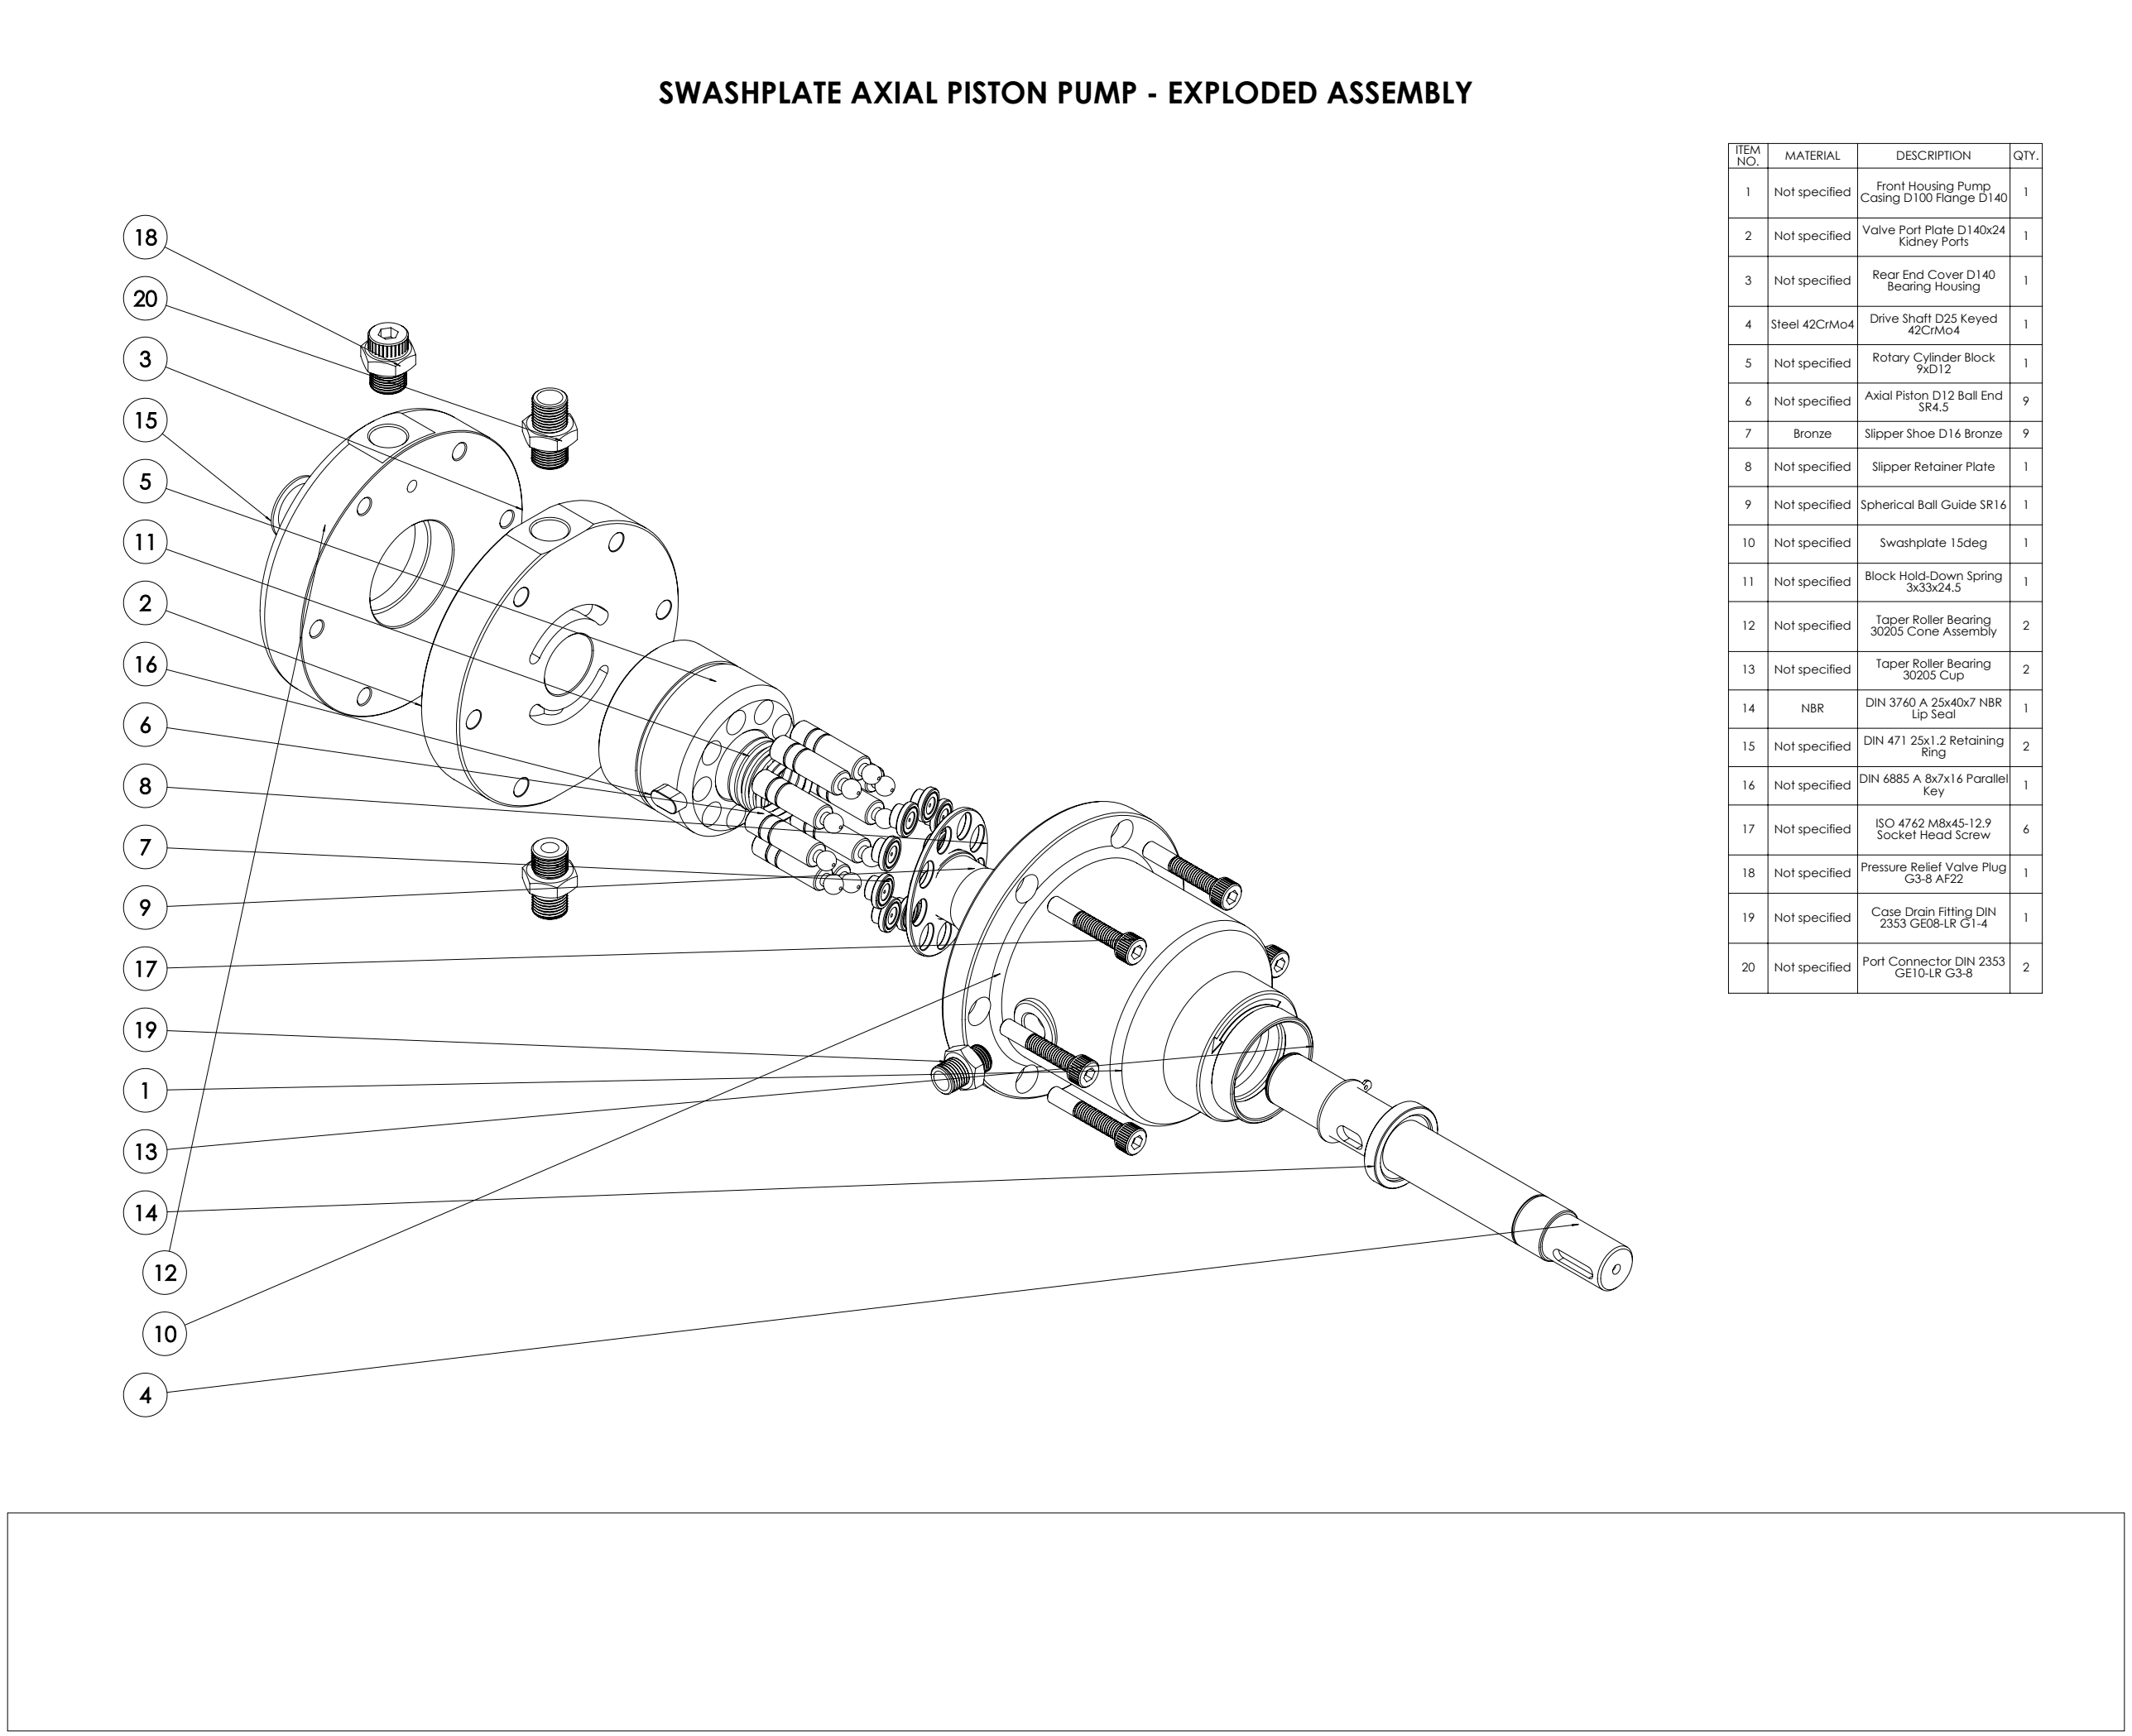
ISO-10303-21;
HEADER;
/* Generated by software containing ST-Developer
 * from STEP Tools, Inc. (www.steptools.com) 
 */

FILE_DESCRIPTION(
/* description */ (''),
/* implementation_level */ '2;1');

FILE_NAME(
/* name */ 'MAS-332',
/* time_stamp */ '2026-10-23T00:52:27+05:00',
/* author */ (''),
/* organization */ (''),
/* preprocessor_version */ 'ST-DEVELOPER v20.2',
/* originating_system */ 'Autodesk Translation Framework v15.15.0.0',
/* authorisation */ '');

FILE_SCHEMA (('AUTOMOTIVE_DESIGN { 1 0 10303 214 3 1 1 }'));
ENDSEC;

DATA;
#10=MECHANICAL_DESIGN_GEOMETRIC_PRESENTATION_REPRESENTATION('',(#1548,#1549,
#1550,#1551,#1552,#1553,#1554,#1555,#1556,#1557,#1558,#1559,#1560,#1561,
#1562,#1563,#1564,#1565,#1566,#1567,#1568,#1569,#1570,#1571,#1572,#1573,
#1574),#59204);
#11=ITEM_DEFINED_TRANSFORMATION($,$,#24159,#25071);
#12=ITEM_DEFINED_TRANSFORMATION($,$,#24197,#25072);
#13=ITEM_DEFINED_TRANSFORMATION($,$,#23046,#25073);
#14=ITEM_DEFINED_TRANSFORMATION($,$,#23123,#25074);
#15=ITEM_DEFINED_TRANSFORMATION($,$,#23145,#25075);
#16=ITEM_DEFINED_TRANSFORMATION($,$,#23166,#25076);
#17=ITEM_DEFINED_TRANSFORMATION($,$,#23174,#25077);
#18=ITEM_DEFINED_TRANSFORMATION($,$,#24636,#25078);
#19=ITEM_DEFINED_TRANSFORMATION($,$,#23191,#25079);
#20=ITEM_DEFINED_TRANSFORMATION($,$,#24231,#25080);
#21=ITEM_DEFINED_TRANSFORMATION($,$,#24619,#25081);
#22=ITEM_DEFINED_TRANSFORMATION($,$,#24661,#25082);
#23=ITEM_DEFINED_TRANSFORMATION($,$,#23228,#25083);
#24=ITEM_DEFINED_TRANSFORMATION($,$,#23491,#25084);
#25=ITEM_DEFINED_TRANSFORMATION($,$,#24996,#25085);
#26=ITEM_DEFINED_TRANSFORMATION($,$,#23559,#25086);
#27=ITEM_DEFINED_TRANSFORMATION($,$,#23609,#25087);
#28=ITEM_DEFINED_TRANSFORMATION($,$,#23720,#25088);
#29=ITEM_DEFINED_TRANSFORMATION($,$,#23866,#25089);
#30=ITEM_DEFINED_TRANSFORMATION($,$,#23996,#25090);
#31=ITEM_DEFINED_TRANSFORMATION($,$,#24159,#25091);
#32=ITEM_DEFINED_TRANSFORMATION($,$,#24159,#25092);
#33=ITEM_DEFINED_TRANSFORMATION($,$,#24159,#25093);
#34=ITEM_DEFINED_TRANSFORMATION($,$,#24159,#25094);
#35=ITEM_DEFINED_TRANSFORMATION($,$,#24159,#25095);
#36=ITEM_DEFINED_TRANSFORMATION($,$,#24159,#25096);
#37=ITEM_DEFINED_TRANSFORMATION($,$,#24159,#25097);
#38=ITEM_DEFINED_TRANSFORMATION($,$,#24159,#25098);
#39=ITEM_DEFINED_TRANSFORMATION($,$,#24197,#25099);
#40=ITEM_DEFINED_TRANSFORMATION($,$,#24197,#25100);
#41=ITEM_DEFINED_TRANSFORMATION($,$,#24197,#25101);
#42=ITEM_DEFINED_TRANSFORMATION($,$,#24197,#25102);
#43=ITEM_DEFINED_TRANSFORMATION($,$,#24197,#25103);
#44=ITEM_DEFINED_TRANSFORMATION($,$,#24197,#25104);
#45=ITEM_DEFINED_TRANSFORMATION($,$,#24197,#25105);
#46=ITEM_DEFINED_TRANSFORMATION($,$,#24197,#25106);
#47=ITEM_DEFINED_TRANSFORMATION($,$,#24231,#25107);
#48=ITEM_DEFINED_TRANSFORMATION($,$,#24619,#25108);
#49=ITEM_DEFINED_TRANSFORMATION($,$,#24636,#25109);
#50=ITEM_DEFINED_TRANSFORMATION($,$,#24661,#25110);
#51=ITEM_DEFINED_TRANSFORMATION($,$,#24661,#25111);
#52=ITEM_DEFINED_TRANSFORMATION($,$,#24661,#25112);
#53=ITEM_DEFINED_TRANSFORMATION($,$,#24661,#25113);
#54=ITEM_DEFINED_TRANSFORMATION($,$,#24661,#25114);
#55=ITEM_DEFINED_TRANSFORMATION($,$,#24996,#25115);
#56=(
REPRESENTATION_RELATIONSHIP($,$,#59310,#59296)
REPRESENTATION_RELATIONSHIP_WITH_TRANSFORMATION(#11)
SHAPE_REPRESENTATION_RELATIONSHIP()
);
#57=(
REPRESENTATION_RELATIONSHIP($,$,#59311,#59296)
REPRESENTATION_RELATIONSHIP_WITH_TRANSFORMATION(#12)
SHAPE_REPRESENTATION_RELATIONSHIP()
);
#58=(
REPRESENTATION_RELATIONSHIP($,$,#59297,#59296)
REPRESENTATION_RELATIONSHIP_WITH_TRANSFORMATION(#13)
SHAPE_REPRESENTATION_RELATIONSHIP()
);
#59=(
REPRESENTATION_RELATIONSHIP($,$,#59298,#59296)
REPRESENTATION_RELATIONSHIP_WITH_TRANSFORMATION(#14)
SHAPE_REPRESENTATION_RELATIONSHIP()
);
#60=(
REPRESENTATION_RELATIONSHIP($,$,#59299,#59296)
REPRESENTATION_RELATIONSHIP_WITH_TRANSFORMATION(#15)
SHAPE_REPRESENTATION_RELATIONSHIP()
);
#61=(
REPRESENTATION_RELATIONSHIP($,$,#59300,#59296)
REPRESENTATION_RELATIONSHIP_WITH_TRANSFORMATION(#16)
SHAPE_REPRESENTATION_RELATIONSHIP()
);
#62=(
REPRESENTATION_RELATIONSHIP($,$,#59301,#59296)
REPRESENTATION_RELATIONSHIP_WITH_TRANSFORMATION(#17)
SHAPE_REPRESENTATION_RELATIONSHIP()
);
#63=(
REPRESENTATION_RELATIONSHIP($,$,#59314,#59296)
REPRESENTATION_RELATIONSHIP_WITH_TRANSFORMATION(#18)
SHAPE_REPRESENTATION_RELATIONSHIP()
);
#64=(
REPRESENTATION_RELATIONSHIP($,$,#59302,#59296)
REPRESENTATION_RELATIONSHIP_WITH_TRANSFORMATION(#19)
SHAPE_REPRESENTATION_RELATIONSHIP()
);
#65=(
REPRESENTATION_RELATIONSHIP($,$,#59312,#59296)
REPRESENTATION_RELATIONSHIP_WITH_TRANSFORMATION(#20)
SHAPE_REPRESENTATION_RELATIONSHIP()
);
#66=(
REPRESENTATION_RELATIONSHIP($,$,#59313,#59296)
REPRESENTATION_RELATIONSHIP_WITH_TRANSFORMATION(#21)
SHAPE_REPRESENTATION_RELATIONSHIP()
);
#67=(
REPRESENTATION_RELATIONSHIP($,$,#59315,#59296)
REPRESENTATION_RELATIONSHIP_WITH_TRANSFORMATION(#22)
SHAPE_REPRESENTATION_RELATIONSHIP()
);
#68=(
REPRESENTATION_RELATIONSHIP($,$,#59303,#59296)
REPRESENTATION_RELATIONSHIP_WITH_TRANSFORMATION(#23)
SHAPE_REPRESENTATION_RELATIONSHIP()
);
#69=(
REPRESENTATION_RELATIONSHIP($,$,#59304,#59296)
REPRESENTATION_RELATIONSHIP_WITH_TRANSFORMATION(#24)
SHAPE_REPRESENTATION_RELATIONSHIP()
);
#70=(
REPRESENTATION_RELATIONSHIP($,$,#59316,#59296)
REPRESENTATION_RELATIONSHIP_WITH_TRANSFORMATION(#25)
SHAPE_REPRESENTATION_RELATIONSHIP()
);
#71=(
REPRESENTATION_RELATIONSHIP($,$,#59305,#59296)
REPRESENTATION_RELATIONSHIP_WITH_TRANSFORMATION(#26)
SHAPE_REPRESENTATION_RELATIONSHIP()
);
#72=(
REPRESENTATION_RELATIONSHIP($,$,#59306,#59296)
REPRESENTATION_RELATIONSHIP_WITH_TRANSFORMATION(#27)
SHAPE_REPRESENTATION_RELATIONSHIP()
);
#73=(
REPRESENTATION_RELATIONSHIP($,$,#59307,#59296)
REPRESENTATION_RELATIONSHIP_WITH_TRANSFORMATION(#28)
SHAPE_REPRESENTATION_RELATIONSHIP()
);
#74=(
REPRESENTATION_RELATIONSHIP($,$,#59308,#59296)
REPRESENTATION_RELATIONSHIP_WITH_TRANSFORMATION(#29)
SHAPE_REPRESENTATION_RELATIONSHIP()
);
#75=(
REPRESENTATION_RELATIONSHIP($,$,#59309,#59296)
REPRESENTATION_RELATIONSHIP_WITH_TRANSFORMATION(#30)
SHAPE_REPRESENTATION_RELATIONSHIP()
);
#76=(
REPRESENTATION_RELATIONSHIP($,$,#59310,#59296)
REPRESENTATION_RELATIONSHIP_WITH_TRANSFORMATION(#31)
SHAPE_REPRESENTATION_RELATIONSHIP()
);
#77=(
REPRESENTATION_RELATIONSHIP($,$,#59310,#59296)
REPRESENTATION_RELATIONSHIP_WITH_TRANSFORMATION(#32)
SHAPE_REPRESENTATION_RELATIONSHIP()
);
#78=(
REPRESENTATION_RELATIONSHIP($,$,#59310,#59296)
REPRESENTATION_RELATIONSHIP_WITH_TRANSFORMATION(#33)
SHAPE_REPRESENTATION_RELATIONSHIP()
);
#79=(
REPRESENTATION_RELATIONSHIP($,$,#59310,#59296)
REPRESENTATION_RELATIONSHIP_WITH_TRANSFORMATION(#34)
SHAPE_REPRESENTATION_RELATIONSHIP()
);
#80=(
REPRESENTATION_RELATIONSHIP($,$,#59310,#59296)
REPRESENTATION_RELATIONSHIP_WITH_TRANSFORMATION(#35)
SHAPE_REPRESENTATION_RELATIONSHIP()
);
#81=(
REPRESENTATION_RELATIONSHIP($,$,#59310,#59296)
REPRESENTATION_RELATIONSHIP_WITH_TRANSFORMATION(#36)
SHAPE_REPRESENTATION_RELATIONSHIP()
);
#82=(
REPRESENTATION_RELATIONSHIP($,$,#59310,#59296)
REPRESENTATION_RELATIONSHIP_WITH_TRANSFORMATION(#37)
SHAPE_REPRESENTATION_RELATIONSHIP()
);
#83=(
REPRESENTATION_RELATIONSHIP($,$,#59310,#59296)
REPRESENTATION_RELATIONSHIP_WITH_TRANSFORMATION(#38)
SHAPE_REPRESENTATION_RELATIONSHIP()
);
#84=(
REPRESENTATION_RELATIONSHIP($,$,#59311,#59296)
REPRESENTATION_RELATIONSHIP_WITH_TRANSFORMATION(#39)
SHAPE_REPRESENTATION_RELATIONSHIP()
);
#85=(
REPRESENTATION_RELATIONSHIP($,$,#59311,#59296)
REPRESENTATION_RELATIONSHIP_WITH_TRANSFORMATION(#40)
SHAPE_REPRESENTATION_RELATIONSHIP()
);
#86=(
REPRESENTATION_RELATIONSHIP($,$,#59311,#59296)
REPRESENTATION_RELATIONSHIP_WITH_TRANSFORMATION(#41)
SHAPE_REPRESENTATION_RELATIONSHIP()
);
#87=(
REPRESENTATION_RELATIONSHIP($,$,#59311,#59296)
REPRESENTATION_RELATIONSHIP_WITH_TRANSFORMATION(#42)
SHAPE_REPRESENTATION_RELATIONSHIP()
);
#88=(
REPRESENTATION_RELATIONSHIP($,$,#59311,#59296)
REPRESENTATION_RELATIONSHIP_WITH_TRANSFORMATION(#43)
SHAPE_REPRESENTATION_RELATIONSHIP()
);
#89=(
REPRESENTATION_RELATIONSHIP($,$,#59311,#59296)
REPRESENTATION_RELATIONSHIP_WITH_TRANSFORMATION(#44)
SHAPE_REPRESENTATION_RELATIONSHIP()
);
#90=(
REPRESENTATION_RELATIONSHIP($,$,#59311,#59296)
REPRESENTATION_RELATIONSHIP_WITH_TRANSFORMATION(#45)
SHAPE_REPRESENTATION_RELATIONSHIP()
);
#91=(
REPRESENTATION_RELATIONSHIP($,$,#59311,#59296)
REPRESENTATION_RELATIONSHIP_WITH_TRANSFORMATION(#46)
SHAPE_REPRESENTATION_RELATIONSHIP()
);
#92=(
REPRESENTATION_RELATIONSHIP($,$,#59312,#59296)
REPRESENTATION_RELATIONSHIP_WITH_TRANSFORMATION(#47)
SHAPE_REPRESENTATION_RELATIONSHIP()
);
#93=(
REPRESENTATION_RELATIONSHIP($,$,#59313,#59296)
REPRESENTATION_RELATIONSHIP_WITH_TRANSFORMATION(#48)
SHAPE_REPRESENTATION_RELATIONSHIP()
);
#94=(
REPRESENTATION_RELATIONSHIP($,$,#59314,#59296)
REPRESENTATION_RELATIONSHIP_WITH_TRANSFORMATION(#49)
SHAPE_REPRESENTATION_RELATIONSHIP()
);
#95=(
REPRESENTATION_RELATIONSHIP($,$,#59315,#59296)
REPRESENTATION_RELATIONSHIP_WITH_TRANSFORMATION(#50)
SHAPE_REPRESENTATION_RELATIONSHIP()
);
#96=(
REPRESENTATION_RELATIONSHIP($,$,#59315,#59296)
REPRESENTATION_RELATIONSHIP_WITH_TRANSFORMATION(#51)
SHAPE_REPRESENTATION_RELATIONSHIP()
);
#97=(
REPRESENTATION_RELATIONSHIP($,$,#59315,#59296)
REPRESENTATION_RELATIONSHIP_WITH_TRANSFORMATION(#52)
SHAPE_REPRESENTATION_RELATIONSHIP()
);
#98=(
REPRESENTATION_RELATIONSHIP($,$,#59315,#59296)
REPRESENTATION_RELATIONSHIP_WITH_TRANSFORMATION(#53)
SHAPE_REPRESENTATION_RELATIONSHIP()
);
#99=(
REPRESENTATION_RELATIONSHIP($,$,#59315,#59296)
REPRESENTATION_RELATIONSHIP_WITH_TRANSFORMATION(#54)
SHAPE_REPRESENTATION_RELATIONSHIP()
);
#100=(
REPRESENTATION_RELATIONSHIP($,$,#59316,#59296)
REPRESENTATION_RELATIONSHIP_WITH_TRANSFORMATION(#55)
SHAPE_REPRESENTATION_RELATIONSHIP()
);
#101=CONTEXT_DEPENDENT_SHAPE_REPRESENTATION(#56,#59251);
#102=CONTEXT_DEPENDENT_SHAPE_REPRESENTATION(#57,#59252);
#103=CONTEXT_DEPENDENT_SHAPE_REPRESENTATION(#58,#59253);
#104=CONTEXT_DEPENDENT_SHAPE_REPRESENTATION(#59,#59254);
#105=CONTEXT_DEPENDENT_SHAPE_REPRESENTATION(#60,#59255);
#106=CONTEXT_DEPENDENT_SHAPE_REPRESENTATION(#61,#59256);
#107=CONTEXT_DEPENDENT_SHAPE_REPRESENTATION(#62,#59257);
#108=CONTEXT_DEPENDENT_SHAPE_REPRESENTATION(#63,#59258);
#109=CONTEXT_DEPENDENT_SHAPE_REPRESENTATION(#64,#59259);
#110=CONTEXT_DEPENDENT_SHAPE_REPRESENTATION(#65,#59260);
#111=CONTEXT_DEPENDENT_SHAPE_REPRESENTATION(#66,#59261);
#112=CONTEXT_DEPENDENT_SHAPE_REPRESENTATION(#67,#59262);
#113=CONTEXT_DEPENDENT_SHAPE_REPRESENTATION(#68,#59263);
#114=CONTEXT_DEPENDENT_SHAPE_REPRESENTATION(#69,#59264);
#115=CONTEXT_DEPENDENT_SHAPE_REPRESENTATION(#70,#59265);
#116=CONTEXT_DEPENDENT_SHAPE_REPRESENTATION(#71,#59266);
#117=CONTEXT_DEPENDENT_SHAPE_REPRESENTATION(#72,#59267);
#118=CONTEXT_DEPENDENT_SHAPE_REPRESENTATION(#73,#59268);
#119=CONTEXT_DEPENDENT_SHAPE_REPRESENTATION(#74,#59269);
#120=CONTEXT_DEPENDENT_SHAPE_REPRESENTATION(#75,#59270);
#121=CONTEXT_DEPENDENT_SHAPE_REPRESENTATION(#76,#59271);
#122=CONTEXT_DEPENDENT_SHAPE_REPRESENTATION(#77,#59272);
#123=CONTEXT_DEPENDENT_SHAPE_REPRESENTATION(#78,#59273);
#124=CONTEXT_DEPENDENT_SHAPE_REPRESENTATION(#79,#59274);
#125=CONTEXT_DEPENDENT_SHAPE_REPRESENTATION(#80,#59275);
#126=CONTEXT_DEPENDENT_SHAPE_REPRESENTATION(#81,#59276);
#127=CONTEXT_DEPENDENT_SHAPE_REPRESENTATION(#82,#59277);
#128=CONTEXT_DEPENDENT_SHAPE_REPRESENTATION(#83,#59278);
#129=CONTEXT_DEPENDENT_SHAPE_REPRESENTATION(#84,#59279);
#130=CONTEXT_DEPENDENT_SHAPE_REPRESENTATION(#85,#59280);
#131=CONTEXT_DEPENDENT_SHAPE_REPRESENTATION(#86,#59281);
#132=CONTEXT_DEPENDENT_SHAPE_REPRESENTATION(#87,#59282);
#133=CONTEXT_DEPENDENT_SHAPE_REPRESENTATION(#88,#59283);
#134=CONTEXT_DEPENDENT_SHAPE_REPRESENTATION(#89,#59284);
#135=CONTEXT_DEPENDENT_SHAPE_REPRESENTATION(#90,#59285);
#136=CONTEXT_DEPENDENT_SHAPE_REPRESENTATION(#91,#59286);
#137=CONTEXT_DEPENDENT_SHAPE_REPRESENTATION(#92,#59287);
#138=CONTEXT_DEPENDENT_SHAPE_REPRESENTATION(#93,#59288);
#139=CONTEXT_DEPENDENT_SHAPE_REPRESENTATION(#94,#59289);
#140=CONTEXT_DEPENDENT_SHAPE_REPRESENTATION(#95,#59290);
#141=CONTEXT_DEPENDENT_SHAPE_REPRESENTATION(#96,#59291);
#142=CONTEXT_DEPENDENT_SHAPE_REPRESENTATION(#97,#59292);
#143=CONTEXT_DEPENDENT_SHAPE_REPRESENTATION(#98,#59293);
#144=CONTEXT_DEPENDENT_SHAPE_REPRESENTATION(#99,#59294);
#145=CONTEXT_DEPENDENT_SHAPE_REPRESENTATION(#100,#59295);
#146=NEXT_ASSEMBLY_USAGE_OCCURRENCE(
'06_Axial_Piston_D12_Ball_End_SR4.5:1',
'06_Axial_Piston_D12_Ball_End_SR4.5:1',
'06_Axial_Piston_D12_Ball_End_SR4.5:1',#59318,#59332,
'06_Axial_Piston_D12_Ball_End_SR4.5:1');
#147=NEXT_ASSEMBLY_USAGE_OCCURRENCE('07_Slipper_Shoe_D16_Bronze:1',
'07_Slipper_Shoe_D16_Bronze:1','07_Slipper_Shoe_D16_Bronze:1',#59318,#59333,
'07_Slipper_Shoe_D16_Bronze:1');
#148=NEXT_ASSEMBLY_USAGE_OCCURRENCE('08_Slipper_Retainer_Plate:1',
'08_Slipper_Retainer_Plate:1','08_Slipper_Retainer_Plate:1',#59318,#59319,
'08_Slipper_Retainer_Plate:1');
#149=NEXT_ASSEMBLY_USAGE_OCCURRENCE('09_Spherical_Ball_Guide_SR16:1',
'09_Spherical_Ball_Guide_SR16:1','09_Spherical_Ball_Guide_SR16:1',#59318,
#59320,'09_Spherical_Ball_Guide_SR16:1');
#150=NEXT_ASSEMBLY_USAGE_OCCURRENCE('10_Swashplate_15deg:1',
'10_Swashplate_15deg:1','10_Swashplate_15deg:1',#59318,#59321,
'10_Swashplate_15deg:1');
#151=NEXT_ASSEMBLY_USAGE_OCCURRENCE(
'11_Block_Hold-Down_Spring_3x33x24.5:1',
'11_Block_Hold-Down_Spring_3x33x24.5:1',
'11_Block_Hold-Down_Spring_3x33x24.5:1',#59318,#59322,
'11_Block_Hold-Down_Spring_3x33x24.5:1');
#152=NEXT_ASSEMBLY_USAGE_OCCURRENCE(
'16_DIN_6885_A_8x7x16_Parallel_Key:1',
'16_DIN_6885_A_8x7x16_Parallel_Key:1',
'16_DIN_6885_A_8x7x16_Parallel_Key:1',#59318,#59323,
'16_DIN_6885_A_8x7x16_Parallel_Key:1');
#153=NEXT_ASSEMBLY_USAGE_OCCURRENCE(
'15_DIN_471_25x1.2_Retaining_Ring:1',
'15_DIN_471_25x1.2_Retaining_Ring:1',
'15_DIN_471_25x1.2_Retaining_Ring:1',#59318,#59336,
'15_DIN_471_25x1.2_Retaining_Ring:1');
#154=NEXT_ASSEMBLY_USAGE_OCCURRENCE(
'14_DIN_3760_A_25x40x7_NBR_Lip_Seal:1',
'14_DIN_3760_A_25x40x7_NBR_Lip_Seal:1',
'14_DIN_3760_A_25x40x7_NBR_Lip_Seal:1',#59318,#59324,
'14_DIN_3760_A_25x40x7_NBR_Lip_Seal:1');
#155=NEXT_ASSEMBLY_USAGE_OCCURRENCE(
'12_Taper_Roller_Bearing_30205_Cone_Assembly:1',
'12_Taper_Roller_Bearing_30205_Cone_Assembly:1',
'12_Taper_Roller_Bearing_30205_Cone_Assembly:1',#59318,#59334,
'12_Taper_Roller_Bearing_30205_Cone_Assembly:1');
#156=NEXT_ASSEMBLY_USAGE_OCCURRENCE(
'13_Taper_Roller_Bearing_30205_Cup:1',
'13_Taper_Roller_Bearing_30205_Cup:1',
'13_Taper_Roller_Bearing_30205_Cup:1',#59318,#59335,
'13_Taper_Roller_Bearing_30205_Cup:1');
#157=NEXT_ASSEMBLY_USAGE_OCCURRENCE(
'17_ISO_4762_M8x45-12.9_Socket_Head_Screw:1',
'17_ISO_4762_M8x45-12.9_Socket_Head_Screw:1',
'17_ISO_4762_M8x45-12.9_Socket_Head_Screw:1',#59318,#59337,
'17_ISO_4762_M8x45-12.9_Socket_Head_Screw:1');
#158=NEXT_ASSEMBLY_USAGE_OCCURRENCE(
'18_Pressure_Relief_Valve_Plug_G3-8_AF22:1',
'18_Pressure_Relief_Valve_Plug_G3-8_AF22:1',
'18_Pressure_Relief_Valve_Plug_G3-8_AF22:1',#59318,#59325,
'18_Pressure_Relief_Valve_Plug_G3-8_AF22:1');
#159=NEXT_ASSEMBLY_USAGE_OCCURRENCE(
'19_Case_Drain_Fitting_DIN_2353_GE08-LR_G1-4:1',
'19_Case_Drain_Fitting_DIN_2353_GE08-LR_G1-4:1',
'19_Case_Drain_Fitting_DIN_2353_GE08-LR_G1-4:1',#59318,#59326,
'19_Case_Drain_Fitting_DIN_2353_GE08-LR_G1-4:1');
#160=NEXT_ASSEMBLY_USAGE_OCCURRENCE(
'20_Port_Connector_DIN_2353_GE10-LR_G3-8:1',
'20_Port_Connector_DIN_2353_GE10-LR_G3-8:1',
'20_Port_Connector_DIN_2353_GE10-LR_G3-8:1',#59318,#59338,
'20_Port_Connector_DIN_2353_GE10-LR_G3-8:1');
#161=NEXT_ASSEMBLY_USAGE_OCCURRENCE(
'04_Drive_Shaft_D25_Keyed_42CrMo4:1',
'04_Drive_Shaft_D25_Keyed_42CrMo4:1',
'04_Drive_Shaft_D25_Keyed_42CrMo4:1',#59318,#59327,
'04_Drive_Shaft_D25_Keyed_42CrMo4:1');
#162=NEXT_ASSEMBLY_USAGE_OCCURRENCE('05_Rotary_Cylinder_Block_9xD12:1',
'05_Rotary_Cylinder_Block_9xD12:1','05_Rotary_Cylinder_Block_9xD12:1',#59318,
#59328,'05_Rotary_Cylinder_Block_9xD12:1');
#163=NEXT_ASSEMBLY_USAGE_OCCURRENCE(
'01_Front_Housing_Pump_Casing_D100_Flange_D140:1',
'01_Front_Housing_Pump_Casing_D100_Flange_D140:1',
'01_Front_Housing_Pump_Casing_D100_Flange_D140:1',#59318,#59329,
'01_Front_Housing_Pump_Casing_D100_Flange_D140:1');
#164=NEXT_ASSEMBLY_USAGE_OCCURRENCE(
'02_Valve_Port_Plate_D140x24_Kidney_Ports:1',
'02_Valve_Port_Plate_D140x24_Kidney_Ports:1',
'02_Valve_Port_Plate_D140x24_Kidney_Ports:1',#59318,#59330,
'02_Valve_Port_Plate_D140x24_Kidney_Ports:1');
#165=NEXT_ASSEMBLY_USAGE_OCCURRENCE(
'03_Rear_End_Cover_D140_Bearing_Housing:1',
'03_Rear_End_Cover_D140_Bearing_Housing:1',
'03_Rear_End_Cover_D140_Bearing_Housing:1',#59318,#59331,
'03_Rear_End_Cover_D140_Bearing_Housing:1');
#166=NEXT_ASSEMBLY_USAGE_OCCURRENCE(
'06_Axial_Piston_D12_Ball_End_SR4.5:2',
'06_Axial_Piston_D12_Ball_End_SR4.5:2',
'06_Axial_Piston_D12_Ball_End_SR4.5:2',#59318,#59332,
'06_Axial_Piston_D12_Ball_End_SR4.5:2');
#167=NEXT_ASSEMBLY_USAGE_OCCURRENCE(
'06_Axial_Piston_D12_Ball_End_SR4.5:3',
'06_Axial_Piston_D12_Ball_End_SR4.5:3',
'06_Axial_Piston_D12_Ball_End_SR4.5:3',#59318,#59332,
'06_Axial_Piston_D12_Ball_End_SR4.5:3');
#168=NEXT_ASSEMBLY_USAGE_OCCURRENCE(
'06_Axial_Piston_D12_Ball_End_SR4.5:4',
'06_Axial_Piston_D12_Ball_End_SR4.5:4',
'06_Axial_Piston_D12_Ball_End_SR4.5:4',#59318,#59332,
'06_Axial_Piston_D12_Ball_End_SR4.5:4');
#169=NEXT_ASSEMBLY_USAGE_OCCURRENCE(
'06_Axial_Piston_D12_Ball_End_SR4.5:5',
'06_Axial_Piston_D12_Ball_End_SR4.5:5',
'06_Axial_Piston_D12_Ball_End_SR4.5:5',#59318,#59332,
'06_Axial_Piston_D12_Ball_End_SR4.5:5');
#170=NEXT_ASSEMBLY_USAGE_OCCURRENCE(
'06_Axial_Piston_D12_Ball_End_SR4.5:6',
'06_Axial_Piston_D12_Ball_End_SR4.5:6',
'06_Axial_Piston_D12_Ball_End_SR4.5:6',#59318,#59332,
'06_Axial_Piston_D12_Ball_End_SR4.5:6');
#171=NEXT_ASSEMBLY_USAGE_OCCURRENCE(
'06_Axial_Piston_D12_Ball_End_SR4.5:7',
'06_Axial_Piston_D12_Ball_End_SR4.5:7',
'06_Axial_Piston_D12_Ball_End_SR4.5:7',#59318,#59332,
'06_Axial_Piston_D12_Ball_End_SR4.5:7');
#172=NEXT_ASSEMBLY_USAGE_OCCURRENCE(
'06_Axial_Piston_D12_Ball_End_SR4.5:8',
'06_Axial_Piston_D12_Ball_End_SR4.5:8',
'06_Axial_Piston_D12_Ball_End_SR4.5:8',#59318,#59332,
'06_Axial_Piston_D12_Ball_End_SR4.5:8');
#173=NEXT_ASSEMBLY_USAGE_OCCURRENCE(
'06_Axial_Piston_D12_Ball_End_SR4.5:9',
'06_Axial_Piston_D12_Ball_End_SR4.5:9',
'06_Axial_Piston_D12_Ball_End_SR4.5:9',#59318,#59332,
'06_Axial_Piston_D12_Ball_End_SR4.5:9');
#174=NEXT_ASSEMBLY_USAGE_OCCURRENCE('07_Slipper_Shoe_D16_Bronze:2',
'07_Slipper_Shoe_D16_Bronze:2','07_Slipper_Shoe_D16_Bronze:2',#59318,#59333,
'07_Slipper_Shoe_D16_Bronze:2');
#175=NEXT_ASSEMBLY_USAGE_OCCURRENCE('07_Slipper_Shoe_D16_Bronze:3',
'07_Slipper_Shoe_D16_Bronze:3','07_Slipper_Shoe_D16_Bronze:3',#59318,#59333,
'07_Slipper_Shoe_D16_Bronze:3');
#176=NEXT_ASSEMBLY_USAGE_OCCURRENCE('07_Slipper_Shoe_D16_Bronze:4',
'07_Slipper_Shoe_D16_Bronze:4','07_Slipper_Shoe_D16_Bronze:4',#59318,#59333,
'07_Slipper_Shoe_D16_Bronze:4');
#177=NEXT_ASSEMBLY_USAGE_OCCURRENCE('07_Slipper_Shoe_D16_Bronze:5',
'07_Slipper_Shoe_D16_Bronze:5','07_Slipper_Shoe_D16_Bronze:5',#59318,#59333,
'07_Slipper_Shoe_D16_Bronze:5');
#178=NEXT_ASSEMBLY_USAGE_OCCURRENCE('07_Slipper_Shoe_D16_Bronze:6',
'07_Slipper_Shoe_D16_Bronze:6','07_Slipper_Shoe_D16_Bronze:6',#59318,#59333,
'07_Slipper_Shoe_D16_Bronze:6');
#179=NEXT_ASSEMBLY_USAGE_OCCURRENCE('07_Slipper_Shoe_D16_Bronze:7',
'07_Slipper_Shoe_D16_Bronze:7','07_Slipper_Shoe_D16_Bronze:7',#59318,#59333,
'07_Slipper_Shoe_D16_Bronze:7');
#180=NEXT_ASSEMBLY_USAGE_OCCURRENCE('07_Slipper_Shoe_D16_Bronze:8',
'07_Slipper_Shoe_D16_Bronze:8','07_Slipper_Shoe_D16_Bronze:8',#59318,#59333,
'07_Slipper_Shoe_D16_Bronze:8');
#181=NEXT_ASSEMBLY_USAGE_OCCURRENCE('07_Slipper_Shoe_D16_Bronze:9',
'07_Slipper_Shoe_D16_Bronze:9','07_Slipper_Shoe_D16_Bronze:9',#59318,#59333,
'07_Slipper_Shoe_D16_Bronze:9');
#182=NEXT_ASSEMBLY_USAGE_OCCURRENCE(
'12_Taper_Roller_Bearing_30205_Cone_Assembly:2',
'12_Taper_Roller_Bearing_30205_Cone_Assembly:2',
'12_Taper_Roller_Bearing_30205_Cone_Assembly:2',#59318,#59334,
'12_Taper_Roller_Bearing_30205_Cone_Assembly:2');
#183=NEXT_ASSEMBLY_USAGE_OCCURRENCE(
'13_Taper_Roller_Bearing_30205_Cup:2',
'13_Taper_Roller_Bearing_30205_Cup:2',
'13_Taper_Roller_Bearing_30205_Cup:2',#59318,#59335,
'13_Taper_Roller_Bearing_30205_Cup:2');
#184=NEXT_ASSEMBLY_USAGE_OCCURRENCE(
'15_DIN_471_25x1.2_Retaining_Ring:2',
'15_DIN_471_25x1.2_Retaining_Ring:2',
'15_DIN_471_25x1.2_Retaining_Ring:2',#59318,#59336,
'15_DIN_471_25x1.2_Retaining_Ring:2');
#185=NEXT_ASSEMBLY_USAGE_OCCURRENCE(
'17_ISO_4762_M8x45-12.9_Socket_Head_Screw:2',
'17_ISO_4762_M8x45-12.9_Socket_Head_Screw:2',
'17_ISO_4762_M8x45-12.9_Socket_Head_Screw:2',#59318,#59337,
'17_ISO_4762_M8x45-12.9_Socket_Head_Screw:2');
#186=NEXT_ASSEMBLY_USAGE_OCCURRENCE(
'17_ISO_4762_M8x45-12.9_Socket_Head_Screw:3',
'17_ISO_4762_M8x45-12.9_Socket_Head_Screw:3',
'17_ISO_4762_M8x45-12.9_Socket_Head_Screw:3',#59318,#59337,
'17_ISO_4762_M8x45-12.9_Socket_Head_Screw:3');
#187=NEXT_ASSEMBLY_USAGE_OCCURRENCE(
'17_ISO_4762_M8x45-12.9_Socket_Head_Screw:4',
'17_ISO_4762_M8x45-12.9_Socket_Head_Screw:4',
'17_ISO_4762_M8x45-12.9_Socket_Head_Screw:4',#59318,#59337,
'17_ISO_4762_M8x45-12.9_Socket_Head_Screw:4');
#188=NEXT_ASSEMBLY_USAGE_OCCURRENCE(
'17_ISO_4762_M8x45-12.9_Socket_Head_Screw:5',
'17_ISO_4762_M8x45-12.9_Socket_Head_Screw:5',
'17_ISO_4762_M8x45-12.9_Socket_Head_Screw:5',#59318,#59337,
'17_ISO_4762_M8x45-12.9_Socket_Head_Screw:5');
#189=NEXT_ASSEMBLY_USAGE_OCCURRENCE(
'17_ISO_4762_M8x45-12.9_Socket_Head_Screw:6',
'17_ISO_4762_M8x45-12.9_Socket_Head_Screw:6',
'17_ISO_4762_M8x45-12.9_Socket_Head_Screw:6',#59318,#59337,
'17_ISO_4762_M8x45-12.9_Socket_Head_Screw:6');
#190=NEXT_ASSEMBLY_USAGE_OCCURRENCE(
'20_Port_Connector_DIN_2353_GE10-LR_G3-8:2',
'20_Port_Connector_DIN_2353_GE10-LR_G3-8:2',
'20_Port_Connector_DIN_2353_GE10-LR_G3-8:2',#59318,#59338,
'20_Port_Connector_DIN_2353_GE10-LR_G3-8:2');
#191=ELLIPSE('',#24235,2.14723853173756,2.09817147851385);
#192=ELLIPSE('',#24236,1.89123203768515,1.8480150491299);
#193=ELLIPSE('',#24237,2.14723853173756,2.09817147851385);
#194=ELLIPSE('',#24238,1.89123203768515,1.8480150491299);
#195=ELLIPSE('',#24239,2.14723853173756,2.09817147851385);
#196=ELLIPSE('',#24240,1.89123203768515,1.8480150491299);
#197=ELLIPSE('',#24241,2.14723853173756,2.09817147851385);
#198=ELLIPSE('',#24242,1.89123203768515,1.8480150491299);
#199=ELLIPSE('',#24243,2.14723853173756,2.09817147851385);
#200=ELLIPSE('',#24244,1.89123203768515,1.8480150491299);
#201=ELLIPSE('',#24245,2.14723853173756,2.09817147851385);
#202=ELLIPSE('',#24246,1.89123203768515,1.8480150491299);
#203=ELLIPSE('',#24247,2.14723853173756,2.09817147851385);
#204=ELLIPSE('',#24248,1.89123203768515,1.8480150491299);
#205=ELLIPSE('',#24249,2.14723853173756,2.09817147851384);
#206=ELLIPSE('',#24250,1.89123203768515,1.8480150491299);
#207=ELLIPSE('',#24251,2.14723853173756,2.09817147851385);
#208=ELLIPSE('',#24252,1.89123203768515,1.8480150491299);
#209=ELLIPSE('',#24253,2.14723853173756,2.09817147851385);
#210=ELLIPSE('',#24254,1.89123203768515,1.8480150491299);
#211=ELLIPSE('',#24255,2.14723853173756,2.09817147851385);
#212=ELLIPSE('',#24256,1.89123203768515,1.8480150491299);
#213=ELLIPSE('',#24257,2.14723853173756,2.09817147851385);
#214=ELLIPSE('',#24258,1.89123203768515,1.8480150491299);
#215=ELLIPSE('',#24259,2.14723853173756,2.09817147851384);
#216=ELLIPSE('',#24260,1.89123203768515,1.8480150491299);
#217=ELLIPSE('',#24261,2.14723853173756,2.09817147851384);
#218=ELLIPSE('',#24262,1.89123203768515,1.8480150491299);
#219=ELLIPSE('',#24263,2.14723853173756,2.09817147851385);
#220=ELLIPSE('',#24264,1.89123203768515,1.8480150491299);
#221=ELLIPSE('',#24265,2.14723853173756,2.09817147851385);
#222=ELLIPSE('',#24266,1.89123203768515,1.8480150491299);
#223=ELLIPSE('',#24267,1.89123203768515,1.8480150491299);
#224=ELLIPSE('',#24268,2.14723853173756,2.09817147851385);
#225=ELLIPSE('',#24272,2.2310239828778,2.18004232858406);
#226=ELLIPSE('',#24273,1.97501748882539,1.92988589920012);
#227=ELLIPSE('',#24274,2.2310239828778,2.18004232858406);
#228=ELLIPSE('',#24275,1.97501748882539,1.92988589920012);
#229=ELLIPSE('',#24276,2.2310239828778,2.18004232858406);
#230=ELLIPSE('',#24277,1.97501748882539,1.92988589920012);
#231=ELLIPSE('',#24278,2.2310239828778,2.18004232858406);
#232=ELLIPSE('',#24279,1.97501748882539,1.92988589920012);
#233=ELLIPSE('',#24280,2.2310239828778,2.18004232858406);
#234=ELLIPSE('',#24281,1.97501748882539,1.92988589920012);
#235=ELLIPSE('',#24282,2.2310239828778,2.18004232858406);
#236=ELLIPSE('',#24283,1.9750174888254,1.92988589920012);
#237=ELLIPSE('',#24284,2.2310239828778,2.18004232858406);
#238=ELLIPSE('',#24285,1.97501748882539,1.92988589920012);
#239=ELLIPSE('',#24286,2.2310239828778,2.18004232858406);
#240=ELLIPSE('',#24287,1.97501748882539,1.92988589920012);
#241=ELLIPSE('',#24288,2.2310239828778,2.18004232858406);
#242=ELLIPSE('',#24289,1.97501748882539,1.92988589920012);
#243=ELLIPSE('',#24290,2.2310239828778,2.18004232858406);
#244=ELLIPSE('',#24291,1.97501748882539,1.92988589920012);
#245=ELLIPSE('',#24292,2.2310239828778,2.18004232858406);
#246=ELLIPSE('',#24293,1.97501748882539,1.92988589920012);
#247=ELLIPSE('',#24294,2.2310239828778,2.18004232858406);
#248=ELLIPSE('',#24295,1.97501748882539,1.92988589920012);
#249=ELLIPSE('',#24296,2.2310239828778,2.18004232858406);
#250=ELLIPSE('',#24297,1.97501748882539,1.92988589920012);
#251=ELLIPSE('',#24298,2.2310239828778,2.18004232858406);
#252=ELLIPSE('',#24299,1.97501748882539,1.92988589920012);
#253=ELLIPSE('',#24300,2.2310239828778,2.18004232858406);
#254=ELLIPSE('',#24301,1.97501748882539,1.92988589920012);
#255=ELLIPSE('',#24302,2.2310239828778,2.18004232858406);
#256=ELLIPSE('',#24303,1.97501748882539,1.92988589920012);
#257=ELLIPSE('',#24304,2.2310239828778,2.18004232858406);
#258=ELLIPSE('',#24305,1.97501748882539,1.92988589920012);
#259=ELLIPSE('',#24312,1.60810685188985,1.57186069047033);
#260=ELLIPSE('',#24318,0.349707645748017,0.3420563457837);
#261=ELLIPSE('',#24324,1.60810685188985,1.57186069047032);
#262=ELLIPSE('',#24330,0.349707645748017,0.3420563457837);
#263=ELLIPSE('',#24336,1.60810685188985,1.57186069047033);
#264=ELLIPSE('',#24342,0.349707645748017,0.3420563457837);
#265=ELLIPSE('',#24348,1.60810685188985,1.57186069047033);
#266=ELLIPSE('',#24354,0.349707645748017,0.3420563457837);
#267=ELLIPSE('',#24360,1.60810685188985,1.57186069047032);
#268=ELLIPSE('',#24366,0.349707645748018,0.3420563457837);
#269=ELLIPSE('',#24372,1.60810685188985,1.57186069047033);
#270=ELLIPSE('',#24378,0.349707645748017,0.3420563457837);
#271=ELLIPSE('',#24384,1.60810685188985,1.57186069047033);
#272=ELLIPSE('',#24390,0.349707645748017,0.3420563457837);
#273=ELLIPSE('',#24396,1.60810685188985,1.57186069047033);
#274=ELLIPSE('',#24402,0.349707645748017,0.3420563457837);
#275=ELLIPSE('',#24408,1.60810685188985,1.57186069047032);
#276=ELLIPSE('',#24414,0.349707645748017,0.3420563457837);
#277=ELLIPSE('',#24420,1.60810685188985,1.57186069047033);
#278=ELLIPSE('',#24426,0.349707645748018,0.3420563457837);
#279=ELLIPSE('',#24432,1.60810685188985,1.57186069047033);
#280=ELLIPSE('',#24438,0.349707645748017,0.3420563457837);
#281=ELLIPSE('',#24444,1.60810685188985,1.57186069047033);
#282=ELLIPSE('',#24450,0.349707645748017,0.3420563457837);
#283=ELLIPSE('',#24456,1.60810685188985,1.57186069047032);
#284=ELLIPSE('',#24462,0.349707645748017,0.3420563457837);
#285=ELLIPSE('',#24468,1.60810685188985,1.57186069047032);
#286=ELLIPSE('',#24474,0.349707645748017,0.3420563457837);
#287=ELLIPSE('',#24480,1.60810685188985,1.57186069047032);
#288=ELLIPSE('',#24486,0.349707645748017,0.3420563457837);
#289=ELLIPSE('',#24492,1.60810685188985,1.57186069047033);
#290=ELLIPSE('',#24498,0.349707645748017,0.3420563457837);
#291=ELLIPSE('',#24506,1.60810685188985,1.57186069047033);
#292=ELLIPSE('',#24511,0.349707645748017,0.3420563457837);
#293=ELLIPSE('',#24515,0.349707645748017,0.3420563457837);
#294=ELLIPSE('',#24539,0.349707645748017,0.3420563457837);
#295=ELLIPSE('',#24543,0.349707645748017,0.3420563457837);
#296=ELLIPSE('',#24547,0.349707645748017,0.3420563457837);
#297=ELLIPSE('',#24551,0.349707645748018,0.3420563457837);
#298=ELLIPSE('',#24555,0.349707645748017,0.3420563457837);
#299=ELLIPSE('',#24559,0.349707645748017,0.3420563457837);
#300=ELLIPSE('',#24563,0.349707645748017,0.3420563457837);
#301=ELLIPSE('',#24567,0.349707645748017,0.3420563457837);
#302=ELLIPSE('',#24571,0.349707645748018,0.3420563457837);
#303=ELLIPSE('',#24575,0.349707645748017,0.3420563457837);
#304=ELLIPSE('',#24579,0.349707645748017,0.3420563457837);
#305=ELLIPSE('',#24583,0.349707645748017,0.3420563457837);
#306=ELLIPSE('',#24587,0.349707645748017,0.3420563457837);
#307=ELLIPSE('',#24591,0.349707645748017,0.3420563457837);
#308=ELLIPSE('',#24595,0.349707645748017,0.3420563457837);
#309=ELLIPSE('',#24597,0.349707645748017,0.3420563457837);
#310=TOROIDAL_SURFACE('',#23784,5.4,0.4);
#311=TOROIDAL_SURFACE('',#23834,4.4,0.6);
#312=TOROIDAL_SURFACE('',#24105,6.3,0.7);
#313=TOROIDAL_SURFACE('',#24719,0.4333,0.04);
#314=B_SPLINE_SURFACE_WITH_KNOTS('',3,3,((#30941,#30942,#30943,#30944,#30945,
#30946,#30947,#30948,#30949,#30950),(#30951,#30952,#30953,#30954,#30955,
#30956,#30957,#30958,#30959,#30960),(#30961,#30962,#30963,#30964,#30965,
#30966,#30967,#30968,#30969,#30970),(#30971,#30972,#30973,#30974,#30975,
#30976,#30977,#30978,#30979,#30980)),.UNSPECIFIED.,.F.,.F.,.F.,(4,4),(4,
1,1,1,1,1,1,4),(0.,1.),(0.0830596749235681,0.519992957590172,0.956926240256775,
1.39385952292338,1.83079280558998,2.26772608825659,2.70465937092319,3.14159265358979),
 .UNSPECIFIED.);
#315=B_SPLINE_SURFACE_WITH_KNOTS('',3,3,((#31030,#31031,#31032,#31033,#31034,
#31035,#31036,#31037,#31038,#31039),(#31040,#31041,#31042,#31043,#31044,
#31045,#31046,#31047,#31048,#31049),(#31050,#31051,#31052,#31053,#31054,
#31055,#31056,#31057,#31058,#31059),(#31060,#31061,#31062,#31063,#31064,
#31065,#31066,#31067,#31068,#31069)),.UNSPECIFIED.,.F.,.F.,.F.,(4,4),(4,
1,1,1,1,1,1,4),(0.,1.),(-3.14159265358979,-2.70465937092292,-2.26772608825605,
-1.83079280558918,-1.39385952292231,-0.95692624025544,-0.519992957588569,
-0.083059674921698),.UNSPECIFIED.);
#316=B_SPLINE_SURFACE_WITH_KNOTS('',3,3,((#31111,#31112,#31113,#31114,#31115,
#31116,#31117,#31118,#31119,#31120,#31121,#31122,#31123,#31124,#31125,#31126,
#31127),(#31128,#31129,#31130,#31131,#31132,#31133,#31134,#31135,#31136,
#31137,#31138,#31139,#31140,#31141,#31142,#31143,#31144),(#31145,#31146,
#31147,#31148,#31149,#31150,#31151,#31152,#31153,#31154,#31155,#31156,#31157,
#31158,#31159,#31160,#31161),(#31162,#31163,#31164,#31165,#31166,#31167,
#31168,#31169,#31170,#31171,#31172,#31173,#31174,#31175,#31176,#31177,#31178)),
 .UNSPECIFIED.,.F.,.T.,.F.,(4,4),(4,1,1,1,1,1,1,1,1,1,1,1,1,1,4),(0.,1.),
(-3.14159265358979,-2.69279370307697,-2.24399475256414,-1.79519580205131,
-1.34639685153848,-1.0471975511966,-0.448798950512828,-0.149599650170943,
0.448798950512828,0.747998250854713,1.34639685153848,1.64559615188037,2.24399475256414,
2.69279370307697,3.14159265358979),.UNSPECIFIED.);
#317=B_SPLINE_SURFACE_WITH_KNOTS('',3,3,((#31275,#31276,#31277,#31278,#31279,
#31280,#31281,#31282,#31283,#31284,#31285,#31286,#31287,#31288,#31289,#31290,
#31291,#31292,#31293,#31294,#31295,#31296,#31297,#31298,#31299,#31300,#31301,
#31302,#31303,#31304,#31305,#31306,#31307,#31308,#31309,#31310,#31311,#31312,
#31313,#31314,#31315,#31316,#31317,#31318,#31319,#31320,#31321,#31322,#31323,
#31324,#31325,#31326,#31327,#31328,#31329,#31330,#31331,#31332,#31333,#31334,
#31335,#31336,#31337,#31338,#31339,#31340,#31341,#31342,#31343,#31344,#31345,
#31346,#31347,#31348,#31349,#31350,#31351,#31352,#31353,#31354,#31355,#31356,
#31357),(#31358,#31359,#31360,#31361,#31362,#31363,#31364,#31365,#31366,
#31367,#31368,#31369,#31370,#31371,#31372,#31373,#31374,#31375,#31376,#31377,
#31378,#31379,#31380,#31381,#31382,#31383,#31384,#31385,#31386,#31387,#31388,
#31389,#31390,#31391,#31392,#31393,#31394,#31395,#31396,#31397,#31398,#31399,
#31400,#31401,#31402,#31403,#31404,#31405,#31406,#31407,#31408,#31409,#31410,
#31411,#31412,#31413,#31414,#31415,#31416,#31417,#31418,#31419,#31420,#31421,
#31422,#31423,#31424,#31425,#31426,#31427,#31428,#31429,#31430,#31431,#31432,
#31433,#31434,#31435,#31436,#31437,#31438,#31439,#31440),(#31441,#31442,
#31443,#31444,#31445,#31446,#31447,#31448,#31449,#31450,#31451,#31452,#31453,
#31454,#31455,#31456,#31457,#31458,#31459,#31460,#31461,#31462,#31463,#31464,
#31465,#31466,#31467,#31468,#31469,#31470,#31471,#31472,#31473,#31474,#31475,
#31476,#31477,#31478,#31479,#31480,#31481,#31482,#31483,#31484,#31485,#31486,
#31487,#31488,#31489,#31490,#31491,#31492,#31493,#31494,#31495,#31496,#31497,
#31498,#31499,#31500,#31501,#31502,#31503,#31504,#31505,#31506,#31507,#31508,
#31509,#31510,#31511,#31512,#31513,#31514,#31515,#31516,#31517,#31518,#31519,
#31520,#31521,#31522,#31523),(#31524,#31525,#31526,#31527,#31528,#31529,
#31530,#31531,#31532,#31533,#31534,#31535,#31536,#31537,#31538,#31539,#31540,
#31541,#31542,#31543,#31544,#31545,#31546,#31547,#31548,#31549,#31550,#31551,
#31552,#31553,#31554,#31555,#31556,#31557,#31558,#31559,#31560,#31561,#31562,
#31563,#31564,#31565,#31566,#31567,#31568,#31569,#31570,#31571,#31572,#31573,
#31574,#31575,#31576,#31577,#31578,#31579,#31580,#31581,#31582,#31583,#31584,
#31585,#31586,#31587,#31588,#31589,#31590,#31591,#31592,#31593,#31594,#31595,
#31596,#31597,#31598,#31599,#31600,#31601,#31602,#31603,#31604,#31605,#31606),
(#31607,#31608,#31609,#31610,#31611,#31612,#31613,#31614,#31615,#31616,
#31617,#31618,#31619,#31620,#31621,#31622,#31623,#31624,#31625,#31626,#31627,
#31628,#31629,#31630,#31631,#31632,#31633,#31634,#31635,#31636,#31637,#31638,
#31639,#31640,#31641,#31642,#31643,#31644,#31645,#31646,#31647,#31648,#31649,
#31650,#31651,#31652,#31653,#31654,#31655,#31656,#31657,#31658,#31659,#31660,
#31661,#31662,#31663,#31664,#31665,#31666,#31667,#31668,#31669,#31670,#31671,
#31672,#31673,#31674,#31675,#31676,#31677,#31678,#31679,#31680,#31681,#31682,
#31683,#31684,#31685,#31686,#31687,#31688,#31689),(#31690,#31691,#31692,
#31693,#31694,#31695,#31696,#31697,#31698,#31699,#31700,#31701,#31702,#31703,
#31704,#31705,#31706,#31707,#31708,#31709,#31710,#31711,#31712,#31713,#31714,
#31715,#31716,#31717,#31718,#31719,#31720,#31721,#31722,#31723,#31724,#31725,
#31726,#31727,#31728,#31729,#31730,#31731,#31732,#31733,#31734,#31735,#31736,
#31737,#31738,#31739,#31740,#31741,#31742,#31743,#31744,#31745,#31746,#31747,
#31748,#31749,#31750,#31751,#31752,#31753,#31754,#31755,#31756,#31757,#31758,
#31759,#31760,#31761,#31762,#31763,#31764,#31765,#31766,#31767,#31768,#31769,
#31770,#31771,#31772),(#31773,#31774,#31775,#31776,#31777,#31778,#31779,
#31780,#31781,#31782,#31783,#31784,#31785,#31786,#31787,#31788,#31789,#31790,
#31791,#31792,#31793,#31794,#31795,#31796,#31797,#31798,#31799,#31800,#31801,
#31802,#31803,#31804,#31805,#31806,#31807,#31808,#31809,#31810,#31811,#31812,
#31813,#31814,#31815,#31816,#31817,#31818,#31819,#31820,#31821,#31822,#31823,
#31824,#31825,#31826,#31827,#31828,#31829,#31830,#31831,#31832,#31833,#31834,
#31835,#31836,#31837,#31838,#31839,#31840,#31841,#31842,#31843,#31844,#31845,
#31846,#31847,#31848,#31849,#31850,#31851,#31852,#31853,#31854,#31855),
(#31856,#31857,#31858,#31859,#31860,#31861,#31862,#31863,#31864,#31865,
#31866,#31867,#31868,#31869,#31870,#31871,#31872,#31873,#31874,#31875,#31876,
#31877,#31878,#31879,#31880,#31881,#31882,#31883,#31884,#31885,#31886,#31887,
#31888,#31889,#31890,#31891,#31892,#31893,#31894,#31895,#31896,#31897,#31898,
#31899,#31900,#31901,#31902,#31903,#31904,#31905,#31906,#31907,#31908,#31909,
#31910,#31911,#31912,#31913,#31914,#31915,#31916,#31917,#31918,#31919,#31920,
#31921,#31922,#31923,#31924,#31925,#31926,#31927,#31928,#31929,#31930,#31931,
#31932,#31933,#31934,#31935,#31936,#31937,#31938),(#31939,#31940,#31941,
#31942,#31943,#31944,#31945,#31946,#31947,#31948,#31949,#31950,#31951,#31952,
#31953,#31954,#31955,#31956,#31957,#31958,#31959,#31960,#31961,#31962,#31963,
#31964,#31965,#31966,#31967,#31968,#31969,#31970,#31971,#31972,#31973,#31974,
#31975,#31976,#31977,#31978,#31979,#31980,#31981,#31982,#31983,#31984,#31985,
#31986,#31987,#31988,#31989,#31990,#31991,#31992,#31993,#31994,#31995,#31996,
#31997,#31998,#31999,#32000,#32001,#32002,#32003,#32004,#32005,#32006,#32007,
#32008,#32009,#32010,#32011,#32012,#32013,#32014,#32015,#32016,#32017,#32018,
#32019,#32020,#32021),(#32022,#32023,#32024,#32025,#32026,#32027,#32028,
#32029,#32030,#32031,#32032,#32033,#32034,#32035,#32036,#32037,#32038,#32039,
#32040,#32041,#32042,#32043,#32044,#32045,#32046,#32047,#32048,#32049,#32050,
#32051,#32052,#32053,#32054,#32055,#32056,#32057,#32058,#32059,#32060,#32061,
#32062,#32063,#32064,#32065,#32066,#32067,#32068,#32069,#32070,#32071,#32072,
#32073,#32074,#32075,#32076,#32077,#32078,#32079,#32080,#32081,#32082,#32083,
#32084,#32085,#32086,#32087,#32088,#32089,#32090,#32091,#32092,#32093,#32094,
#32095,#32096,#32097,#32098,#32099,#32100,#32101,#32102,#32103,#32104)),
 .UNSPECIFIED.,.T.,.F.,.F.,(4,1,1,1,1,1,1,4),(4,1,1,1,1,1,1,1,1,1,1,1,1,
1,1,1,1,1,1,1,1,1,1,1,1,1,1,1,1,1,1,1,1,1,1,1,1,1,1,1,1,1,1,1,1,1,1,1,1,
1,1,1,1,1,1,1,1,1,1,1,1,1,1,1,1,1,1,1,1,1,1,1,1,1,1,1,1,1,1,1,4),(-3.14159265358979,
-2.24399475256414,-1.34639685153848,-0.448798950512828,0.448798950512828,
1.34639685153848,2.24399475256414,3.14159265358979),(0.,0.00892857142857143,
0.0178571428571429,0.0267857142857143,0.0357142857142857,0.0535714285714286,
0.0714285714285714,0.0892857142857143,0.107142857142857,0.125,0.133928571428571,
0.142857142857143,0.158730158730159,0.174603174603175,0.19047619047619,
0.202380952380952,0.214285714285714,0.226190476190476,0.238095238095238,
0.25,0.261904761904762,0.273809523809524,0.279761904761905,0.285714285714286,
0.297619047619048,0.30952380952381,0.321428571428571,0.333333333333333,
0.349206349206349,0.365079365079365,0.373015873015873,0.380952380952381,
0.396825396825397,0.412698412698413,0.428571428571429,0.444444444444444,
0.46031746031746,0.476190476190476,0.492063492063492,0.507936507936508,
0.523809523809524,0.535714285714286,0.547619047619048,0.55952380952381,
0.571428571428571,0.583333333333333,0.595238095238095,0.607142857142857,
0.619047619047619,0.630952380952381,0.642857142857143,0.654761904761905,
0.666666666666667,0.682539682539682,0.698412698412698,0.706349206349206,
0.714285714285714,0.722222222222222,0.73015873015873,0.746031746031746,
0.761904761904762,0.773809523809524,0.785714285714286,0.797619047619047,
0.809523809523809,0.821428571428571,0.833333333333333,0.845238095238095,
0.857142857142857,0.861607142857143,0.866071428571429,0.875,0.892857142857143,
0.910714285714286,0.928571428571429,0.946428571428571,0.964285714285714,
0.973214285714286,0.982142857142857,0.991071428571429,1.),.UNSPECIFIED.);
#318=B_SPLINE_SURFACE_WITH_KNOTS('',3,3,((#32590,#32591,#32592,#32593,#32594,
#32595,#32596,#32597,#32598,#32599,#32600,#32601,#32602,#32603,#32604,#32605,
#32606,#32607,#32608,#32609,#32610,#32611,#32612,#32613,#32614,#32615,#32616,
#32617,#32618,#32619,#32620,#32621,#32622,#32623,#32624,#32625,#32626,#32627,
#32628,#32629,#32630,#32631,#32632,#32633,#32634,#32635,#32636,#32637,#32638,
#32639,#32640,#32641,#32642,#32643,#32644,#32645,#32646,#32647,#32648,#32649,
#32650,#32651,#32652,#32653,#32654,#32655,#32656,#32657,#32658,#32659,#32660,
#32661,#32662,#32663,#32664,#32665,#32666,#32667,#32668,#32669,#32670,#32671,
#32672,#32673,#32674,#32675,#32676,#32677,#32678,#32679,#32680,#32681,#32682,
#32683,#32684,#32685,#32686,#32687,#32688,#32689,#32690),(#32691,#32692,
#32693,#32694,#32695,#32696,#32697,#32698,#32699,#32700,#32701,#32702,#32703,
#32704,#32705,#32706,#32707,#32708,#32709,#32710,#32711,#32712,#32713,#32714,
#32715,#32716,#32717,#32718,#32719,#32720,#32721,#32722,#32723,#32724,#32725,
#32726,#32727,#32728,#32729,#32730,#32731,#32732,#32733,#32734,#32735,#32736,
#32737,#32738,#32739,#32740,#32741,#32742,#32743,#32744,#32745,#32746,#32747,
#32748,#32749,#32750,#32751,#32752,#32753,#32754,#32755,#32756,#32757,#32758,
#32759,#32760,#32761,#32762,#32763,#32764,#32765,#32766,#32767,#32768,#32769,
#32770,#32771,#32772,#32773,#32774,#32775,#32776,#32777,#32778,#32779,#32780,
#32781,#32782,#32783,#32784,#32785,#32786,#32787,#32788,#32789,#32790,#32791),
(#32792,#32793,#32794,#32795,#32796,#32797,#32798,#32799,#32800,#32801,
#32802,#32803,#32804,#32805,#32806,#32807,#32808,#32809,#32810,#32811,#32812,
#32813,#32814,#32815,#32816,#32817,#32818,#32819,#32820,#32821,#32822,#32823,
#32824,#32825,#32826,#32827,#32828,#32829,#32830,#32831,#32832,#32833,#32834,
#32835,#32836,#32837,#32838,#32839,#32840,#32841,#32842,#32843,#32844,#32845,
#32846,#32847,#32848,#32849,#32850,#32851,#32852,#32853,#32854,#32855,#32856,
#32857,#32858,#32859,#32860,#32861,#32862,#32863,#32864,#32865,#32866,#32867,
#32868,#32869,#32870,#32871,#32872,#32873,#32874,#32875,#32876,#32877,#32878,
#32879,#32880,#32881,#32882,#32883,#32884,#32885,#32886,#32887,#32888,#32889,
#32890,#32891,#32892),(#32893,#32894,#32895,#32896,#32897,#32898,#32899,
#32900,#32901,#32902,#32903,#32904,#32905,#32906,#32907,#32908,#32909,#32910,
#32911,#32912,#32913,#32914,#32915,#32916,#32917,#32918,#32919,#32920,#32921,
#32922,#32923,#32924,#32925,#32926,#32927,#32928,#32929,#32930,#32931,#32932,
#32933,#32934,#32935,#32936,#32937,#32938,#32939,#32940,#32941,#32942,#32943,
#32944,#32945,#32946,#32947,#32948,#32949,#32950,#32951,#32952,#32953,#32954,
#32955,#32956,#32957,#32958,#32959,#32960,#32961,#32962,#32963,#32964,#32965,
#32966,#32967,#32968,#32969,#32970,#32971,#32972,#32973,#32974,#32975,#32976,
#32977,#32978,#32979,#32980,#32981,#32982,#32983,#32984,#32985,#32986,#32987,
#32988,#32989,#32990,#32991,#32992,#32993),(#32994,#32995,#32996,#32997,
#32998,#32999,#33000,#33001,#33002,#33003,#33004,#33005,#33006,#33007,#33008,
#33009,#33010,#33011,#33012,#33013,#33014,#33015,#33016,#33017,#33018,#33019,
#33020,#33021,#33022,#33023,#33024,#33025,#33026,#33027,#33028,#33029,#33030,
#33031,#33032,#33033,#33034,#33035,#33036,#33037,#33038,#33039,#33040,#33041,
#33042,#33043,#33044,#33045,#33046,#33047,#33048,#33049,#33050,#33051,#33052,
#33053,#33054,#33055,#33056,#33057,#33058,#33059,#33060,#33061,#33062,#33063,
#33064,#33065,#33066,#33067,#33068,#33069,#33070,#33071,#33072,#33073,#33074,
#33075,#33076,#33077,#33078,#33079,#33080,#33081,#33082,#33083,#33084,#33085,
#33086,#33087,#33088,#33089,#33090,#33091,#33092,#33093,#33094)),
 .UNSPECIFIED.,.F.,.F.,.F.,(4,1,4),(4,1,1,1,1,1,1,1,1,1,1,1,1,1,1,1,1,1,
1,1,1,1,1,1,1,1,1,1,1,1,1,1,1,1,1,1,1,1,1,1,1,1,1,1,1,1,1,1,1,1,1,1,1,1,
1,1,1,1,1,1,1,1,1,1,1,1,1,1,1,1,1,1,1,1,1,1,1,1,1,1,1,1,1,1,1,1,1,1,1,1,
1,1,1,1,1,1,1,1,4),(0.,0.467498906784196,1.09083078249646),(6.28318530717956,
6.77358368901884,7.26398207085813,7.75438045269741,8.24477883453669,8.73517721637598,
9.22557559821526,9.71597398005454,10.2063723618938,10.6967707437331,11.1871691255724,
11.6775675074117,12.167965889251,12.6583642710902,13.1487626529295,13.6391610347688,
14.1295594166081,14.6199577984474,15.1103561802867,15.6007545621259,16.0911529439652,
16.5815513258045,17.0719497076438,17.5623480894831,18.0527464713224,18.5431448531616,
19.0335432350009,19.5239416168402,20.0143399986795,20.5047383805188,20.9951367623581,
21.4855351441973,21.9759335260366,22.4663319078759,22.9567302897152,23.4471286715545,
23.9375270533938,24.427925435233,24.9183238170723,25.4087221989116,25.8991205807509,
26.3895189625902,26.8799173444295,27.3703157262687,27.860714108108,28.3511124899473,
28.8415108717866,29.3319092536259,29.8223076354652,30.3127060173044,30.8031043991437,
31.293502780983,31.7839011628223,32.2742995446616,32.7646979265009,33.2550963083402,
33.7454946901794,34.2358930720187,34.726291453858,35.2166898356973,35.7070882175366,
36.1974865993759,36.6878849812151,37.1782833630544,37.6686817448937,38.159080126733,
38.6494785085723,39.1398768904116,39.6302752722508,40.1206736540901,40.6110720359294,
41.1014704177687,41.591868799608,42.0822671814473,42.5726655632865,43.0630639451258,
43.5534623269651,44.0438607088044,44.5342590906437,45.024657472483,45.5150558543222,
46.0054542361615,46.4958526180008,46.9862509998401,47.4766493816794,47.9670477635187,
48.4574461453579,48.9478445271972,49.4382429090365,49.9286412908758,50.4190396727151,
50.9094380545544,51.3998364363936,51.8902348182329,52.3806332000722,52.8710315819115,
53.3614299637508,53.8518283455901,54.3422267274293),.UNSPECIFIED.);
#319=B_SPLINE_SURFACE_WITH_KNOTS('',3,3,((#33507,#33508,#33509,#33510,#33511,
#33512,#33513,#33514,#33515,#33516,#33517,#33518,#33519,#33520,#33521,#33522,
#33523,#33524,#33525,#33526,#33527,#33528,#33529,#33530,#33531,#33532,#33533,
#33534,#33535,#33536,#33537,#33538,#33539,#33540,#33541,#33542,#33543,#33544,
#33545,#33546,#33547,#33548,#33549,#33550,#33551,#33552,#33553,#33554,#33555,
#33556,#33557,#33558,#33559,#33560,#33561,#33562,#33563,#33564,#33565,#33566,
#33567,#33568,#33569,#33570,#33571,#33572,#33573,#33574,#33575,#33576,#33577,
#33578,#33579,#33580,#33581,#33582,#33583,#33584,#33585,#33586,#33587,#33588,
#33589,#33590,#33591,#33592,#33593,#33594,#33595,#33596,#33597,#33598,#33599,
#33600,#33601,#33602,#33603,#33604,#33605,#33606,#33607),(#33608,#33609,
#33610,#33611,#33612,#33613,#33614,#33615,#33616,#33617,#33618,#33619,#33620,
#33621,#33622,#33623,#33624,#33625,#33626,#33627,#33628,#33629,#33630,#33631,
#33632,#33633,#33634,#33635,#33636,#33637,#33638,#33639,#33640,#33641,#33642,
#33643,#33644,#33645,#33646,#33647,#33648,#33649,#33650,#33651,#33652,#33653,
#33654,#33655,#33656,#33657,#33658,#33659,#33660,#33661,#33662,#33663,#33664,
#33665,#33666,#33667,#33668,#33669,#33670,#33671,#33672,#33673,#33674,#33675,
#33676,#33677,#33678,#33679,#33680,#33681,#33682,#33683,#33684,#33685,#33686,
#33687,#33688,#33689,#33690,#33691,#33692,#33693,#33694,#33695,#33696,#33697,
#33698,#33699,#33700,#33701,#33702,#33703,#33704,#33705,#33706,#33707,#33708),
(#33709,#33710,#33711,#33712,#33713,#33714,#33715,#33716,#33717,#33718,
#33719,#33720,#33721,#33722,#33723,#33724,#33725,#33726,#33727,#33728,#33729,
#33730,#33731,#33732,#33733,#33734,#33735,#33736,#33737,#33738,#33739,#33740,
#33741,#33742,#33743,#33744,#33745,#33746,#33747,#33748,#33749,#33750,#33751,
#33752,#33753,#33754,#33755,#33756,#33757,#33758,#33759,#33760,#33761,#33762,
#33763,#33764,#33765,#33766,#33767,#33768,#33769,#33770,#33771,#33772,#33773,
#33774,#33775,#33776,#33777,#33778,#33779,#33780,#33781,#33782,#33783,#33784,
#33785,#33786,#33787,#33788,#33789,#33790,#33791,#33792,#33793,#33794,#33795,
#33796,#33797,#33798,#33799,#33800,#33801,#33802,#33803,#33804,#33805,#33806,
#33807,#33808,#33809),(#33810,#33811,#33812,#33813,#33814,#33815,#33816,
#33817,#33818,#33819,#33820,#33821,#33822,#33823,#33824,#33825,#33826,#33827,
#33828,#33829,#33830,#33831,#33832,#33833,#33834,#33835,#33836,#33837,#33838,
#33839,#33840,#33841,#33842,#33843,#33844,#33845,#33846,#33847,#33848,#33849,
#33850,#33851,#33852,#33853,#33854,#33855,#33856,#33857,#33858,#33859,#33860,
#33861,#33862,#33863,#33864,#33865,#33866,#33867,#33868,#33869,#33870,#33871,
#33872,#33873,#33874,#33875,#33876,#33877,#33878,#33879,#33880,#33881,#33882,
#33883,#33884,#33885,#33886,#33887,#33888,#33889,#33890,#33891,#33892,#33893,
#33894,#33895,#33896,#33897,#33898,#33899,#33900,#33901,#33902,#33903,#33904,
#33905,#33906,#33907,#33908,#33909,#33910)),.UNSPECIFIED.,.F.,.F.,.F.,(4,
4),(4,1,1,1,1,1,1,1,1,1,1,1,1,1,1,1,1,1,1,1,1,1,1,1,1,1,1,1,1,1,1,1,1,1,
1,1,1,1,1,1,1,1,1,1,1,1,1,1,1,1,1,1,1,1,1,1,1,1,1,1,1,1,1,1,1,1,1,1,1,1,
1,1,1,1,1,1,1,1,1,1,1,1,1,1,1,1,1,1,1,1,1,1,1,1,1,1,1,1,4),(0.,0.0671853436149873),
(7.04827039213813,7.54574010072062,8.04320980930311,8.5406795178856,9.03814922646809,
9.53561893505058,10.0330886436331,10.5305583522156,11.0280280607981,11.5254977693805,
12.022967477963,12.5204371865455,13.017906895128,13.5153766037105,14.012846312293,
14.5103160208755,15.007785729458,15.5052554380405,16.002725146623,16.5001948552054,
16.9976645637879,17.4951342723704,17.9926039809529,18.4900736895354,18.9875433981179,
19.4850131067004,19.9824828152829,20.4799525238654,20.9774222324479,21.4748919410303,
21.9723616496128,22.4698313581953,22.9673010667778,23.4647707753603,23.9622404839428,
24.4597101925253,24.9571799011078,25.4546496096903,25.9521193182728,26.4495890268552,
26.9470587354377,27.4445284440202,27.9419981526027,28.4394678611852,28.9369375697677,
29.4344072783502,29.9318769869327,30.4293466955152,30.9268164040977,31.4242861126801,
31.9217558212626,32.4192255298451,32.9166952384276,33.4141649470101,33.9116346555926,
34.4091043641751,34.9065740727576,35.4040437813401,35.9015134899225,36.398983198505,
36.8964529070875,37.39392261567,37.8913923242525,38.388862032835,38.8863317414175,
39.38380145,39.8812711585825,40.378740867165,40.8762105757474,41.3736802843299,
41.8711499929124,42.3686197014949,42.8660894100774,43.3635591186599,43.8610288272424,
44.3584985358249,44.8559682444074,45.3534379529899,45.8509076615723,46.3483773701548,
46.8458470787373,47.3433167873198,47.8407864959023,48.3382562044848,48.8357259130673,
49.3331956216498,49.8306653302323,50.3281350388148,50.8256047473972,51.3230744559797,
51.8205441645622,52.3180138731447,52.8154835817272,53.3129532903097,53.8104229988922,
54.3078927074747,54.8053624160572,55.3028321246397,55.8003018332221),
 .UNSPECIFIED.);
#320=B_SPLINE_SURFACE_WITH_KNOTS('',3,3,((#34113,#34114,#34115,#34116,#34117,
#34118,#34119,#34120,#34121,#34122,#34123,#34124,#34125,#34126,#34127,#34128,
#34129,#34130,#34131,#34132,#34133,#34134,#34135,#34136,#34137,#34138,#34139,
#34140,#34141,#34142,#34143,#34144,#34145,#34146,#34147,#34148,#34149,#34150,
#34151,#34152,#34153,#34154,#34155,#34156,#34157,#34158,#34159,#34160,#34161,
#34162,#34163,#34164,#34165,#34166,#34167,#34168,#34169,#34170,#34171,#34172,
#34173,#34174,#34175,#34176,#34177,#34178,#34179,#34180,#34181,#34182,#34183,
#34184,#34185,#34186,#34187,#34188,#34189,#34190,#34191,#34192,#34193,#34194,
#34195,#34196,#34197,#34198,#34199,#34200,#34201,#34202,#34203,#34204,#34205,
#34206,#34207,#34208,#34209,#34210,#34211,#34212,#34213),(#34214,#34215,
#34216,#34217,#34218,#34219,#34220,#34221,#34222,#34223,#34224,#34225,#34226,
#34227,#34228,#34229,#34230,#34231,#34232,#34233,#34234,#34235,#34236,#34237,
#34238,#34239,#34240,#34241,#34242,#34243,#34244,#34245,#34246,#34247,#34248,
#34249,#34250,#34251,#34252,#34253,#34254,#34255,#34256,#34257,#34258,#34259,
#34260,#34261,#34262,#34263,#34264,#34265,#34266,#34267,#34268,#34269,#34270,
#34271,#34272,#34273,#34274,#34275,#34276,#34277,#34278,#34279,#34280,#34281,
#34282,#34283,#34284,#34285,#34286,#34287,#34288,#34289,#34290,#34291,#34292,
#34293,#34294,#34295,#34296,#34297,#34298,#34299,#34300,#34301,#34302,#34303,
#34304,#34305,#34306,#34307,#34308,#34309,#34310,#34311,#34312,#34313,#34314),
(#34315,#34316,#34317,#34318,#34319,#34320,#34321,#34322,#34323,#34324,
#34325,#34326,#34327,#34328,#34329,#34330,#34331,#34332,#34333,#34334,#34335,
#34336,#34337,#34338,#34339,#34340,#34341,#34342,#34343,#34344,#34345,#34346,
#34347,#34348,#34349,#34350,#34351,#34352,#34353,#34354,#34355,#34356,#34357,
#34358,#34359,#34360,#34361,#34362,#34363,#34364,#34365,#34366,#34367,#34368,
#34369,#34370,#34371,#34372,#34373,#34374,#34375,#34376,#34377,#34378,#34379,
#34380,#34381,#34382,#34383,#34384,#34385,#34386,#34387,#34388,#34389,#34390,
#34391,#34392,#34393,#34394,#34395,#34396,#34397,#34398,#34399,#34400,#34401,
#34402,#34403,#34404,#34405,#34406,#34407,#34408,#34409,#34410,#34411,#34412,
#34413,#34414,#34415),(#34416,#34417,#34418,#34419,#34420,#34421,#34422,
#34423,#34424,#34425,#34426,#34427,#34428,#34429,#34430,#34431,#34432,#34433,
#34434,#34435,#34436,#34437,#34438,#34439,#34440,#34441,#34442,#34443,#34444,
#34445,#34446,#34447,#34448,#34449,#34450,#34451,#34452,#34453,#34454,#34455,
#34456,#34457,#34458,#34459,#34460,#34461,#34462,#34463,#34464,#34465,#34466,
#34467,#34468,#34469,#34470,#34471,#34472,#34473,#34474,#34475,#34476,#34477,
#34478,#34479,#34480,#34481,#34482,#34483,#34484,#34485,#34486,#34487,#34488,
#34489,#34490,#34491,#34492,#34493,#34494,#34495,#34496,#34497,#34498,#34499,
#34500,#34501,#34502,#34503,#34504,#34505,#34506,#34507,#34508,#34509,#34510,
#34511,#34512,#34513,#34514,#34515,#34516),(#34517,#34518,#34519,#34520,
#34521,#34522,#34523,#34524,#34525,#34526,#34527,#34528,#34529,#34530,#34531,
#34532,#34533,#34534,#34535,#34536,#34537,#34538,#34539,#34540,#34541,#34542,
#34543,#34544,#34545,#34546,#34547,#34548,#34549,#34550,#34551,#34552,#34553,
#34554,#34555,#34556,#34557,#34558,#34559,#34560,#34561,#34562,#34563,#34564,
#34565,#34566,#34567,#34568,#34569,#34570,#34571,#34572,#34573,#34574,#34575,
#34576,#34577,#34578,#34579,#34580,#34581,#34582,#34583,#34584,#34585,#34586,
#34587,#34588,#34589,#34590,#34591,#34592,#34593,#34594,#34595,#34596,#34597,
#34598,#34599,#34600,#34601,#34602,#34603,#34604,#34605,#34606,#34607,#34608,
#34609,#34610,#34611,#34612,#34613,#34614,#34615,#34616,#34617)),
 .UNSPECIFIED.,.F.,.F.,.F.,(4,1,4),(4,1,1,1,1,1,1,1,1,1,1,1,1,1,1,1,1,1,
1,1,1,1,1,1,1,1,1,1,1,1,1,1,1,1,1,1,1,1,1,1,1,1,1,1,1,1,1,1,1,1,1,1,1,1,
1,1,1,1,1,1,1,1,1,1,1,1,1,1,1,1,1,1,1,1,1,1,1,1,1,1,1,1,1,1,1,1,1,1,1,1,
1,1,1,1,1,1,1,1,4),(0.,0.467498906784196,1.09083078249646),(8.50634549793094,
8.99674387977022,9.48714226160951,9.97754064344879,10.4679390252881,10.9583374071274,
11.4487357889666,11.9391341708059,12.4295325526452,12.9199309344845,13.4103293163238,
13.9007276981631,14.3911260800023,14.8815244618416,15.3719228436809,15.8623212255202,
16.3527196073595,16.8431179891988,17.333516371038,17.8239147528773,18.3143131347166,
18.8047115165559,19.2951098983952,19.7855082802345,20.2759066620737,20.766305043913,
21.2567034257523,21.7471018075916,22.2375001894309,22.7278985712702,23.2182969531094,
23.7086953349487,24.199093716788,24.6894920986273,25.1798904804666,25.6702888623059,
26.1606872441451,26.6510856259844,27.1414840078237,27.631882389663,28.1222807715023,
28.6126791533416,29.1030775351808,29.5934759170201,30.0838742988594,30.5742726806987,
31.064671062538,31.5550694443773,32.0454678262165,32.5358662080558,33.0262645898951,
33.5166629717344,34.0070613535737,34.497459735413,34.9878581172523,35.4782564990915,
35.9686548809308,36.4590532627701,36.9494516446094,37.4398500264487,37.930248408288,
38.4206467901272,38.9110451719665,39.4014435538058,39.8918419356451,40.3822403174844,
40.8726386993237,41.3630370811629,41.8534354630022,42.3438338448415,42.8342322266808,
43.3246306085201,43.8150289903594,44.3054273721986,44.7958257540379,45.2862241358772,
45.7766225177165,46.2670208995558,46.7574192813951,47.2478176632343,47.7382160450736,
48.2286144269129,48.7190128087522,49.2094111905915,49.6998095724308,50.19020795427,
50.6806063361093,51.1710047179486,51.6614030997879,52.1518014816272,52.6421998634665,
53.1325982453057,53.622996627145,54.1133950089843,54.6037933908236,55.0941917726629,
55.5845901545022,56.0749885363414,56.5653869181807),.UNSPECIFIED.);
#321=B_SPLINE_SURFACE_WITH_KNOTS('',3,3,((#34710,#34711,#34712,#34713,#34714,
#34715,#34716,#34717,#34718,#34719,#34720,#34721,#34722,#34723,#34724,#34725,
#34726,#34727,#34728,#34729,#34730,#34731,#34732,#34733,#34734,#34735,#34736,
#34737,#34738,#34739,#34740,#34741,#34742,#34743,#34744,#34745,#34746,#34747,
#34748,#34749,#34750,#34751,#34752,#34753,#34754,#34755,#34756,#34757,#34758,
#34759,#34760,#34761,#34762,#34763,#34764,#34765,#34766,#34767,#34768,#34769,
#34770,#34771,#34772,#34773,#34774,#34775,#34776,#34777,#34778,#34779,#34780,
#34781,#34782,#34783,#34784,#34785,#34786,#34787,#34788,#34789,#34790,#34791,
#34792,#34793,#34794,#34795,#34796,#34797,#34798,#34799,#34800,#34801,#34802,
#34803,#34804,#34805,#34806,#34807,#34808,#34809,#34810),(#34811,#34812,
#34813,#34814,#34815,#34816,#34817,#34818,#34819,#34820,#34821,#34822,#34823,
#34824,#34825,#34826,#34827,#34828,#34829,#34830,#34831,#34832,#34833,#34834,
#34835,#34836,#34837,#34838,#34839,#34840,#34841,#34842,#34843,#34844,#34845,
#34846,#34847,#34848,#34849,#34850,#34851,#34852,#34853,#34854,#34855,#34856,
#34857,#34858,#34859,#34860,#34861,#34862,#34863,#34864,#34865,#34866,#34867,
#34868,#34869,#34870,#34871,#34872,#34873,#34874,#34875,#34876,#34877,#34878,
#34879,#34880,#34881,#34882,#34883,#34884,#34885,#34886,#34887,#34888,#34889,
#34890,#34891,#34892,#34893,#34894,#34895,#34896,#34897,#34898,#34899,#34900,
#34901,#34902,#34903,#34904,#34905,#34906,#34907,#34908,#34909,#34910,#34911),
(#34912,#34913,#34914,#34915,#34916,#34917,#34918,#34919,#34920,#34921,
#34922,#34923,#34924,#34925,#34926,#34927,#34928,#34929,#34930,#34931,#34932,
#34933,#34934,#34935,#34936,#34937,#34938,#34939,#34940,#34941,#34942,#34943,
#34944,#34945,#34946,#34947,#34948,#34949,#34950,#34951,#34952,#34953,#34954,
#34955,#34956,#34957,#34958,#34959,#34960,#34961,#34962,#34963,#34964,#34965,
#34966,#34967,#34968,#34969,#34970,#34971,#34972,#34973,#34974,#34975,#34976,
#34977,#34978,#34979,#34980,#34981,#34982,#34983,#34984,#34985,#34986,#34987,
#34988,#34989,#34990,#34991,#34992,#34993,#34994,#34995,#34996,#34997,#34998,
#34999,#35000,#35001,#35002,#35003,#35004,#35005,#35006,#35007,#35008,#35009,
#35010,#35011,#35012),(#35013,#35014,#35015,#35016,#35017,#35018,#35019,
#35020,#35021,#35022,#35023,#35024,#35025,#35026,#35027,#35028,#35029,#35030,
#35031,#35032,#35033,#35034,#35035,#35036,#35037,#35038,#35039,#35040,#35041,
#35042,#35043,#35044,#35045,#35046,#35047,#35048,#35049,#35050,#35051,#35052,
#35053,#35054,#35055,#35056,#35057,#35058,#35059,#35060,#35061,#35062,#35063,
#35064,#35065,#35066,#35067,#35068,#35069,#35070,#35071,#35072,#35073,#35074,
#35075,#35076,#35077,#35078,#35079,#35080,#35081,#35082,#35083,#35084,#35085,
#35086,#35087,#35088,#35089,#35090,#35091,#35092,#35093,#35094,#35095,#35096,
#35097,#35098,#35099,#35100,#35101,#35102,#35103,#35104,#35105,#35106,#35107,
#35108,#35109,#35110,#35111,#35112,#35113),(#35114,#35115,#35116,#35117,
#35118,#35119,#35120,#35121,#35122,#35123,#35124,#35125,#35126,#35127,#35128,
#35129,#35130,#35131,#35132,#35133,#35134,#35135,#35136,#35137,#35138,#35139,
#35140,#35141,#35142,#35143,#35144,#35145,#35146,#35147,#35148,#35149,#35150,
#35151,#35152,#35153,#35154,#35155,#35156,#35157,#35158,#35159,#35160,#35161,
#35162,#35163,#35164,#35165,#35166,#35167,#35168,#35169,#35170,#35171,#35172,
#35173,#35174,#35175,#35176,#35177,#35178,#35179,#35180,#35181,#35182,#35183,
#35184,#35185,#35186,#35187,#35188,#35189,#35190,#35191,#35192,#35193,#35194,
#35195,#35196,#35197,#35198,#35199,#35200,#35201,#35202,#35203,#35204,#35205,
#35206,#35207,#35208,#35209,#35210,#35211,#35212,#35213,#35214)),
 .UNSPECIFIED.,.F.,.F.,.F.,(4,1,4),(4,1,1,1,1,1,1,1,1,1,1,1,1,1,1,1,1,1,
1,1,1,1,1,1,1,1,1,1,1,1,1,1,1,1,1,1,1,1,1,1,1,1,1,1,1,1,1,1,1,1,1,1,1,1,
1,1,1,1,1,1,1,1,1,1,1,1,1,1,1,1,1,1,1,1,1,1,1,1,1,1,1,1,1,1,1,1,1,1,1,1,
1,1,1,1,1,1,1,1,4),(-1.09083078249646,-0.623331875712262,0.),(9.57812533864918,
10.0685237204885,10.5589221023278,11.049320484167,11.5397188660063,12.0301172478456,
12.5205156296849,13.0109140115242,13.5013123933635,13.9917107752027,14.482109157042,
14.9725075388813,15.4629059207206,15.9533043025599,16.4437026843992,16.9341010662384,
17.4244994480777,17.914897829917,18.4052962117563,18.8956945935956,19.3860929754349,
19.8764913572741,20.3668897391134,20.8572881209527,21.347686502792,21.8380848846313,
22.3284832664706,22.8188816483098,23.3092800301491,23.7996784119884,24.2900767938277,
24.780475175667,25.2708735575063,25.7612719393455,26.2516703211848,26.7420687030241,
27.2324670848634,27.7228654667027,28.213263848542,28.7036622303812,29.1940606122205,
29.6844589940598,30.1748573758991,30.6652557577384,31.1556541395777,31.6460525214169,
32.1364509032562,32.6268492850955,33.1172476669348,33.6076460487741,34.0980444306134,
34.5884428124526,35.0788411942919,35.5692395761312,36.0596379579705,36.5500363398098,
37.0404347216491,37.5308331034883,38.0212314853276,38.5116298671669,39.0020282490062,
39.4924266308455,39.9828250126848,40.473223394524,40.9636217763633,41.4540201582026,
41.9444185400419,42.4348169218812,42.9252153037205,43.4156136855597,43.906012067399,
44.3964104492383,44.8868088310776,45.3772072129169,45.8676055947562,46.3580039765954,
46.8484023584347,47.338800740274,47.8291991221133,48.3195975039526,48.8099958857919,
49.3003942676311,49.7907926494704,50.2811910313097,50.771589413149,51.2619877949883,
51.7523861768276,52.2427845586669,52.7331829405061,53.2235813223454,53.7139797041847,
54.204378086024,54.6947764678633,55.1851748497025,55.6755732315418,56.1659716133811,
56.6563699952204,57.1467683770597,57.637166758899),.UNSPECIFIED.);
#322=B_SPLINE_SURFACE_WITH_KNOTS('',3,3,((#35322,#35323,#35324,#35325,#35326,
#35327,#35328,#35329,#35330,#35331,#35332,#35333,#35334,#35335,#35336,#35337,
#35338,#35339,#35340,#35341,#35342,#35343,#35344,#35345,#35346,#35347,#35348,
#35349,#35350,#35351,#35352,#35353,#35354,#35355,#35356,#35357,#35358,#35359,
#35360,#35361,#35362,#35363,#35364,#35365,#35366,#35367,#35368,#35369,#35370,
#35371,#35372,#35373,#35374,#35375,#35376,#35377,#35378,#35379,#35380,#35381,
#35382,#35383,#35384,#35385,#35386,#35387,#35388,#35389,#35390,#35391,#35392,
#35393,#35394,#35395,#35396,#35397,#35398,#35399,#35400,#35401,#35402,#35403,
#35404,#35405,#35406,#35407,#35408,#35409,#35410,#35411,#35412,#35413,#35414,
#35415,#35416,#35417,#35418,#35419,#35420,#35421,#35422),(#35423,#35424,
#35425,#35426,#35427,#35428,#35429,#35430,#35431,#35432,#35433,#35434,#35435,
#35436,#35437,#35438,#35439,#35440,#35441,#35442,#35443,#35444,#35445,#35446,
#35447,#35448,#35449,#35450,#35451,#35452,#35453,#35454,#35455,#35456,#35457,
#35458,#35459,#35460,#35461,#35462,#35463,#35464,#35465,#35466,#35467,#35468,
#35469,#35470,#35471,#35472,#35473,#35474,#35475,#35476,#35477,#35478,#35479,
#35480,#35481,#35482,#35483,#35484,#35485,#35486,#35487,#35488,#35489,#35490,
#35491,#35492,#35493,#35494,#35495,#35496,#35497,#35498,#35499,#35500,#35501,
#35502,#35503,#35504,#35505,#35506,#35507,#35508,#35509,#35510,#35511,#35512,
#35513,#35514,#35515,#35516,#35517,#35518,#35519,#35520,#35521,#35522,#35523),
(#35524,#35525,#35526,#35527,#35528,#35529,#35530,#35531,#35532,#35533,
#35534,#35535,#35536,#35537,#35538,#35539,#35540,#35541,#35542,#35543,#35544,
#35545,#35546,#35547,#35548,#35549,#35550,#35551,#35552,#35553,#35554,#35555,
#35556,#35557,#35558,#35559,#35560,#35561,#35562,#35563,#35564,#35565,#35566,
#35567,#35568,#35569,#35570,#35571,#35572,#35573,#35574,#35575,#35576,#35577,
#35578,#35579,#35580,#35581,#35582,#35583,#35584,#35585,#35586,#35587,#35588,
#35589,#35590,#35591,#35592,#35593,#35594,#35595,#35596,#35597,#35598,#35599,
#35600,#35601,#35602,#35603,#35604,#35605,#35606,#35607,#35608,#35609,#35610,
#35611,#35612,#35613,#35614,#35615,#35616,#35617,#35618,#35619,#35620,#35621,
#35622,#35623,#35624),(#35625,#35626,#35627,#35628,#35629,#35630,#35631,
#35632,#35633,#35634,#35635,#35636,#35637,#35638,#35639,#35640,#35641,#35642,
#35643,#35644,#35645,#35646,#35647,#35648,#35649,#35650,#35651,#35652,#35653,
#35654,#35655,#35656,#35657,#35658,#35659,#35660,#35661,#35662,#35663,#35664,
#35665,#35666,#35667,#35668,#35669,#35670,#35671,#35672,#35673,#35674,#35675,
#35676,#35677,#35678,#35679,#35680,#35681,#35682,#35683,#35684,#35685,#35686,
#35687,#35688,#35689,#35690,#35691,#35692,#35693,#35694,#35695,#35696,#35697,
#35698,#35699,#35700,#35701,#35702,#35703,#35704,#35705,#35706,#35707,#35708,
#35709,#35710,#35711,#35712,#35713,#35714,#35715,#35716,#35717,#35718,#35719,
#35720,#35721,#35722,#35723,#35724,#35725)),.UNSPECIFIED.,.F.,.F.,.F.,(4,
4),(4,1,1,1,1,1,1,1,1,1,1,1,1,1,1,1,1,1,1,1,1,1,1,1,1,1,1,1,1,1,1,1,1,1,
1,1,1,1,1,1,1,1,1,1,1,1,1,1,1,1,1,1,1,1,1,1,1,1,1,1,1,1,1,1,1,1,1,1,1,1,
1,1,1,1,1,1,1,1,1,1,1,1,1,1,1,1,1,1,1,1,1,1,1,1,1,1,1,1,4),(0.,0.0671853436149873),
(10.3432104236078,10.8406801321902,11.3381498407727,11.8356195493552,12.3330892579377,
12.8305589665202,13.3280286751027,13.8254983836852,14.3229680922677,14.8204378008502,
15.3179075094327,15.8153772180151,16.3128469265976,16.8103166351801,17.3077863437626,
17.8052560523451,18.3027257609276,18.8001954695101,19.2976651780926,19.7951348866751,
20.2926045952576,20.79007430384,21.2875440124225,21.785013721005,22.2824834295875,
22.77995313817,23.2774228467525,23.774892555335,24.2723622639175,24.7698319725,
25.2673016810825,25.7647713896649,26.2622410982474,26.7597108068299,27.2571805154124,
27.7546502239949,28.2521199325774,28.7495896411599,29.2470593497424,29.7445290583249,
30.2419987669074,30.7394684754899,31.2369381840723,31.7344078926548,32.2318776012373,
32.7293473098198,33.2268170184023,33.7242867269848,34.2217564355673,34.7192261441498,
35.2166958527323,35.7141655613148,36.2116352698972,36.7091049784797,37.2065746870622,
37.7040443956447,38.2015141042272,38.6989838128097,39.1964535213922,39.6939232299747,
40.1913929385572,40.6888626471397,41.1863323557221,41.6838020643046,42.1812717728871,
42.6787414814696,43.1762111900521,43.6736808986346,44.1711506072171,44.6686203157996,
45.1660900243821,45.6635597329645,46.161029441547,46.6584991501295,47.155968858712,
47.6534385672945,48.150908275877,48.6483779844595,49.145847693042,49.6433174016245,
50.140787110207,50.6382568187894,51.1357265273719,51.6331962359544,52.1306659445369,
52.6281356531194,53.1256053617019,53.6230750702844,54.1205447788669,54.6180144874494,
55.1154841960319,55.6129539046143,56.1104236131968,56.6078933217793,57.1053630303618,
57.6028327389443,58.1003024475268,58.5977721561093,59.0952418646918),
 .UNSPECIFIED.);
#323=B_SPLINE_SURFACE_WITH_KNOTS('',3,3,((#35878,#35879,#35880,#35881,#35882,
#35883,#35884,#35885,#35886,#35887,#35888,#35889,#35890,#35891,#35892,#35893,
#35894,#35895,#35896,#35897,#35898,#35899,#35900,#35901,#35902,#35903,#35904,
#35905,#35906,#35907,#35908,#35909,#35910,#35911,#35912,#35913,#35914,#35915,
#35916,#35917,#35918,#35919,#35920,#35921,#35922,#35923,#35924,#35925,#35926,
#35927,#35928,#35929,#35930,#35931,#35932,#35933,#35934,#35935,#35936,#35937,
#35938,#35939,#35940,#35941,#35942,#35943,#35944,#35945,#35946,#35947,#35948,
#35949,#35950,#35951,#35952,#35953,#35954,#35955,#35956,#35957,#35958,#35959,
#35960,#35961,#35962,#35963,#35964,#35965,#35966,#35967,#35968,#35969,#35970,
#35971,#35972,#35973,#35974,#35975,#35976,#35977,#35978),(#35979,#35980,
#35981,#35982,#35983,#35984,#35985,#35986,#35987,#35988,#35989,#35990,#35991,
#35992,#35993,#35994,#35995,#35996,#35997,#35998,#35999,#36000,#36001,#36002,
#36003,#36004,#36005,#36006,#36007,#36008,#36009,#36010,#36011,#36012,#36013,
#36014,#36015,#36016,#36017,#36018,#36019,#36020,#36021,#36022,#36023,#36024,
#36025,#36026,#36027,#36028,#36029,#36030,#36031,#36032,#36033,#36034,#36035,
#36036,#36037,#36038,#36039,#36040,#36041,#36042,#36043,#36044,#36045,#36046,
#36047,#36048,#36049,#36050,#36051,#36052,#36053,#36054,#36055,#36056,#36057,
#36058,#36059,#36060,#36061,#36062,#36063,#36064,#36065,#36066,#36067,#36068,
#36069,#36070,#36071,#36072,#36073,#36074,#36075,#36076,#36077,#36078,#36079),
(#36080,#36081,#36082,#36083,#36084,#36085,#36086,#36087,#36088,#36089,
#36090,#36091,#36092,#36093,#36094,#36095,#36096,#36097,#36098,#36099,#36100,
#36101,#36102,#36103,#36104,#36105,#36106,#36107,#36108,#36109,#36110,#36111,
#36112,#36113,#36114,#36115,#36116,#36117,#36118,#36119,#36120,#36121,#36122,
#36123,#36124,#36125,#36126,#36127,#36128,#36129,#36130,#36131,#36132,#36133,
#36134,#36135,#36136,#36137,#36138,#36139,#36140,#36141,#36142,#36143,#36144,
#36145,#36146,#36147,#36148,#36149,#36150,#36151,#36152,#36153,#36154,#36155,
#36156,#36157,#36158,#36159,#36160,#36161,#36162,#36163,#36164,#36165,#36166,
#36167,#36168,#36169,#36170,#36171,#36172,#36173,#36174,#36175,#36176,#36177,
#36178,#36179,#36180),(#36181,#36182,#36183,#36184,#36185,#36186,#36187,
#36188,#36189,#36190,#36191,#36192,#36193,#36194,#36195,#36196,#36197,#36198,
#36199,#36200,#36201,#36202,#36203,#36204,#36205,#36206,#36207,#36208,#36209,
#36210,#36211,#36212,#36213,#36214,#36215,#36216,#36217,#36218,#36219,#36220,
#36221,#36222,#36223,#36224,#36225,#36226,#36227,#36228,#36229,#36230,#36231,
#36232,#36233,#36234,#36235,#36236,#36237,#36238,#36239,#36240,#36241,#36242,
#36243,#36244,#36245,#36246,#36247,#36248,#36249,#36250,#36251,#36252,#36253,
#36254,#36255,#36256,#36257,#36258,#36259,#36260,#36261,#36262,#36263,#36264,
#36265,#36266,#36267,#36268,#36269,#36270,#36271,#36272,#36273,#36274,#36275,
#36276,#36277,#36278,#36279,#36280,#36281),(#36282,#36283,#36284,#36285,
#36286,#36287,#36288,#36289,#36290,#36291,#36292,#36293,#36294,#36295,#36296,
#36297,#36298,#36299,#36300,#36301,#36302,#36303,#36304,#36305,#36306,#36307,
#36308,#36309,#36310,#36311,#36312,#36313,#36314,#36315,#36316,#36317,#36318,
#36319,#36320,#36321,#36322,#36323,#36324,#36325,#36326,#36327,#36328,#36329,
#36330,#36331,#36332,#36333,#36334,#36335,#36336,#36337,#36338,#36339,#36340,
#36341,#36342,#36343,#36344,#36345,#36346,#36347,#36348,#36349,#36350,#36351,
#36352,#36353,#36354,#36355,#36356,#36357,#36358,#36359,#36360,#36361,#36362,
#36363,#36364,#36365,#36366,#36367,#36368,#36369,#36370,#36371,#36372,#36373,
#36374,#36375,#36376,#36377,#36378,#36379,#36380,#36381,#36382)),
 .UNSPECIFIED.,.F.,.F.,.F.,(4,1,4),(4,1,1,1,1,1,1,1,1,1,1,1,1,1,1,1,1,1,
1,1,1,1,1,1,1,1,1,1,1,1,1,1,1,1,1,1,1,1,1,1,1,1,1,1,1,1,1,1,1,1,1,1,1,1,
1,1,1,1,1,1,1,1,1,1,1,1,1,1,1,1,1,1,1,1,1,1,1,1,1,1,1,1,1,1,1,1,1,1,1,1,
1,1,1,1,1,1,1,1,4),(-1.09083078249646,-0.623331875712262,0.),(11.8012855294006,
12.2916839112399,12.7820822930791,13.2724806749184,13.7628790567577,14.253277438597,
14.7436758204363,15.2340742022756,15.7244725841148,16.2148709659541,16.7052693477934,
17.1956677296327,17.686066111472,18.1764644933113,18.6668628751505,19.1572612569898,
19.6476596388291,20.1380580206684,20.6284564025077,21.118854784347,21.6092531661862,
22.0996515480255,22.5900499298648,23.0804483117041,23.5708466935434,24.0612450753827,
24.5516434572219,25.0420418390612,25.5324402209005,26.0228386027398,26.5132369845791,
27.0036353664184,27.4940337482576,27.9844321300969,28.4748305119362,28.9652288937755,
29.4556272756148,29.9460256574541,30.4364240392933,30.9268224211326,31.4172208029719,
31.9076191848112,32.3980175666505,32.8884159484898,33.378814330329,33.8692127121683,
34.3596110940076,34.8500094758469,35.3404078576862,35.8308062395255,36.3212046213647,
36.811603003204,37.3020013850433,37.7923997668826,38.2827981487219,38.7731965305612,
39.2635949124004,39.7539932942397,40.244391676079,40.7347900579183,41.2251884397576,
41.7155868215969,42.2059852034361,42.6963835852754,43.1867819671147,43.677180348954,
44.1675787307933,44.6579771126326,45.1483754944718,45.6387738763111,46.1291722581504,
46.6195706399897,47.109969021829,47.6003674036683,48.0907657855076,48.5811641673468,
49.0715625491861,49.5619609310254,50.0523593128647,50.542757694704,51.0331560765432,
51.5235544583825,52.0139528402218,52.5043512220611,52.9947496039004,53.4851479857397,
53.975546367579,54.4659447494182,54.9563431312575,55.4467415130968,55.9371398949361,
56.4275382767754,56.9179366586147,57.4083350404539,57.8987334222932,58.3891318041325,
58.8795301859718,59.3699285678111,59.8603269496504),.UNSPECIFIED.);
#324=B_SPLINE_SURFACE_WITH_KNOTS('',3,3,((#38272,#38273,#38274,#38275,#38276,
#38277,#38278,#38279,#38280,#38281,#38282,#38283,#38284,#38285,#38286,#38287,
#38288,#38289,#38290,#38291,#38292,#38293,#38294,#38295,#38296,#38297,#38298,
#38299,#38300,#38301,#38302,#38303,#38304,#38305,#38306,#38307,#38308,#38309,
#38310,#38311,#38312,#38313,#38314,#38315,#38316,#38317,#38318,#38319,#38320,
#38321,#38322,#38323,#38324,#38325,#38326,#38327,#38328,#38329,#38330,#38331,
#38332,#38333,#38334,#38335,#38336,#38337,#38338,#38339,#38340,#38341,#38342,
#38343,#38344,#38345,#38346,#38347,#38348,#38349,#38350,#38351,#38352,#38353,
#38354,#38355,#38356,#38357,#38358,#38359,#38360,#38361,#38362,#38363,#38364,
#38365,#38366),(#38367,#38368,#38369,#38370,#38371,#38372,#38373,#38374,
#38375,#38376,#38377,#38378,#38379,#38380,#38381,#38382,#38383,#38384,#38385,
#38386,#38387,#38388,#38389,#38390,#38391,#38392,#38393,#38394,#38395,#38396,
#38397,#38398,#38399,#38400,#38401,#38402,#38403,#38404,#38405,#38406,#38407,
#38408,#38409,#38410,#38411,#38412,#38413,#38414,#38415,#38416,#38417,#38418,
#38419,#38420,#38421,#38422,#38423,#38424,#38425,#38426,#38427,#38428,#38429,
#38430,#38431,#38432,#38433,#38434,#38435,#38436,#38437,#38438,#38439,#38440,
#38441,#38442,#38443,#38444,#38445,#38446,#38447,#38448,#38449,#38450,#38451,
#38452,#38453,#38454,#38455,#38456,#38457,#38458,#38459,#38460,#38461),
(#38462,#38463,#38464,#38465,#38466,#38467,#38468,#38469,#38470,#38471,
#38472,#38473,#38474,#38475,#38476,#38477,#38478,#38479,#38480,#38481,#38482,
#38483,#38484,#38485,#38486,#38487,#38488,#38489,#38490,#38491,#38492,#38493,
#38494,#38495,#38496,#38497,#38498,#38499,#38500,#38501,#38502,#38503,#38504,
#38505,#38506,#38507,#38508,#38509,#38510,#38511,#38512,#38513,#38514,#38515,
#38516,#38517,#38518,#38519,#38520,#38521,#38522,#38523,#38524,#38525,#38526,
#38527,#38528,#38529,#38530,#38531,#38532,#38533,#38534,#38535,#38536,#38537,
#38538,#38539,#38540,#38541,#38542,#38543,#38544,#38545,#38546,#38547,#38548,
#38549,#38550,#38551,#38552,#38553,#38554,#38555,#38556),(#38557,#38558,
#38559,#38560,#38561,#38562,#38563,#38564,#38565,#38566,#38567,#38568,#38569,
#38570,#38571,#38572,#38573,#38574,#38575,#38576,#38577,#38578,#38579,#38580,
#38581,#38582,#38583,#38584,#38585,#38586,#38587,#38588,#38589,#38590,#38591,
#38592,#38593,#38594,#38595,#38596,#38597,#38598,#38599,#38600,#38601,#38602,
#38603,#38604,#38605,#38606,#38607,#38608,#38609,#38610,#38611,#38612,#38613,
#38614,#38615,#38616,#38617,#38618,#38619,#38620,#38621,#38622,#38623,#38624,
#38625,#38626,#38627,#38628,#38629,#38630,#38631,#38632,#38633,#38634,#38635,
#38636,#38637,#38638,#38639,#38640,#38641,#38642,#38643,#38644,#38645,#38646,
#38647,#38648,#38649,#38650,#38651)),.UNSPECIFIED.,.F.,.F.,.F.,(4,4),(4,
1,1,1,1,1,1,1,1,1,1,1,1,1,1,1,1,1,1,1,1,1,1,1,1,1,1,1,1,1,1,1,1,1,1,1,1,
1,1,1,1,1,1,1,1,1,1,1,1,1,1,1,1,1,1,1,1,1,1,1,1,1,1,1,1,1,1,1,1,1,1,1,1,
1,1,1,1,1,1,1,1,1,1,1,1,1,1,1,1,1,1,1,4),(0.,0.0989001011121828),(8.30505915324877,
8.80450411269543,9.30394907214209,9.80339403158876,10.3028389910354,10.8022839504821,
11.3017289099287,11.8011738693754,12.3006188288221,12.8000637882687,13.2995087477154,
13.7989537071621,14.2983986666087,14.7978436260554,15.297288585502,15.7967335449487,
16.2961785043954,16.795623463842,17.2950684232887,17.7945133827353,18.293958342182,
18.7934033016287,19.2928482610753,19.792293220522,20.2917381799687,20.7911831394153,
21.290628098862,21.7900730583086,22.2895180177553,22.788962977202,23.2884079366486,
23.7878528960953,24.287297855542,24.7867428149886,25.2861877744353,25.7856327338819,
26.2850776933286,26.7845226527753,27.2839676122219,27.7834125716686,28.2828575311152,
28.7823024905619,29.2817474500086,29.7811924094552,30.2806373689019,30.7800823283486,
31.2795272877952,31.7789722472419,32.2784172066885,32.7778621661352,33.2773071255819,
33.7767520850285,34.2761970444752,34.7756420039219,35.2750869633685,35.7745319228152,
36.2739768822618,36.7734218417085,37.2728668011552,37.7723117606018,38.2717567200485,
38.7712016794951,39.2706466389418,39.7700915983885,40.2695365578351,40.7689815172818,
41.2684264767285,41.7678714361751,42.2673163956218,42.7667613550684,43.2662063145151,
43.7656512739618,44.2650962334084,44.7645411928551,45.2639861523018,45.7634311117484,
46.2628760711951,46.7623210306417,47.2617659900884,47.7612109495351,48.2606559089817,
48.7601008684284,49.2595458278751,49.7589907873217,50.2584357467684,50.757880706215,
51.2573256656617,51.7567706251084,52.256215584555,52.7556605440017,53.2551055034483,
53.754550462895,54.2539954223417),.UNSPECIFIED.);
#325=B_SPLINE_SURFACE_WITH_KNOTS('',3,3,((#38789,#38790,#38791,#38792,#38793,
#38794,#38795,#38796,#38797,#38798,#38799,#38800,#38801,#38802,#38803,#38804,
#38805,#38806,#38807,#38808,#38809,#38810,#38811,#38812,#38813,#38814,#38815,
#38816,#38817,#38818,#38819,#38820,#38821,#38822,#38823,#38824,#38825,#38826,
#38827,#38828,#38829,#38830,#38831,#38832,#38833,#38834,#38835,#38836,#38837,
#38838,#38839,#38840,#38841,#38842,#38843,#38844,#38845,#38846,#38847,#38848,
#38849,#38850,#38851,#38852,#38853,#38854,#38855,#38856,#38857,#38858,#38859,
#38860,#38861,#38862,#38863,#38864,#38865,#38866,#38867,#38868,#38869,#38870,
#38871,#38872,#38873,#38874,#38875,#38876,#38877,#38878,#38879,#38880,#38881,
#38882,#38883),(#38884,#38885,#38886,#38887,#38888,#38889,#38890,#38891,
#38892,#38893,#38894,#38895,#38896,#38897,#38898,#38899,#38900,#38901,#38902,
#38903,#38904,#38905,#38906,#38907,#38908,#38909,#38910,#38911,#38912,#38913,
#38914,#38915,#38916,#38917,#38918,#38919,#38920,#38921,#38922,#38923,#38924,
#38925,#38926,#38927,#38928,#38929,#38930,#38931,#38932,#38933,#38934,#38935,
#38936,#38937,#38938,#38939,#38940,#38941,#38942,#38943,#38944,#38945,#38946,
#38947,#38948,#38949,#38950,#38951,#38952,#38953,#38954,#38955,#38956,#38957,
#38958,#38959,#38960,#38961,#38962,#38963,#38964,#38965,#38966,#38967,#38968,
#38969,#38970,#38971,#38972,#38973,#38974,#38975,#38976,#38977,#38978),
(#38979,#38980,#38981,#38982,#38983,#38984,#38985,#38986,#38987,#38988,
#38989,#38990,#38991,#38992,#38993,#38994,#38995,#38996,#38997,#38998,#38999,
#39000,#39001,#39002,#39003,#39004,#39005,#39006,#39007,#39008,#39009,#39010,
#39011,#39012,#39013,#39014,#39015,#39016,#39017,#39018,#39019,#39020,#39021,
#39022,#39023,#39024,#39025,#39026,#39027,#39028,#39029,#39030,#39031,#39032,
#39033,#39034,#39035,#39036,#39037,#39038,#39039,#39040,#39041,#39042,#39043,
#39044,#39045,#39046,#39047,#39048,#39049,#39050,#39051,#39052,#39053,#39054,
#39055,#39056,#39057,#39058,#39059,#39060,#39061,#39062,#39063,#39064,#39065,
#39066,#39067,#39068,#39069,#39070,#39071,#39072,#39073),(#39074,#39075,
#39076,#39077,#39078,#39079,#39080,#39081,#39082,#39083,#39084,#39085,#39086,
#39087,#39088,#39089,#39090,#39091,#39092,#39093,#39094,#39095,#39096,#39097,
#39098,#39099,#39100,#39101,#39102,#39103,#39104,#39105,#39106,#39107,#39108,
#39109,#39110,#39111,#39112,#39113,#39114,#39115,#39116,#39117,#39118,#39119,
#39120,#39121,#39122,#39123,#39124,#39125,#39126,#39127,#39128,#39129,#39130,
#39131,#39132,#39133,#39134,#39135,#39136,#39137,#39138,#39139,#39140,#39141,
#39142,#39143,#39144,#39145,#39146,#39147,#39148,#39149,#39150,#39151,#39152,
#39153,#39154,#39155,#39156,#39157,#39158,#39159,#39160,#39161,#39162,#39163,
#39164,#39165,#39166,#39167,#39168)),.UNSPECIFIED.,.F.,.F.,.F.,(4,4),(4,
1,1,1,1,1,1,1,1,1,1,1,1,1,1,1,1,1,1,1,1,1,1,1,1,1,1,1,1,1,1,1,1,1,1,1,1,
1,1,1,1,1,1,1,1,1,1,1,1,1,1,1,1,1,1,1,1,1,1,1,1,1,1,1,1,1,1,1,1,1,1,1,1,
1,1,1,1,1,1,1,1,1,1,1,1,1,1,1,1,1,1,1,4),(0.,0.0989001011121828),(11.6147305479243,
12.1141755073709,12.6136204668176,13.1130654262643,13.6125103857109,14.1119553451576,
14.6114003046042,15.1108452640509,15.6102902234976,16.1097351829442,16.6091801423909,
17.1086251018376,17.6080700612842,18.1075150207309,18.6069599801775,19.1064049396242,
19.6058498990709,20.1052948585175,20.6047398179642,21.1041847774109,21.6036297368575,
22.1030746963042,22.6025196557508,23.1019646151975,23.6014095746442,24.1008545340908,
24.6002994935375,25.0997444529841,25.5991894124308,26.0986343718775,26.5980793313241,
27.0975242907708,27.5969692502175,28.0964142096641,28.5958591691108,29.0953041285574,
29.5947490880041,30.0941940474508,30.5936390068974,31.0930839663441,31.5925289257907,
32.0919738852374,32.5914188446841,33.0908638041307,33.5903087635774,34.0897537230241,
34.5891986824707,35.0886436419174,35.588088601364,36.0875335608107,36.5869785202574,
37.086423479704,37.5858684391507,38.0853133985973,38.584758358044,39.0842033174907,
39.5836482769373,40.083093236384,40.5825381958307,41.0819831552773,41.581428114724,
42.0808730741707,42.5803180336173,43.079762993064,43.5792079525106,44.0786529119573,
44.578097871404,45.0775428308506,45.5769877902973,46.0764327497439,46.5758777091906,
47.0753226686373,47.5747676280839,48.0742125875306,48.5736575469773,49.0731025064239,
49.5725474658706,50.0719924253172,50.5714373847639,51.0708823442106,51.5703273036572,
52.0697722631039,52.5692172225505,53.0686621819972,53.5681071414439,54.0675521008905,
54.5669970603372,55.0664420197839,55.5658869792305,56.0653319386772,56.5647768981239,
57.0642218575705,57.5636668170172),.UNSPECIFIED.);
#326=B_SPLINE_SURFACE_WITH_KNOTS('',3,3,((#39272,#39273,#39274,#39275,#39276,
#39277,#39278,#39279,#39280,#39281,#39282,#39283,#39284,#39285,#39286,#39287,
#39288,#39289,#39290,#39291,#39292,#39293,#39294,#39295,#39296,#39297,#39298,
#39299,#39300,#39301,#39302,#39303,#39304,#39305,#39306,#39307,#39308,#39309,
#39310,#39311,#39312,#39313,#39314,#39315,#39316,#39317,#39318,#39319,#39320,
#39321,#39322,#39323,#39324,#39325,#39326,#39327,#39328,#39329,#39330,#39331,
#39332,#39333,#39334),(#39335,#39336,#39337,#39338,#39339,#39340,#39341,
#39342,#39343,#39344,#39345,#39346,#39347,#39348,#39349,#39350,#39351,#39352,
#39353,#39354,#39355,#39356,#39357,#39358,#39359,#39360,#39361,#39362,#39363,
#39364,#39365,#39366,#39367,#39368,#39369,#39370,#39371,#39372,#39373,#39374,
#39375,#39376,#39377,#39378,#39379,#39380,#39381,#39382,#39383,#39384,#39385,
#39386,#39387,#39388,#39389,#39390,#39391,#39392,#39393,#39394,#39395,#39396,
#39397),(#39398,#39399,#39400,#39401,#39402,#39403,#39404,#39405,#39406,
#39407,#39408,#39409,#39410,#39411,#39412,#39413,#39414,#39415,#39416,#39417,
#39418,#39419,#39420,#39421,#39422,#39423,#39424,#39425,#39426,#39427,#39428,
#39429,#39430,#39431,#39432,#39433,#39434,#39435,#39436,#39437,#39438,#39439,
#39440,#39441,#39442,#39443,#39444,#39445,#39446,#39447,#39448,#39449,#39450,
#39451,#39452,#39453,#39454,#39455,#39456,#39457,#39458,#39459,#39460),
(#39461,#39462,#39463,#39464,#39465,#39466,#39467,#39468,#39469,#39470,
#39471,#39472,#39473,#39474,#39475,#39476,#39477,#39478,#39479,#39480,#39481,
#39482,#39483,#39484,#39485,#39486,#39487,#39488,#39489,#39490,#39491,#39492,
#39493,#39494,#39495,#39496,#39497,#39498,#39499,#39500,#39501,#39502,#39503,
#39504,#39505,#39506,#39507,#39508,#39509,#39510,#39511,#39512,#39513,#39514,
#39515,#39516,#39517,#39518,#39519,#39520,#39521,#39522,#39523),(#39524,
#39525,#39526,#39527,#39528,#39529,#39530,#39531,#39532,#39533,#39534,#39535,
#39536,#39537,#39538,#39539,#39540,#39541,#39542,#39543,#39544,#39545,#39546,
#39547,#39548,#39549,#39550,#39551,#39552,#39553,#39554,#39555,#39556,#39557,
#39558,#39559,#39560,#39561,#39562,#39563,#39564,#39565,#39566,#39567,#39568,
#39569,#39570,#39571,#39572,#39573,#39574,#39575,#39576,#39577,#39578,#39579,
#39580,#39581,#39582,#39583,#39584,#39585,#39586)),.UNSPECIFIED.,.F.,.F.,
 .F.,(4,1,4),(4,1,1,1,1,1,1,1,1,1,1,1,1,1,1,1,1,1,1,1,1,1,1,1,1,1,1,1,1,
1,1,1,1,1,1,1,1,1,1,1,1,1,1,1,1,1,1,1,1,1,1,1,1,1,1,1,1,1,1,1,4),(0.,0.467498906784196,
1.09083078249646),(6.2831853071796,6.77083463049239,7.25848395380519,7.74613327711798,
8.23378260043077,8.72143192374356,9.20908124705636,9.69673057036915,10.1843798936819,
10.6720292169947,11.1596785403075,11.6473278636203,12.1349771869331,12.6226265102459,
13.1102758335587,13.5979251568715,14.0855744801843,14.5732238034971,15.0608731268099,
15.5485224501227,16.0361717734355,16.5238210967483,17.011470420061,17.4991197433738,
17.9867690666866,18.4744183899994,18.9620677133122,19.449717036625,19.9373663599378,
20.4250156832506,20.9126650065634,21.4003143298762,21.887963653189,22.3756129765018,
22.8632622998146,23.3509116231274,23.8385609464401,24.3262102697529,24.8138595930657,
25.3015089163785,25.7891582396913,26.2768075630041,26.7644568863169,27.2521062096297,
27.7397555329425,28.2274048562553,28.7150541795681,29.2027035028809,29.6903528261937,
30.1780021495065,30.6656514728192,31.153300796132,31.6409501194448,32.1285994427576,
32.6162487660704,33.1038980893832,33.591547412696,34.0791967360088,34.5668460593216,
35.0544953826344,35.5421447059472),.UNSPECIFIED.);
#327=B_SPLINE_SURFACE_WITH_KNOTS('',3,3,((#39847,#39848,#39849,#39850,#39851,
#39852,#39853,#39854,#39855,#39856,#39857,#39858,#39859,#39860,#39861,#39862,
#39863,#39864,#39865,#39866,#39867,#39868,#39869,#39870,#39871,#39872,#39873,
#39874,#39875,#39876,#39877,#39878,#39879,#39880,#39881,#39882,#39883,#39884,
#39885,#39886,#39887,#39888,#39889,#39890,#39891,#39892,#39893,#39894,#39895,
#39896,#39897,#39898,#39899,#39900,#39901,#39902,#39903,#39904,#39905,#39906,
#39907,#39908,#39909),(#39910,#39911,#39912,#39913,#39914,#39915,#39916,
#39917,#39918,#39919,#39920,#39921,#39922,#39923,#39924,#39925,#39926,#39927,
#39928,#39929,#39930,#39931,#39932,#39933,#39934,#39935,#39936,#39937,#39938,
#39939,#39940,#39941,#39942,#39943,#39944,#39945,#39946,#39947,#39948,#39949,
#39950,#39951,#39952,#39953,#39954,#39955,#39956,#39957,#39958,#39959,#39960,
#39961,#39962,#39963,#39964,#39965,#39966,#39967,#39968,#39969,#39970,#39971,
#39972),(#39973,#39974,#39975,#39976,#39977,#39978,#39979,#39980,#39981,
#39982,#39983,#39984,#39985,#39986,#39987,#39988,#39989,#39990,#39991,#39992,
#39993,#39994,#39995,#39996,#39997,#39998,#39999,#40000,#40001,#40002,#40003,
#40004,#40005,#40006,#40007,#40008,#40009,#40010,#40011,#40012,#40013,#40014,
#40015,#40016,#40017,#40018,#40019,#40020,#40021,#40022,#40023,#40024,#40025,
#40026,#40027,#40028,#40029,#40030,#40031,#40032,#40033,#40034,#40035),
(#40036,#40037,#40038,#40039,#40040,#40041,#40042,#40043,#40044,#40045,
#40046,#40047,#40048,#40049,#40050,#40051,#40052,#40053,#40054,#40055,#40056,
#40057,#40058,#40059,#40060,#40061,#40062,#40063,#40064,#40065,#40066,#40067,
#40068,#40069,#40070,#40071,#40072,#40073,#40074,#40075,#40076,#40077,#40078,
#40079,#40080,#40081,#40082,#40083,#40084,#40085,#40086,#40087,#40088,#40089,
#40090,#40091,#40092,#40093,#40094,#40095,#40096,#40097,#40098)),
 .UNSPECIFIED.,.F.,.F.,.F.,(4,4),(4,1,1,1,1,1,1,1,1,1,1,1,1,1,1,1,1,1,1,
1,1,1,1,1,1,1,1,1,1,1,1,1,1,1,1,1,1,1,1,1,1,1,1,1,1,1,1,1,1,1,1,1,1,1,1,
1,1,1,1,1,4),(0.,0.0671853436149874),(7.04827039213817,7.54746954913154,
8.0466687061249,8.54586786311827,9.04506702011163,9.54426617710499,10.0434653340984,
10.5426644910917,11.0418636480851,11.5410628050784,12.0402619620718,12.5394611190652,
13.0386602760585,13.5378594330519,14.0370585900453,14.5362577470386,15.035456904032,
15.5346560610254,16.0338552180187,16.5330543750121,17.0322535320054,17.5314526889988,
18.0306518459922,18.5298510029855,19.0290501599789,19.5282493169723,20.0274484739656,
20.526647630959,21.0258467879524,21.5250459449457,22.0242451019391,22.5234442589325,
23.0226434159258,23.5218425729192,24.0210417299125,24.5202408869059,25.0194400438993,
25.5186392008926,26.017838357886,26.5170375148794,27.0162366718727,27.5154358288661,
28.0146349858595,28.5138341428528,29.0130332998462,29.5122324568395,30.0114316138329,
30.5106307708263,31.0098299278196,31.509029084813,32.0082282418064,32.5074273987997,
33.0066265557931,33.5058257127865,34.0050248697798,34.5042240267732,35.0034231837665,
35.5026223407599,36.0018214977533,36.5010206547466,37.00021981174),
 .UNSPECIFIED.);
#328=B_SPLINE_SURFACE_WITH_KNOTS('',3,3,((#40257,#40258,#40259,#40260,#40261,
#40262,#40263,#40264,#40265,#40266,#40267,#40268,#40269,#40270,#40271,#40272,
#40273,#40274,#40275,#40276,#40277,#40278,#40279,#40280,#40281,#40282,#40283,
#40284,#40285,#40286,#40287,#40288,#40289,#40290,#40291,#40292,#40293,#40294,
#40295,#40296,#40297,#40298,#40299,#40300,#40301,#40302,#40303,#40304,#40305,
#40306,#40307,#40308,#40309,#40310,#40311,#40312,#40313,#40314,#40315,#40316,
#40317,#40318,#40319),(#40320,#40321,#40322,#40323,#40324,#40325,#40326,
#40327,#40328,#40329,#40330,#40331,#40332,#40333,#40334,#40335,#40336,#40337,
#40338,#40339,#40340,#40341,#40342,#40343,#40344,#40345,#40346,#40347,#40348,
#40349,#40350,#40351,#40352,#40353,#40354,#40355,#40356,#40357,#40358,#40359,
#40360,#40361,#40362,#40363,#40364,#40365,#40366,#40367,#40368,#40369,#40370,
#40371,#40372,#40373,#40374,#40375,#40376,#40377,#40378,#40379,#40380,#40381,
#40382),(#40383,#40384,#40385,#40386,#40387,#40388,#40389,#40390,#40391,
#40392,#40393,#40394,#40395,#40396,#40397,#40398,#40399,#40400,#40401,#40402,
#40403,#40404,#40405,#40406,#40407,#40408,#40409,#40410,#40411,#40412,#40413,
#40414,#40415,#40416,#40417,#40418,#40419,#40420,#40421,#40422,#40423,#40424,
#40425,#40426,#40427,#40428,#40429,#40430,#40431,#40432,#40433,#40434,#40435,
#40436,#40437,#40438,#40439,#40440,#40441,#40442,#40443,#40444,#40445),
(#40446,#40447,#40448,#40449,#40450,#40451,#40452,#40453,#40454,#40455,
#40456,#40457,#40458,#40459,#40460,#40461,#40462,#40463,#40464,#40465,#40466,
#40467,#40468,#40469,#40470,#40471,#40472,#40473,#40474,#40475,#40476,#40477,
#40478,#40479,#40480,#40481,#40482,#40483,#40484,#40485,#40486,#40487,#40488,
#40489,#40490,#40491,#40492,#40493,#40494,#40495,#40496,#40497,#40498,#40499,
#40500,#40501,#40502,#40503,#40504,#40505,#40506,#40507,#40508),(#40509,
#40510,#40511,#40512,#40513,#40514,#40515,#40516,#40517,#40518,#40519,#40520,
#40521,#40522,#40523,#40524,#40525,#40526,#40527,#40528,#40529,#40530,#40531,
#40532,#40533,#40534,#40535,#40536,#40537,#40538,#40539,#40540,#40541,#40542,
#40543,#40544,#40545,#40546,#40547,#40548,#40549,#40550,#40551,#40552,#40553,
#40554,#40555,#40556,#40557,#40558,#40559,#40560,#40561,#40562,#40563,#40564,
#40565,#40566,#40567,#40568,#40569,#40570,#40571)),.UNSPECIFIED.,.F.,.F.,
 .F.,(4,1,4),(4,1,1,1,1,1,1,1,1,1,1,1,1,1,1,1,1,1,1,1,1,1,1,1,1,1,1,1,1,
1,1,1,1,1,1,1,1,1,1,1,1,1,1,1,1,1,1,1,1,1,1,1,1,1,1,1,1,1,1,1,4),(0.,0.467498906784196,
1.09083078249646),(8.50634549793098,8.99399482124377,9.48164414455657,9.96929346786936,
10.4569427911822,10.9445921144949,11.4322414378077,11.9198907611205,12.4075400844333,
12.8951894077461,13.3828387310589,13.8704880543717,14.3581373776845,14.8457867009973,
15.3334360243101,15.8210853476229,16.3087346709357,16.7963839942485,17.2840333175613,
17.771682640874,18.2593319641868,18.7469812874996,19.2346306108124,19.7222799341252,
20.209929257438,20.6975785807508,21.1852279040636,21.6728772273764,22.1605265506892,
22.648175874002,23.1358251973148,23.6234745206276,24.1111238439404,24.5987731672532,
25.0864224905659,25.5740718138787,26.0617211371915,26.5493704605043,27.0370197838171,
27.5246691071299,28.0123184304427,28.4999677537555,28.9876170770683,29.4752664003811,
29.9629157236939,30.4505650470067,30.9382143703195,31.4258636936323,31.913513016945,
32.4011623402578,32.8888116635706,33.3764609868834,33.8641103101962,34.351759633509,
34.8394089568218,35.3270582801346,35.8147076034474,36.3023569267602,36.790006250073,
37.2776555733858,37.7653048966986),.UNSPECIFIED.);
#329=B_SPLINE_SURFACE_WITH_KNOTS('',3,3,((#40664,#40665,#40666,#40667,#40668,
#40669,#40670,#40671,#40672,#40673,#40674,#40675,#40676,#40677,#40678,#40679,
#40680,#40681,#40682,#40683,#40684,#40685,#40686,#40687,#40688,#40689,#40690,
#40691,#40692,#40693,#40694,#40695,#40696,#40697,#40698,#40699,#40700,#40701,
#40702,#40703,#40704,#40705,#40706,#40707,#40708,#40709,#40710,#40711,#40712,
#40713,#40714,#40715,#40716,#40717,#40718,#40719,#40720,#40721,#40722,#40723,
#40724,#40725,#40726),(#40727,#40728,#40729,#40730,#40731,#40732,#40733,
#40734,#40735,#40736,#40737,#40738,#40739,#40740,#40741,#40742,#40743,#40744,
#40745,#40746,#40747,#40748,#40749,#40750,#40751,#40752,#40753,#40754,#40755,
#40756,#40757,#40758,#40759,#40760,#40761,#40762,#40763,#40764,#40765,#40766,
#40767,#40768,#40769,#40770,#40771,#40772,#40773,#40774,#40775,#40776,#40777,
#40778,#40779,#40780,#40781,#40782,#40783,#40784,#40785,#40786,#40787,#40788,
#40789),(#40790,#40791,#40792,#40793,#40794,#40795,#40796,#40797,#40798,
#40799,#40800,#40801,#40802,#40803,#40804,#40805,#40806,#40807,#40808,#40809,
#40810,#40811,#40812,#40813,#40814,#40815,#40816,#40817,#40818,#40819,#40820,
#40821,#40822,#40823,#40824,#40825,#40826,#40827,#40828,#40829,#40830,#40831,
#40832,#40833,#40834,#40835,#40836,#40837,#40838,#40839,#40840,#40841,#40842,
#40843,#40844,#40845,#40846,#40847,#40848,#40849,#40850,#40851,#40852),
(#40853,#40854,#40855,#40856,#40857,#40858,#40859,#40860,#40861,#40862,
#40863,#40864,#40865,#40866,#40867,#40868,#40869,#40870,#40871,#40872,#40873,
#40874,#40875,#40876,#40877,#40878,#40879,#40880,#40881,#40882,#40883,#40884,
#40885,#40886,#40887,#40888,#40889,#40890,#40891,#40892,#40893,#40894,#40895,
#40896,#40897,#40898,#40899,#40900,#40901,#40902,#40903,#40904,#40905,#40906,
#40907,#40908,#40909,#40910,#40911,#40912,#40913,#40914,#40915),(#40916,
#40917,#40918,#40919,#40920,#40921,#40922,#40923,#40924,#40925,#40926,#40927,
#40928,#40929,#40930,#40931,#40932,#40933,#40934,#40935,#40936,#40937,#40938,
#40939,#40940,#40941,#40942,#40943,#40944,#40945,#40946,#40947,#40948,#40949,
#40950,#40951,#40952,#40953,#40954,#40955,#40956,#40957,#40958,#40959,#40960,
#40961,#40962,#40963,#40964,#40965,#40966,#40967,#40968,#40969,#40970,#40971,
#40972,#40973,#40974,#40975,#40976,#40977,#40978)),.UNSPECIFIED.,.F.,.F.,
 .F.,(4,1,4),(4,1,1,1,1,1,1,1,1,1,1,1,1,1,1,1,1,1,1,1,1,1,1,1,1,1,1,1,1,
1,1,1,1,1,1,1,1,1,1,1,1,1,1,1,1,1,1,1,1,1,1,1,1,1,1,1,1,1,1,1,4),(-1.09083078249646,
-0.623331875712262,0.),(9.57812533864923,10.065774661962,10.5534239852748,
11.0410733085876,11.5287226319004,12.0163719552132,12.504021278526,12.9916706018388,
13.4793199251516,13.9669692484644,14.4546185717772,14.94226789509,15.4299172184027,
15.9175665417155,16.4052158650283,16.8928651883411,17.3805145116539,17.8681638349667,
18.3558131582795,18.8434624815923,19.3311118049051,19.8187611282179,20.3064104515307,
20.7940597748435,21.2817090981563,21.7693584214691,22.2570077447818,22.7446570680946,
23.2323063914074,23.7199557147202,24.207605038033,24.6952543613458,25.1829036846586,
25.6705530079714,26.1582023312842,26.645851654597,27.1335009779098,27.6211503012226,
28.1087996245354,28.5964489478482,29.0840982711609,29.5717475944737,30.0593969177865,
30.5470462410993,31.0346955644121,31.5223448877249,32.0099942110377,32.4976435343505,
32.9852928576633,33.4729421809761,33.9605915042889,34.4482408276017,34.9358901509145,
35.4235394742273,35.91118879754,36.3988381208528,36.8864874441656,37.3741367674784,
37.8617860907912,38.349435414104,38.8370847374168),.UNSPECIFIED.);
#330=B_SPLINE_SURFACE_WITH_KNOTS('',3,3,((#41048,#41049,#41050,#41051,#41052,
#41053,#41054,#41055,#41056,#41057,#41058,#41059,#41060,#41061,#41062,#41063,
#41064,#41065,#41066,#41067,#41068,#41069,#41070,#41071,#41072,#41073,#41074,
#41075,#41076,#41077,#41078,#41079,#41080,#41081,#41082,#41083,#41084,#41085,
#41086,#41087,#41088,#41089,#41090,#41091,#41092,#41093,#41094,#41095,#41096,
#41097,#41098,#41099,#41100,#41101,#41102,#41103,#41104,#41105,#41106,#41107,
#41108,#41109,#41110),(#41111,#41112,#41113,#41114,#41115,#41116,#41117,
#41118,#41119,#41120,#41121,#41122,#41123,#41124,#41125,#41126,#41127,#41128,
#41129,#41130,#41131,#41132,#41133,#41134,#41135,#41136,#41137,#41138,#41139,
#41140,#41141,#41142,#41143,#41144,#41145,#41146,#41147,#41148,#41149,#41150,
#41151,#41152,#41153,#41154,#41155,#41156,#41157,#41158,#41159,#41160,#41161,
#41162,#41163,#41164,#41165,#41166,#41167,#41168,#41169,#41170,#41171,#41172,
#41173),(#41174,#41175,#41176,#41177,#41178,#41179,#41180,#41181,#41182,
#41183,#41184,#41185,#41186,#41187,#41188,#41189,#41190,#41191,#41192,#41193,
#41194,#41195,#41196,#41197,#41198,#41199,#41200,#41201,#41202,#41203,#41204,
#41205,#41206,#41207,#41208,#41209,#41210,#41211,#41212,#41213,#41214,#41215,
#41216,#41217,#41218,#41219,#41220,#41221,#41222,#41223,#41224,#41225,#41226,
#41227,#41228,#41229,#41230,#41231,#41232,#41233,#41234,#41235,#41236),
(#41237,#41238,#41239,#41240,#41241,#41242,#41243,#41244,#41245,#41246,
#41247,#41248,#41249,#41250,#41251,#41252,#41253,#41254,#41255,#41256,#41257,
#41258,#41259,#41260,#41261,#41262,#41263,#41264,#41265,#41266,#41267,#41268,
#41269,#41270,#41271,#41272,#41273,#41274,#41275,#41276,#41277,#41278,#41279,
#41280,#41281,#41282,#41283,#41284,#41285,#41286,#41287,#41288,#41289,#41290,
#41291,#41292,#41293,#41294,#41295,#41296,#41297,#41298,#41299)),
 .UNSPECIFIED.,.F.,.F.,.F.,(4,4),(4,1,1,1,1,1,1,1,1,1,1,1,1,1,1,1,1,1,1,
1,1,1,1,1,1,1,1,1,1,1,1,1,1,1,1,1,1,1,1,1,1,1,1,1,1,1,1,1,1,1,1,1,1,1,1,
1,1,1,1,1,4),(0.,0.0671853436149874),(10.3432104236078,10.8424095806012,
11.3416087375945,11.8408078945879,12.3400070515813,12.8392062085746,13.338405365568,
13.8376045225613,14.3368036795547,14.8360028365481,15.3352019935414,15.8344011505348,
16.3336003075282,16.8327994645215,17.3319986215149,17.8311977785083,18.3303969355016,
18.829596092495,19.3287952494883,19.8279944064817,20.3271935634751,20.8263927204684,
21.3255918774618,21.8247910344552,22.3239901914485,22.8231893484419,23.3223885054353,
23.8215876624286,24.320786819422,24.8199859764153,25.3191851334087,25.8183842904021,
26.3175834473954,26.8167826043888,27.3159817613822,27.8151809183755,28.3143800753689,
28.8135792323623,29.3127783893556,29.811977546349,30.3111767033423,30.8103758603357,
31.3095750173291,31.8087741743224,32.3079733313158,32.8071724883092,33.3063716453025,
33.8055708022959,34.3047699592893,34.8039691162826,35.303168273276,35.8023674302693,
36.3015665872627,36.8007657442561,37.2999649012494,37.7991640582428,38.2983632152362,
38.7975623722295,39.2967615292229,39.7959606862163,40.2951598432096),
 .UNSPECIFIED.);
#331=B_SPLINE_SURFACE_WITH_KNOTS('',3,3,((#41411,#41412,#41413,#41414,#41415,
#41416,#41417,#41418,#41419,#41420,#41421,#41422,#41423,#41424,#41425,#41426,
#41427,#41428,#41429,#41430,#41431,#41432,#41433,#41434,#41435,#41436,#41437,
#41438,#41439,#41440,#41441,#41442,#41443,#41444,#41445,#41446,#41447,#41448,
#41449,#41450,#41451,#41452,#41453,#41454,#41455,#41456,#41457,#41458,#41459,
#41460,#41461,#41462,#41463,#41464,#41465,#41466,#41467,#41468,#41469,#41470,
#41471,#41472,#41473),(#41474,#41475,#41476,#41477,#41478,#41479,#41480,
#41481,#41482,#41483,#41484,#41485,#41486,#41487,#41488,#41489,#41490,#41491,
#41492,#41493,#41494,#41495,#41496,#41497,#41498,#41499,#41500,#41501,#41502,
#41503,#41504,#41505,#41506,#41507,#41508,#41509,#41510,#41511,#41512,#41513,
#41514,#41515,#41516,#41517,#41518,#41519,#41520,#41521,#41522,#41523,#41524,
#41525,#41526,#41527,#41528,#41529,#41530,#41531,#41532,#41533,#41534,#41535,
#41536),(#41537,#41538,#41539,#41540,#41541,#41542,#41543,#41544,#41545,
#41546,#41547,#41548,#41549,#41550,#41551,#41552,#41553,#41554,#41555,#41556,
#41557,#41558,#41559,#41560,#41561,#41562,#41563,#41564,#41565,#41566,#41567,
#41568,#41569,#41570,#41571,#41572,#41573,#41574,#41575,#41576,#41577,#41578,
#41579,#41580,#41581,#41582,#41583,#41584,#41585,#41586,#41587,#41588,#41589,
#41590,#41591,#41592,#41593,#41594,#41595,#41596,#41597,#41598,#41599),
(#41600,#41601,#41602,#41603,#41604,#41605,#41606,#41607,#41608,#41609,
#41610,#41611,#41612,#41613,#41614,#41615,#41616,#41617,#41618,#41619,#41620,
#41621,#41622,#41623,#41624,#41625,#41626,#41627,#41628,#41629,#41630,#41631,
#41632,#41633,#41634,#41635,#41636,#41637,#41638,#41639,#41640,#41641,#41642,
#41643,#41644,#41645,#41646,#41647,#41648,#41649,#41650,#41651,#41652,#41653,
#41654,#41655,#41656,#41657,#41658,#41659,#41660,#41661,#41662),(#41663,
#41664,#41665,#41666,#41667,#41668,#41669,#41670,#41671,#41672,#41673,#41674,
#41675,#41676,#41677,#41678,#41679,#41680,#41681,#41682,#41683,#41684,#41685,
#41686,#41687,#41688,#41689,#41690,#41691,#41692,#41693,#41694,#41695,#41696,
#41697,#41698,#41699,#41700,#41701,#41702,#41703,#41704,#41705,#41706,#41707,
#41708,#41709,#41710,#41711,#41712,#41713,#41714,#41715,#41716,#41717,#41718,
#41719,#41720,#41721,#41722,#41723,#41724,#41725)),.UNSPECIFIED.,.F.,.F.,
 .F.,(4,1,4),(4,1,1,1,1,1,1,1,1,1,1,1,1,1,1,1,1,1,1,1,1,1,1,1,1,1,1,1,1,
1,1,1,1,1,1,1,1,1,1,1,1,1,1,1,1,1,1,1,1,1,1,1,1,1,1,1,1,1,1,1,4),(-1.09083078249646,
-0.623331875712262,0.),(11.8012855294006,12.2889348527134,12.7765841760262,
13.264233499339,13.7518828226518,14.2395321459646,14.7271814692774,15.2148307925902,
15.702480115903,16.1901294392157,16.6777787625285,17.1654280858413,17.6530774091541,
18.1407267324669,18.6283760557797,19.1160253790925,19.6036747024053,20.0913240257181,
20.5789733490309,21.0666226723437,21.5542719956565,22.0419213189693,22.5295706422821,
23.0172199655949,23.5048692889076,23.9925186122204,24.4801679355332,24.967817258846,
25.4554665821588,25.9431159054716,26.4307652287844,26.9184145520972,27.40606387541,
27.8937131987228,28.3813625220356,28.8690118453484,29.3566611686612,29.844310491974,
30.3319598152868,30.8196091385995,31.3072584619123,31.7949077852251,32.2825571085379,
32.7702064318507,33.2578557551635,33.7455050784763,34.2331544017891,34.7208037251019,
35.2084530484147,35.6961023717275,36.1837516950403,36.6714010183531,37.1590503416659,
37.6466996649787,38.1343489882914,38.6219983116042,39.109647634917,39.5972969582298,
40.0849462815426,40.5725956048554,41.0602449281682),.UNSPECIFIED.);
#332=B_SPLINE_SURFACE_WITH_KNOTS('',2,1,((#43216,#43217),(#43218,#43219),
(#43220,#43221)),.UNSPECIFIED.,.F.,.F.,.F.,(3,3),(2,2),(0.,1.),(0.,0.0300000000000002),
 .UNSPECIFIED.);
#333=B_SPLINE_SURFACE_WITH_KNOTS('',2,1,((#43234,#43235),(#43236,#43237),
(#43238,#43239)),.UNSPECIFIED.,.F.,.F.,.F.,(3,3),(2,2),(0.,1.),(0.,0.0300000000000002),
 .UNSPECIFIED.);
#334=B_SPLINE_SURFACE_WITH_KNOTS('',2,1,((#43249,#43250),(#43251,#43252),
(#43253,#43254)),.UNSPECIFIED.,.F.,.F.,.F.,(3,3),(2,2),(0.,1.),(0.,0.0300000000000002),
 .UNSPECIFIED.);
#335=B_SPLINE_SURFACE_WITH_KNOTS('',2,1,((#43264,#43265),(#43266,#43267),
(#43268,#43269)),.UNSPECIFIED.,.F.,.F.,.F.,(3,3),(2,2),(0.,1.),(0.,0.0300000000000002),
 .UNSPECIFIED.);
#336=B_SPLINE_SURFACE_WITH_KNOTS('',2,1,((#43279,#43280),(#43281,#43282),
(#43283,#43284)),.UNSPECIFIED.,.F.,.F.,.F.,(3,3),(2,2),(0.,1.),(0.,0.0300000000000002),
 .UNSPECIFIED.);
#337=B_SPLINE_SURFACE_WITH_KNOTS('',2,1,((#43294,#43295),(#43296,#43297),
(#43298,#43299)),.UNSPECIFIED.,.F.,.F.,.F.,(3,3),(2,2),(0.,1.),(0.,0.0300000000000002),
 .UNSPECIFIED.);
#338=B_SPLINE_SURFACE_WITH_KNOTS('',2,1,((#43309,#43310),(#43311,#43312),
(#43313,#43314)),.UNSPECIFIED.,.F.,.F.,.F.,(3,3),(2,2),(0.,1.),(0.,0.0300000000000002),
 .UNSPECIFIED.);
#339=B_SPLINE_SURFACE_WITH_KNOTS('',2,1,((#43324,#43325),(#43326,#43327),
(#43328,#43329)),.UNSPECIFIED.,.F.,.F.,.F.,(3,3),(2,2),(0.,1.),(0.,0.0300000000000002),
 .UNSPECIFIED.);
#340=B_SPLINE_SURFACE_WITH_KNOTS('',2,1,((#43339,#43340),(#43341,#43342),
(#43343,#43344)),.UNSPECIFIED.,.F.,.F.,.F.,(3,3),(2,2),(0.,1.),(0.,0.0300000000000002),
 .UNSPECIFIED.);
#341=B_SPLINE_SURFACE_WITH_KNOTS('',2,1,((#43357,#43358),(#43359,#43360),
(#43361,#43362)),.UNSPECIFIED.,.F.,.F.,.F.,(3,3),(2,2),(0.,1.),(0.,0.0300000000000002),
 .UNSPECIFIED.);
#342=B_SPLINE_SURFACE_WITH_KNOTS('',2,1,((#43375,#43376),(#43377,#43378),
(#43379,#43380)),.UNSPECIFIED.,.F.,.F.,.F.,(3,3),(2,2),(0.,1.),(0.,0.0300000000000002),
 .UNSPECIFIED.);
#343=B_SPLINE_SURFACE_WITH_KNOTS('',2,1,((#43396,#43397),(#43398,#43399),
(#43400,#43401)),.UNSPECIFIED.,.F.,.F.,.F.,(3,3),(2,2),(0.,1.),(0.,0.0300000000000002),
 .UNSPECIFIED.);
#344=B_SPLINE_SURFACE_WITH_KNOTS('',2,1,((#43411,#43412),(#43413,#43414),
(#43415,#43416)),.UNSPECIFIED.,.F.,.F.,.F.,(3,3),(2,2),(0.,1.),(0.,0.0300000000000002),
 .UNSPECIFIED.);
#345=B_SPLINE_SURFACE_WITH_KNOTS('',2,1,((#43426,#43427),(#43428,#43429),
(#43430,#43431)),.UNSPECIFIED.,.F.,.F.,.F.,(3,3),(2,2),(0.,1.),(0.,0.0300000000000002),
 .UNSPECIFIED.);
#346=B_SPLINE_SURFACE_WITH_KNOTS('',2,1,((#43441,#43442),(#43443,#43444),
(#43445,#43446)),.UNSPECIFIED.,.F.,.F.,.F.,(3,3),(2,2),(0.,1.),(0.,0.0300000000000002),
 .UNSPECIFIED.);
#347=B_SPLINE_SURFACE_WITH_KNOTS('',2,1,((#43456,#43457),(#43458,#43459),
(#43460,#43461)),.UNSPECIFIED.,.F.,.F.,.F.,(3,3),(2,2),(0.,1.),(0.,0.0300000000000002),
 .UNSPECIFIED.);
#348=B_SPLINE_SURFACE_WITH_KNOTS('',2,1,((#43471,#43472),(#43473,#43474),
(#43475,#43476)),.UNSPECIFIED.,.F.,.F.,.F.,(3,3),(2,2),(0.,1.),(0.,0.0300000000000002),
 .UNSPECIFIED.);
#349=B_SPLINE_SURFACE_WITH_KNOTS('',2,1,((#43486,#43487),(#43488,#43489),
(#43490,#43491)),.UNSPECIFIED.,.F.,.F.,.F.,(3,3),(2,2),(0.,1.),(0.,0.0300000000000002),
 .UNSPECIFIED.);
#350=B_SPLINE_SURFACE_WITH_KNOTS('',2,1,((#43507,#43508),(#43509,#43510),
(#43511,#43512)),.UNSPECIFIED.,.F.,.F.,.F.,(3,3),(2,2),(0.,1.),(0.,0.0300000000000002),
 .UNSPECIFIED.);
#351=B_SPLINE_SURFACE_WITH_KNOTS('',2,1,((#43522,#43523),(#43524,#43525),
(#43526,#43527)),.UNSPECIFIED.,.F.,.F.,.F.,(3,3),(2,2),(0.,1.),(0.,0.0300000000000002),
 .UNSPECIFIED.);
#352=B_SPLINE_SURFACE_WITH_KNOTS('',2,1,((#43537,#43538),(#43539,#43540),
(#43541,#43542)),.UNSPECIFIED.,.F.,.F.,.F.,(3,3),(2,2),(0.,1.),(0.,0.0300000000000002),
 .UNSPECIFIED.);
#353=B_SPLINE_SURFACE_WITH_KNOTS('',2,1,((#43552,#43553),(#43554,#43555),
(#43556,#43557)),.UNSPECIFIED.,.F.,.F.,.F.,(3,3),(2,2),(0.,1.),(0.,0.0300000000000002),
 .UNSPECIFIED.);
#354=B_SPLINE_SURFACE_WITH_KNOTS('',2,1,((#43567,#43568),(#43569,#43570),
(#43571,#43572)),.UNSPECIFIED.,.F.,.F.,.F.,(3,3),(2,2),(0.,1.),(0.,0.0300000000000002),
 .UNSPECIFIED.);
#355=B_SPLINE_SURFACE_WITH_KNOTS('',2,1,((#43582,#43583),(#43584,#43585),
(#43586,#43587)),.UNSPECIFIED.,.F.,.F.,.F.,(3,3),(2,2),(0.,1.),(0.,0.0300000000000002),
 .UNSPECIFIED.);
#356=B_SPLINE_SURFACE_WITH_KNOTS('',2,1,((#43597,#43598),(#43599,#43600),
(#43601,#43602)),.UNSPECIFIED.,.F.,.F.,.F.,(3,3),(2,2),(0.,1.),(0.,0.0300000000000002),
 .UNSPECIFIED.);
#357=B_SPLINE_SURFACE_WITH_KNOTS('',2,1,((#43612,#43613),(#43614,#43615),
(#43616,#43617)),.UNSPECIFIED.,.F.,.F.,.F.,(3,3),(2,2),(0.,1.),(0.,0.0300000000000002),
 .UNSPECIFIED.);
#358=B_SPLINE_SURFACE_WITH_KNOTS('',2,1,((#43627,#43628),(#43629,#43630),
(#43631,#43632)),.UNSPECIFIED.,.F.,.F.,.F.,(3,3),(2,2),(0.,1.),(0.,0.0300000000000002),
 .UNSPECIFIED.);
#359=B_SPLINE_SURFACE_WITH_KNOTS('',2,1,((#43642,#43643),(#43644,#43645),
(#43646,#43647)),.UNSPECIFIED.,.F.,.F.,.F.,(3,3),(2,2),(0.,1.),(0.,0.0300000000000002),
 .UNSPECIFIED.);
#360=B_SPLINE_SURFACE_WITH_KNOTS('',2,1,((#43657,#43658),(#43659,#43660),
(#43661,#43662)),.UNSPECIFIED.,.F.,.F.,.F.,(3,3),(2,2),(0.,1.),(0.,0.0300000000000002),
 .UNSPECIFIED.);
#361=B_SPLINE_SURFACE_WITH_KNOTS('',2,1,((#43672,#43673),(#43674,#43675),
(#43676,#43677)),.UNSPECIFIED.,.F.,.F.,.F.,(3,3),(2,2),(0.,1.),(0.,0.0300000000000002),
 .UNSPECIFIED.);
#362=B_SPLINE_SURFACE_WITH_KNOTS('',2,1,((#43687,#43688),(#43689,#43690),
(#43691,#43692)),.UNSPECIFIED.,.F.,.F.,.F.,(3,3),(2,2),(0.,1.),(0.,0.0300000000000002),
 .UNSPECIFIED.);
#363=B_SPLINE_SURFACE_WITH_KNOTS('',2,1,((#43702,#43703),(#43704,#43705),
(#43706,#43707)),.UNSPECIFIED.,.F.,.F.,.F.,(3,3),(2,2),(0.,1.),(0.,0.0300000000000002),
 .UNSPECIFIED.);
#364=B_SPLINE_SURFACE_WITH_KNOTS('',2,1,((#43717,#43718),(#43719,#43720),
(#43721,#43722)),.UNSPECIFIED.,.F.,.F.,.F.,(3,3),(2,2),(0.,1.),(0.,0.0300000000000002),
 .UNSPECIFIED.);
#365=B_SPLINE_SURFACE_WITH_KNOTS('',2,1,((#43736,#43737),(#43738,#43739),
(#43740,#43741)),.UNSPECIFIED.,.F.,.F.,.F.,(3,3),(2,2),(0.,1.),(0.,0.0300000000000002),
 .UNSPECIFIED.);
#366=B_SPLINE_SURFACE_WITH_KNOTS('',2,1,((#43754,#43755),(#43756,#43757),
(#43758,#43759)),.UNSPECIFIED.,.F.,.F.,.F.,(3,3),(2,2),(0.,1.),(0.,0.0300000000000002),
 .UNSPECIFIED.);
#367=B_SPLINE_SURFACE_WITH_KNOTS('',2,1,((#43769,#43770),(#43771,#43772),
(#43773,#43774)),.UNSPECIFIED.,.F.,.F.,.F.,(3,3),(2,2),(0.,1.),(0.,0.0300000000000002),
 .UNSPECIFIED.);
#368=B_SPLINE_SURFACE_WITH_KNOTS('',2,1,((#43784,#43785),(#43786,#43787),
(#43788,#43789)),.UNSPECIFIED.,.F.,.F.,.F.,(3,3),(2,2),(0.,1.),(0.,0.0300000000000002),
 .UNSPECIFIED.);
#369=B_SPLINE_SURFACE_WITH_KNOTS('',2,1,((#43799,#43800),(#43801,#43802),
(#43803,#43804)),.UNSPECIFIED.,.F.,.F.,.F.,(3,3),(2,2),(0.,1.),(0.,0.0300000000000002),
 .UNSPECIFIED.);
#370=B_SPLINE_SURFACE_WITH_KNOTS('',2,1,((#43814,#43815),(#43816,#43817),
(#43818,#43819)),.UNSPECIFIED.,.F.,.F.,.F.,(3,3),(2,2),(0.,1.),(0.,0.0300000000000002),
 .UNSPECIFIED.);
#371=B_SPLINE_SURFACE_WITH_KNOTS('',2,1,((#43829,#43830),(#43831,#43832),
(#43833,#43834)),.UNSPECIFIED.,.F.,.F.,.F.,(3,3),(2,2),(0.,1.),(0.,0.0300000000000002),
 .UNSPECIFIED.);
#372=B_SPLINE_SURFACE_WITH_KNOTS('',2,1,((#43844,#43845),(#43846,#43847),
(#43848,#43849)),.UNSPECIFIED.,.F.,.F.,.F.,(3,3),(2,2),(0.,1.),(0.,0.0300000000000002),
 .UNSPECIFIED.);
#373=B_SPLINE_SURFACE_WITH_KNOTS('',2,1,((#43856,#43857),(#43858,#43859),
(#43860,#43861)),.UNSPECIFIED.,.F.,.F.,.F.,(3,3),(2,2),(0.,1.),(0.,0.0300000000000002),
 .UNSPECIFIED.);
#374=B_SPLINE_SURFACE_WITH_KNOTS('',2,1,((#43874,#43875),(#43876,#43877),
(#43878,#43879)),.UNSPECIFIED.,.F.,.F.,.F.,(3,3),(2,2),(0.,1.),(0.,0.0300000000000002),
 .UNSPECIFIED.);
#375=B_SPLINE_SURFACE_WITH_KNOTS('',2,1,((#43889,#43890),(#43891,#43892),
(#43893,#43894)),.UNSPECIFIED.,.F.,.F.,.F.,(3,3),(2,2),(0.,1.),(0.,0.0300000000000002),
 .UNSPECIFIED.);
#376=B_SPLINE_SURFACE_WITH_KNOTS('',2,1,((#43904,#43905),(#43906,#43907),
(#43908,#43909)),.UNSPECIFIED.,.F.,.F.,.F.,(3,3),(2,2),(0.,1.),(0.,0.0300000000000002),
 .UNSPECIFIED.);
#377=B_SPLINE_SURFACE_WITH_KNOTS('',2,1,((#43919,#43920),(#43921,#43922),
(#43923,#43924)),.UNSPECIFIED.,.F.,.F.,.F.,(3,3),(2,2),(0.,1.),(0.,0.0300000000000002),
 .UNSPECIFIED.);
#378=B_SPLINE_SURFACE_WITH_KNOTS('',2,1,((#43934,#43935),(#43936,#43937),
(#43938,#43939)),.UNSPECIFIED.,.F.,.F.,.F.,(3,3),(2,2),(0.,1.),(0.,0.0300000000000002),
 .UNSPECIFIED.);
#379=B_SPLINE_SURFACE_WITH_KNOTS('',2,1,((#43949,#43950),(#43951,#43952),
(#43953,#43954)),.UNSPECIFIED.,.F.,.F.,.F.,(3,3),(2,2),(0.,1.),(0.,0.0300000000000002),
 .UNSPECIFIED.);
#380=B_SPLINE_SURFACE_WITH_KNOTS('',2,1,((#43964,#43965),(#43966,#43967),
(#43968,#43969)),.UNSPECIFIED.,.F.,.F.,.F.,(3,3),(2,2),(0.,1.),(0.,0.0300000000000002),
 .UNSPECIFIED.);
#381=B_SPLINE_SURFACE_WITH_KNOTS('',2,1,((#43979,#43980),(#43981,#43982),
(#43983,#43984)),.UNSPECIFIED.,.F.,.F.,.F.,(3,3),(2,2),(0.,1.),(0.,0.0300000000000002),
 .UNSPECIFIED.);
#382=B_SPLINE_SURFACE_WITH_KNOTS('',2,1,((#43994,#43995),(#43996,#43997),
(#43998,#43999)),.UNSPECIFIED.,.F.,.F.,.F.,(3,3),(2,2),(0.,1.),(0.,0.0300000000000002),
 .UNSPECIFIED.);
#383=B_SPLINE_SURFACE_WITH_KNOTS('',2,1,((#44009,#44010),(#44011,#44012),
(#44013,#44014)),.UNSPECIFIED.,.F.,.F.,.F.,(3,3),(2,2),(0.,1.),(0.,0.0300000000000002),
 .UNSPECIFIED.);
#384=B_SPLINE_SURFACE_WITH_KNOTS('',2,1,((#44024,#44025),(#44026,#44027),
(#44028,#44029)),.UNSPECIFIED.,.F.,.F.,.F.,(3,3),(2,2),(0.,1.),(0.,0.0300000000000002),
 .UNSPECIFIED.);
#385=B_SPLINE_SURFACE_WITH_KNOTS('',2,1,((#44037,#44038),(#44039,#44040),
(#44041,#44042)),.UNSPECIFIED.,.F.,.F.,.F.,(3,3),(2,2),(0.,1.),(0.,0.0300000000000002),
 .UNSPECIFIED.);
#386=B_SPLINE_SURFACE_WITH_KNOTS('',2,1,((#44055,#44056),(#44057,#44058),
(#44059,#44060)),.UNSPECIFIED.,.F.,.F.,.F.,(3,3),(2,2),(0.,1.),(0.,0.0300000000000002),
 .UNSPECIFIED.);
#387=B_SPLINE_SURFACE_WITH_KNOTS('',2,1,((#44076,#44077),(#44078,#44079),
(#44080,#44081)),.UNSPECIFIED.,.F.,.F.,.F.,(3,3),(2,2),(0.,1.),(0.,0.0300000000000002),
 .UNSPECIFIED.);
#388=B_SPLINE_SURFACE_WITH_KNOTS('',2,1,((#44091,#44092),(#44093,#44094),
(#44095,#44096)),.UNSPECIFIED.,.F.,.F.,.F.,(3,3),(2,2),(0.,1.),(0.,0.0300000000000002),
 .UNSPECIFIED.);
#389=B_SPLINE_SURFACE_WITH_KNOTS('',2,1,((#44179,#44180),(#44181,#44182),
(#44183,#44184)),.UNSPECIFIED.,.F.,.F.,.F.,(3,3),(2,2),(0.,1.),(0.,0.0300000000000002),
 .UNSPECIFIED.);
#390=B_SPLINE_SURFACE_WITH_KNOTS('',2,1,((#44194,#44195),(#44196,#44197),
(#44198,#44199)),.UNSPECIFIED.,.F.,.F.,.F.,(3,3),(2,2),(0.,1.),(0.,0.0300000000000002),
 .UNSPECIFIED.);
#391=B_SPLINE_SURFACE_WITH_KNOTS('',2,1,((#44237,#44238),(#44239,#44240),
(#44241,#44242)),.UNSPECIFIED.,.F.,.F.,.F.,(3,3),(2,2),(0.,1.),(0.,0.0300000000000002),
 .UNSPECIFIED.);
#392=B_SPLINE_SURFACE_WITH_KNOTS('',2,1,((#44255,#44256),(#44257,#44258),
(#44259,#44260)),.UNSPECIFIED.,.F.,.F.,.F.,(3,3),(2,2),(0.,1.),(0.,0.0300000000000002),
 .UNSPECIFIED.);
#393=B_SPLINE_SURFACE_WITH_KNOTS('',2,1,((#44270,#44271),(#44272,#44273),
(#44274,#44275)),.UNSPECIFIED.,.F.,.F.,.F.,(3,3),(2,2),(0.,1.),(0.,0.0300000000000002),
 .UNSPECIFIED.);
#394=B_SPLINE_SURFACE_WITH_KNOTS('',2,1,((#44285,#44286),(#44287,#44288),
(#44289,#44290)),.UNSPECIFIED.,.F.,.F.,.F.,(3,3),(2,2),(0.,1.),(0.,0.0300000000000002),
 .UNSPECIFIED.);
#395=B_SPLINE_SURFACE_WITH_KNOTS('',2,1,((#44300,#44301),(#44302,#44303),
(#44304,#44305)),.UNSPECIFIED.,.F.,.F.,.F.,(3,3),(2,2),(0.,1.),(0.,0.0300000000000002),
 .UNSPECIFIED.);
#396=B_SPLINE_SURFACE_WITH_KNOTS('',2,1,((#44315,#44316),(#44317,#44318),
(#44319,#44320)),.UNSPECIFIED.,.F.,.F.,.F.,(3,3),(2,2),(0.,1.),(0.,0.0300000000000002),
 .UNSPECIFIED.);
#397=B_SPLINE_SURFACE_WITH_KNOTS('',2,1,((#44330,#44331),(#44332,#44333),
(#44334,#44335)),.UNSPECIFIED.,.F.,.F.,.F.,(3,3),(2,2),(0.,1.),(0.,0.0300000000000002),
 .UNSPECIFIED.);
#398=B_SPLINE_SURFACE_WITH_KNOTS('',2,1,((#44345,#44346),(#44347,#44348),
(#44349,#44350)),.UNSPECIFIED.,.F.,.F.,.F.,(3,3),(2,2),(0.,1.),(0.,0.0300000000000002),
 .UNSPECIFIED.);
#399=B_SPLINE_SURFACE_WITH_KNOTS('',2,1,((#44360,#44361),(#44362,#44363),
(#44364,#44365)),.UNSPECIFIED.,.F.,.F.,.F.,(3,3),(2,2),(0.,1.),(0.,0.0300000000000002),
 .UNSPECIFIED.);
#400=B_SPLINE_SURFACE_WITH_KNOTS('',2,1,((#44375,#44376),(#44377,#44378),
(#44379,#44380)),.UNSPECIFIED.,.F.,.F.,.F.,(3,3),(2,2),(0.,1.),(0.,0.0300000000000002),
 .UNSPECIFIED.);
#401=B_SPLINE_SURFACE_WITH_KNOTS('',2,1,((#44390,#44391),(#44392,#44393),
(#44394,#44395)),.UNSPECIFIED.,.F.,.F.,.F.,(3,3),(2,2),(0.,1.),(0.,0.0300000000000002),
 .UNSPECIFIED.);
#402=B_SPLINE_SURFACE_WITH_KNOTS('',2,1,((#44411,#44412),(#44413,#44414),
(#44415,#44416)),.UNSPECIFIED.,.F.,.F.,.F.,(3,3),(2,2),(0.,1.),(0.,0.0300000000000002),
 .UNSPECIFIED.);
#403=B_SPLINE_SURFACE_WITH_KNOTS('',2,1,((#44426,#44427),(#44428,#44429),
(#44430,#44431)),.UNSPECIFIED.,.F.,.F.,.F.,(3,3),(2,2),(0.,1.),(0.,0.0300000000000002),
 .UNSPECIFIED.);
#404=B_SPLINE_SURFACE_WITH_KNOTS('',2,1,((#44441,#44442),(#44443,#44444),
(#44445,#44446)),.UNSPECIFIED.,.F.,.F.,.F.,(3,3),(2,2),(0.,1.),(0.,0.0300000000000002),
 .UNSPECIFIED.);
#405=B_SPLINE_SURFACE_WITH_KNOTS('',2,1,((#44456,#44457),(#44458,#44459),
(#44460,#44461)),.UNSPECIFIED.,.F.,.F.,.F.,(3,3),(2,2),(0.,1.),(0.,0.0300000000000002),
 .UNSPECIFIED.);
#406=B_SPLINE_SURFACE_WITH_KNOTS('',2,1,((#44471,#44472),(#44473,#44474),
(#44475,#44476)),.UNSPECIFIED.,.F.,.F.,.F.,(3,3),(2,2),(0.,1.),(0.,0.0300000000000002),
 .UNSPECIFIED.);
#407=B_SPLINE_SURFACE_WITH_KNOTS('',2,1,((#44486,#44487),(#44488,#44489),
(#44490,#44491)),.UNSPECIFIED.,.F.,.F.,.F.,(3,3),(2,2),(0.,1.),(0.,0.0300000000000002),
 .UNSPECIFIED.);
#408=B_SPLINE_SURFACE_WITH_KNOTS('',2,1,((#44501,#44502),(#44503,#44504),
(#44505,#44506)),.UNSPECIFIED.,.F.,.F.,.F.,(3,3),(2,2),(0.,1.),(0.,0.0300000000000002),
 .UNSPECIFIED.);
#409=B_SPLINE_SURFACE_WITH_KNOTS('',2,1,((#44522,#44523),(#44524,#44525),
(#44526,#44527)),.UNSPECIFIED.,.F.,.F.,.F.,(3,3),(2,2),(0.,1.),(0.,0.0300000000000002),
 .UNSPECIFIED.);
#410=B_SPLINE_SURFACE_WITH_KNOTS('',2,1,((#44537,#44538),(#44539,#44540),
(#44541,#44542)),.UNSPECIFIED.,.F.,.F.,.F.,(3,3),(2,2),(0.,1.),(0.,0.0300000000000002),
 .UNSPECIFIED.);
#411=B_SPLINE_SURFACE_WITH_KNOTS('',2,1,((#44552,#44553),(#44554,#44555),
(#44556,#44557)),.UNSPECIFIED.,.F.,.F.,.F.,(3,3),(2,2),(0.,1.),(0.,0.0300000000000002),
 .UNSPECIFIED.);
#412=B_SPLINE_SURFACE_WITH_KNOTS('',2,1,((#44567,#44568),(#44569,#44570),
(#44571,#44572)),.UNSPECIFIED.,.F.,.F.,.F.,(3,3),(2,2),(0.,1.),(0.,0.0300000000000002),
 .UNSPECIFIED.);
#413=B_SPLINE_SURFACE_WITH_KNOTS('',2,1,((#44582,#44583),(#44584,#44585),
(#44586,#44587)),.UNSPECIFIED.,.F.,.F.,.F.,(3,3),(2,2),(0.,1.),(0.,0.0300000000000002),
 .UNSPECIFIED.);
#414=B_SPLINE_SURFACE_WITH_KNOTS('',2,1,((#44597,#44598),(#44599,#44600),
(#44601,#44602)),.UNSPECIFIED.,.F.,.F.,.F.,(3,3),(2,2),(0.,1.),(0.,0.0300000000000002),
 .UNSPECIFIED.);
#415=B_SPLINE_SURFACE_WITH_KNOTS('',2,1,((#44612,#44613),(#44614,#44615),
(#44616,#44617)),.UNSPECIFIED.,.F.,.F.,.F.,(3,3),(2,2),(0.,1.),(0.,0.0300000000000002),
 .UNSPECIFIED.);
#416=B_SPLINE_SURFACE_WITH_KNOTS('',2,1,((#44633,#44634),(#44635,#44636),
(#44637,#44638)),.UNSPECIFIED.,.F.,.F.,.F.,(3,3),(2,2),(0.,1.),(0.,0.0300000000000002),
 .UNSPECIFIED.);
#417=B_SPLINE_SURFACE_WITH_KNOTS('',2,1,((#44648,#44649),(#44650,#44651),
(#44652,#44653)),.UNSPECIFIED.,.F.,.F.,.F.,(3,3),(2,2),(0.,1.),(0.,0.0300000000000002),
 .UNSPECIFIED.);
#418=B_SPLINE_SURFACE_WITH_KNOTS('',2,1,((#44686,#44687),(#44688,#44689),
(#44690,#44691)),.UNSPECIFIED.,.F.,.F.,.F.,(3,3),(2,2),(0.,1.),(0.,0.0300000000000002),
 .UNSPECIFIED.);
#419=B_SPLINE_SURFACE_WITH_KNOTS('',2,1,((#44704,#44705),(#44706,#44707),
(#44708,#44709)),.UNSPECIFIED.,.F.,.F.,.F.,(3,3),(2,2),(0.,1.),(0.,0.0300000000000002),
 .UNSPECIFIED.);
#420=B_SPLINE_SURFACE_WITH_KNOTS('',2,1,((#44783,#44784),(#44785,#44786),
(#44787,#44788)),.UNSPECIFIED.,.F.,.F.,.F.,(3,3),(2,2),(0.,1.),(0.,0.0300000000000002),
 .UNSPECIFIED.);
#421=B_SPLINE_SURFACE_WITH_KNOTS('',2,1,((#44801,#44802),(#44803,#44804),
(#44805,#44806)),.UNSPECIFIED.,.F.,.F.,.F.,(3,3),(2,2),(0.,1.),(0.,0.0300000000000002),
 .UNSPECIFIED.);
#422=B_SPLINE_SURFACE_WITH_KNOTS('',2,1,((#44816,#44817),(#44818,#44819),
(#44820,#44821)),.UNSPECIFIED.,.F.,.F.,.F.,(3,3),(2,2),(0.,1.),(0.,0.0300000000000002),
 .UNSPECIFIED.);
#423=B_SPLINE_SURFACE_WITH_KNOTS('',2,1,((#44831,#44832),(#44833,#44834),
(#44835,#44836)),.UNSPECIFIED.,.F.,.F.,.F.,(3,3),(2,2),(0.,1.),(0.,0.0300000000000002),
 .UNSPECIFIED.);
#424=B_SPLINE_SURFACE_WITH_KNOTS('',2,1,((#44846,#44847),(#44848,#44849),
(#44850,#44851)),.UNSPECIFIED.,.F.,.F.,.F.,(3,3),(2,2),(0.,1.),(0.,0.0300000000000002),
 .UNSPECIFIED.);
#425=B_SPLINE_SURFACE_WITH_KNOTS('',2,1,((#44861,#44862),(#44863,#44864),
(#44865,#44866)),.UNSPECIFIED.,.F.,.F.,.F.,(3,3),(2,2),(0.,1.),(0.,0.0300000000000002),
 .UNSPECIFIED.);
#426=B_SPLINE_SURFACE_WITH_KNOTS('',2,1,((#44876,#44877),(#44878,#44879),
(#44880,#44881)),.UNSPECIFIED.,.F.,.F.,.F.,(3,3),(2,2),(0.,1.),(0.,0.0300000000000002),
 .UNSPECIFIED.);
#427=B_SPLINE_SURFACE_WITH_KNOTS('',2,1,((#44891,#44892),(#44893,#44894),
(#44895,#44896)),.UNSPECIFIED.,.F.,.F.,.F.,(3,3),(2,2),(0.,1.),(0.,0.0300000000000002),
 .UNSPECIFIED.);
#428=B_SPLINE_SURFACE_WITH_KNOTS('',2,1,((#44906,#44907),(#44908,#44909),
(#44910,#44911)),.UNSPECIFIED.,.F.,.F.,.F.,(3,3),(2,2),(0.,1.),(0.,0.0300000000000002),
 .UNSPECIFIED.);
#429=B_SPLINE_SURFACE_WITH_KNOTS('',2,1,((#44921,#44922),(#44923,#44924),
(#44925,#44926)),.UNSPECIFIED.,.F.,.F.,.F.,(3,3),(2,2),(0.,1.),(0.,0.0300000000000002),
 .UNSPECIFIED.);
#430=B_SPLINE_SURFACE_WITH_KNOTS('',2,1,((#44936,#44937),(#44938,#44939),
(#44940,#44941)),.UNSPECIFIED.,.F.,.F.,.F.,(3,3),(2,2),(0.,1.),(0.,0.0300000000000002),
 .UNSPECIFIED.);
#431=B_SPLINE_SURFACE_WITH_KNOTS('',2,1,((#44951,#44952),(#44953,#44954),
(#44955,#44956)),.UNSPECIFIED.,.F.,.F.,.F.,(3,3),(2,2),(0.,1.),(0.,0.0300000000000002),
 .UNSPECIFIED.);
#432=B_SPLINE_SURFACE_WITH_KNOTS('',2,1,((#44966,#44967),(#44968,#44969),
(#44970,#44971)),.UNSPECIFIED.,.F.,.F.,.F.,(3,3),(2,2),(0.,1.),(0.,0.0300000000000002),
 .UNSPECIFIED.);
#433=B_SPLINE_SURFACE_WITH_KNOTS('',2,1,((#44987,#44988),(#44989,#44990),
(#44991,#44992)),.UNSPECIFIED.,.F.,.F.,.F.,(3,3),(2,2),(0.,1.),(0.,0.0300000000000002),
 .UNSPECIFIED.);
#434=B_SPLINE_SURFACE_WITH_KNOTS('',2,1,((#45002,#45003),(#45004,#45005),
(#45006,#45007)),.UNSPECIFIED.,.F.,.F.,.F.,(3,3),(2,2),(0.,1.),(0.,0.0300000000000002),
 .UNSPECIFIED.);
#435=B_SPLINE_SURFACE_WITH_KNOTS('',2,1,((#45017,#45018),(#45019,#45020),
(#45021,#45022)),.UNSPECIFIED.,.F.,.F.,.F.,(3,3),(2,2),(0.,1.),(0.,0.0300000000000002),
 .UNSPECIFIED.);
#436=B_SPLINE_SURFACE_WITH_KNOTS('',2,1,((#45032,#45033),(#45034,#45035),
(#45036,#45037)),.UNSPECIFIED.,.F.,.F.,.F.,(3,3),(2,2),(0.,1.),(0.,0.0300000000000002),
 .UNSPECIFIED.);
#437=B_SPLINE_SURFACE_WITH_KNOTS('',2,1,((#45047,#45048),(#45049,#45050),
(#45051,#45052)),.UNSPECIFIED.,.F.,.F.,.F.,(3,3),(2,2),(0.,1.),(0.,0.0300000000000002),
 .UNSPECIFIED.);
#438=B_SPLINE_SURFACE_WITH_KNOTS('',2,1,((#45062,#45063),(#45064,#45065),
(#45066,#45067)),.UNSPECIFIED.,.F.,.F.,.F.,(3,3),(2,2),(0.,1.),(0.,0.0300000000000002),
 .UNSPECIFIED.);
#439=B_SPLINE_SURFACE_WITH_KNOTS('',2,1,((#45077,#45078),(#45079,#45080),
(#45081,#45082)),.UNSPECIFIED.,.F.,.F.,.F.,(3,3),(2,2),(0.,1.),(0.,0.0300000000000002),
 .UNSPECIFIED.);
#440=B_SPLINE_SURFACE_WITH_KNOTS('',2,1,((#45092,#45093),(#45094,#45095),
(#45096,#45097)),.UNSPECIFIED.,.F.,.F.,.F.,(3,3),(2,2),(0.,1.),(0.,0.0300000000000002),
 .UNSPECIFIED.);
#441=B_SPLINE_SURFACE_WITH_KNOTS('',2,1,((#45107,#45108),(#45109,#45110),
(#45111,#45112)),.UNSPECIFIED.,.F.,.F.,.F.,(3,3),(2,2),(0.,1.),(0.,0.0300000000000002),
 .UNSPECIFIED.);
#442=B_SPLINE_SURFACE_WITH_KNOTS('',2,1,((#45122,#45123),(#45124,#45125),
(#45126,#45127)),.UNSPECIFIED.,.F.,.F.,.F.,(3,3),(2,2),(0.,1.),(0.,0.0300000000000002),
 .UNSPECIFIED.);
#443=B_SPLINE_SURFACE_WITH_KNOTS('',2,1,((#45137,#45138),(#45139,#45140),
(#45141,#45142)),.UNSPECIFIED.,.F.,.F.,.F.,(3,3),(2,2),(0.,1.),(0.,0.0300000000000002),
 .UNSPECIFIED.);
#444=B_SPLINE_SURFACE_WITH_KNOTS('',2,1,((#45152,#45153),(#45154,#45155),
(#45156,#45157)),.UNSPECIFIED.,.F.,.F.,.F.,(3,3),(2,2),(0.,1.),(0.,0.0300000000000002),
 .UNSPECIFIED.);
#445=B_SPLINE_SURFACE_WITH_KNOTS('',2,1,((#45167,#45168),(#45169,#45170),
(#45171,#45172)),.UNSPECIFIED.,.F.,.F.,.F.,(3,3),(2,2),(0.,1.),(0.,0.0300000000000002),
 .UNSPECIFIED.);
#446=B_SPLINE_SURFACE_WITH_KNOTS('',2,1,((#45182,#45183),(#45184,#45185),
(#45186,#45187)),.UNSPECIFIED.,.F.,.F.,.F.,(3,3),(2,2),(0.,1.),(0.,0.0300000000000002),
 .UNSPECIFIED.);
#447=B_SPLINE_SURFACE_WITH_KNOTS('',2,1,((#45197,#45198),(#45199,#45200),
(#45201,#45202)),.UNSPECIFIED.,.F.,.F.,.F.,(3,3),(2,2),(0.,1.),(0.,0.0300000000000002),
 .UNSPECIFIED.);
#448=B_SPLINE_SURFACE_WITH_KNOTS('',2,1,((#45212,#45213),(#45214,#45215),
(#45216,#45217)),.UNSPECIFIED.,.F.,.F.,.F.,(3,3),(2,2),(0.,1.),(0.,0.0300000000000002),
 .UNSPECIFIED.);
#449=B_SPLINE_SURFACE_WITH_KNOTS('',2,1,((#45227,#45228),(#45229,#45230),
(#45231,#45232)),.UNSPECIFIED.,.F.,.F.,.F.,(3,3),(2,2),(0.,1.),(0.,0.0300000000000002),
 .UNSPECIFIED.);
#450=B_SPLINE_SURFACE_WITH_KNOTS('',2,1,((#45242,#45243),(#45244,#45245),
(#45246,#45247)),.UNSPECIFIED.,.F.,.F.,.F.,(3,3),(2,2),(0.,1.),(0.,0.0300000000000002),
 .UNSPECIFIED.);
#451=B_SPLINE_SURFACE_WITH_KNOTS('',2,1,((#45263,#45264),(#45265,#45266),
(#45267,#45268)),.UNSPECIFIED.,.F.,.F.,.F.,(3,3),(2,2),(0.,1.),(0.,0.0300000000000002),
 .UNSPECIFIED.);
#452=B_SPLINE_SURFACE_WITH_KNOTS('',2,1,((#45278,#45279),(#45280,#45281),
(#45282,#45283)),.UNSPECIFIED.,.F.,.F.,.F.,(3,3),(2,2),(0.,1.),(0.,0.0300000000000002),
 .UNSPECIFIED.);
#453=B_SPLINE_SURFACE_WITH_KNOTS('',2,1,((#45291,#45292),(#45293,#45294),
(#45295,#45296)),.UNSPECIFIED.,.F.,.F.,.F.,(3,3),(2,2),(0.,1.),(0.,0.0300000000000002),
 .UNSPECIFIED.);
#454=B_SPLINE_SURFACE_WITH_KNOTS('',2,1,((#45309,#45310),(#45311,#45312),
(#45313,#45314)),.UNSPECIFIED.,.F.,.F.,.F.,(3,3),(2,2),(0.,1.),(0.,0.0300000000000002),
 .UNSPECIFIED.);
#455=B_SPLINE_SURFACE_WITH_KNOTS('',2,1,((#45324,#45325),(#45326,#45327),
(#45328,#45329)),.UNSPECIFIED.,.F.,.F.,.F.,(3,3),(2,2),(0.,1.),(0.,0.0300000000000002),
 .UNSPECIFIED.);
#456=B_SPLINE_SURFACE_WITH_KNOTS('',2,1,((#45339,#45340),(#45341,#45342),
(#45343,#45344)),.UNSPECIFIED.,.F.,.F.,.F.,(3,3),(2,2),(0.,1.),(0.,0.0300000000000002),
 .UNSPECIFIED.);
#457=B_SPLINE_SURFACE_WITH_KNOTS('',2,1,((#45354,#45355),(#45356,#45357),
(#45358,#45359)),.UNSPECIFIED.,.F.,.F.,.F.,(3,3),(2,2),(0.,1.),(0.,0.0300000000000002),
 .UNSPECIFIED.);
#458=B_SPLINE_SURFACE_WITH_KNOTS('',2,1,((#45369,#45370),(#45371,#45372),
(#45373,#45374)),.UNSPECIFIED.,.F.,.F.,.F.,(3,3),(2,2),(0.,1.),(0.,0.0300000000000002),
 .UNSPECIFIED.);
#459=B_SPLINE_SURFACE_WITH_KNOTS('',2,1,((#45384,#45385),(#45386,#45387),
(#45388,#45389)),.UNSPECIFIED.,.F.,.F.,.F.,(3,3),(2,2),(0.,1.),(0.,0.0300000000000002),
 .UNSPECIFIED.);
#460=B_SPLINE_SURFACE_WITH_KNOTS('',2,1,((#45399,#45400),(#45401,#45402),
(#45403,#45404)),.UNSPECIFIED.,.F.,.F.,.F.,(3,3),(2,2),(0.,1.),(0.,0.0300000000000002),
 .UNSPECIFIED.);
#461=B_SPLINE_SURFACE_WITH_KNOTS('',2,1,((#45414,#45415),(#45416,#45417),
(#45418,#45419)),.UNSPECIFIED.,.F.,.F.,.F.,(3,3),(2,2),(0.,1.),(0.,0.0300000000000002),
 .UNSPECIFIED.);
#462=B_SPLINE_SURFACE_WITH_KNOTS('',2,1,((#45429,#45430),(#45431,#45432),
(#45433,#45434)),.UNSPECIFIED.,.F.,.F.,.F.,(3,3),(2,2),(0.,1.),(0.,0.0300000000000002),
 .UNSPECIFIED.);
#463=B_SPLINE_SURFACE_WITH_KNOTS('',2,1,((#45444,#45445),(#45446,#45447),
(#45448,#45449)),.UNSPECIFIED.,.F.,.F.,.F.,(3,3),(2,2),(0.,1.),(0.,0.0300000000000002),
 .UNSPECIFIED.);
#464=B_SPLINE_SURFACE_WITH_KNOTS('',2,1,((#45465,#45466),(#45467,#45468),
(#45469,#45470)),.UNSPECIFIED.,.F.,.F.,.F.,(3,3),(2,2),(0.,1.),(0.,0.0300000000000002),
 .UNSPECIFIED.);
#465=B_SPLINE_SURFACE_WITH_KNOTS('',2,1,((#45480,#45481),(#45482,#45483),
(#45484,#45485)),.UNSPECIFIED.,.F.,.F.,.F.,(3,3),(2,2),(0.,1.),(0.,0.0300000000000002),
 .UNSPECIFIED.);
#466=B_SPLINE_SURFACE_WITH_KNOTS('',2,1,((#45495,#45496),(#45497,#45498),
(#45499,#45500)),.UNSPECIFIED.,.F.,.F.,.F.,(3,3),(2,2),(0.,1.),(0.,0.0300000000000002),
 .UNSPECIFIED.);
#467=B_SPLINE_SURFACE_WITH_KNOTS('',2,1,((#45510,#45511),(#45512,#45513),
(#45514,#45515)),.UNSPECIFIED.,.F.,.F.,.F.,(3,3),(2,2),(0.,1.),(0.,0.0300000000000002),
 .UNSPECIFIED.);
#468=B_SPLINE_SURFACE_WITH_KNOTS('',2,1,((#45525,#45526),(#45527,#45528),
(#45529,#45530)),.UNSPECIFIED.,.F.,.F.,.F.,(3,3),(2,2),(0.,1.),(0.,0.0300000000000002),
 .UNSPECIFIED.);
#469=B_SPLINE_SURFACE_WITH_KNOTS('',2,1,((#45540,#45541),(#45542,#45543),
(#45544,#45545)),.UNSPECIFIED.,.F.,.F.,.F.,(3,3),(2,2),(0.,1.),(0.,0.0300000000000002),
 .UNSPECIFIED.);
#470=B_SPLINE_SURFACE_WITH_KNOTS('',2,1,((#45555,#45556),(#45557,#45558),
(#45559,#45560)),.UNSPECIFIED.,.F.,.F.,.F.,(3,3),(2,2),(0.,1.),(0.,0.0300000000000002),
 .UNSPECIFIED.);
#471=B_SPLINE_SURFACE_WITH_KNOTS('',2,1,((#45576,#45577),(#45578,#45579),
(#45580,#45581)),.UNSPECIFIED.,.F.,.F.,.F.,(3,3),(2,2),(0.,1.),(0.,0.0300000000000002),
 .UNSPECIFIED.);
#472=B_SPLINE_SURFACE_WITH_KNOTS('',2,1,((#45591,#45592),(#45593,#45594),
(#45595,#45596)),.UNSPECIFIED.,.F.,.F.,.F.,(3,3),(2,2),(0.,1.),(0.,0.0300000000000002),
 .UNSPECIFIED.);
#473=B_SPLINE_SURFACE_WITH_KNOTS('',2,1,((#45606,#45607),(#45608,#45609),
(#45610,#45611)),.UNSPECIFIED.,.F.,.F.,.F.,(3,3),(2,2),(0.,1.),(0.,0.0300000000000002),
 .UNSPECIFIED.);
#474=B_SPLINE_SURFACE_WITH_KNOTS('',2,1,((#45621,#45622),(#45623,#45624),
(#45625,#45626)),.UNSPECIFIED.,.F.,.F.,.F.,(3,3),(2,2),(0.,1.),(0.,0.0300000000000002),
 .UNSPECIFIED.);
#475=B_SPLINE_SURFACE_WITH_KNOTS('',2,1,((#45636,#45637),(#45638,#45639),
(#45640,#45641)),.UNSPECIFIED.,.F.,.F.,.F.,(3,3),(2,2),(0.,1.),(0.,0.0300000000000002),
 .UNSPECIFIED.);
#476=B_SPLINE_SURFACE_WITH_KNOTS('',2,1,((#45651,#45652),(#45653,#45654),
(#45655,#45656)),.UNSPECIFIED.,.F.,.F.,.F.,(3,3),(2,2),(0.,1.),(0.,0.0300000000000002),
 .UNSPECIFIED.);
#477=B_SPLINE_SURFACE_WITH_KNOTS('',2,1,((#45666,#45667),(#45668,#45669),
(#45670,#45671)),.UNSPECIFIED.,.F.,.F.,.F.,(3,3),(2,2),(0.,1.),(0.,0.0300000000000002),
 .UNSPECIFIED.);
#478=B_SPLINE_SURFACE_WITH_KNOTS('',2,1,((#45687,#45688),(#45689,#45690),
(#45691,#45692)),.UNSPECIFIED.,.F.,.F.,.F.,(3,3),(2,2),(0.,1.),(0.,0.0300000000000002),
 .UNSPECIFIED.);
#479=B_SPLINE_SURFACE_WITH_KNOTS('',2,1,((#45702,#45703),(#45704,#45705),
(#45706,#45707)),.UNSPECIFIED.,.F.,.F.,.F.,(3,3),(2,2),(0.,1.),(0.,0.0300000000000002),
 .UNSPECIFIED.);
#480=B_SPLINE_SURFACE_WITH_KNOTS('',2,1,((#45715,#45716),(#45717,#45718),
(#45719,#45720)),.UNSPECIFIED.,.F.,.F.,.F.,(3,3),(2,2),(0.,1.),(0.,0.0300000000000002),
 .UNSPECIFIED.);
#481=B_SPLINE_SURFACE_WITH_KNOTS('',2,1,((#45733,#45734),(#45735,#45736),
(#45737,#45738)),.UNSPECIFIED.,.F.,.F.,.F.,(3,3),(2,2),(0.,1.),(0.,0.0300000000000002),
 .UNSPECIFIED.);
#482=B_SPLINE_SURFACE_WITH_KNOTS('',2,1,((#45748,#45749),(#45750,#45751),
(#45752,#45753)),.UNSPECIFIED.,.F.,.F.,.F.,(3,3),(2,2),(0.,1.),(0.,0.0300000000000002),
 .UNSPECIFIED.);
#483=B_SPLINE_SURFACE_WITH_KNOTS('',2,1,((#45763,#45764),(#45765,#45766),
(#45767,#45768)),.UNSPECIFIED.,.F.,.F.,.F.,(3,3),(2,2),(0.,1.),(0.,0.0300000000000002),
 .UNSPECIFIED.);
#484=B_SPLINE_SURFACE_WITH_KNOTS('',2,1,((#45778,#45779),(#45780,#45781),
(#45782,#45783)),.UNSPECIFIED.,.F.,.F.,.F.,(3,3),(2,2),(0.,1.),(0.,0.0300000000000002),
 .UNSPECIFIED.);
#485=B_SPLINE_SURFACE_WITH_KNOTS('',2,1,((#45793,#45794),(#45795,#45796),
(#45797,#45798)),.UNSPECIFIED.,.F.,.F.,.F.,(3,3),(2,2),(0.,1.),(0.,0.0300000000000002),
 .UNSPECIFIED.);
#486=B_SPLINE_SURFACE_WITH_KNOTS('',2,1,((#45808,#45809),(#45810,#45811),
(#45812,#45813)),.UNSPECIFIED.,.F.,.F.,.F.,(3,3),(2,2),(0.,1.),(0.,0.0300000000000002),
 .UNSPECIFIED.);
#487=B_SPLINE_SURFACE_WITH_KNOTS('',2,1,((#45823,#45824),(#45825,#45826),
(#45827,#45828)),.UNSPECIFIED.,.F.,.F.,.F.,(3,3),(2,2),(0.,1.),(0.,0.0300000000000002),
 .UNSPECIFIED.);
#488=B_SPLINE_SURFACE_WITH_KNOTS('',2,1,((#45844,#45845),(#45846,#45847),
(#45848,#45849)),.UNSPECIFIED.,.F.,.F.,.F.,(3,3),(2,2),(0.,1.),(0.,0.0300000000000002),
 .UNSPECIFIED.);
#489=B_SPLINE_SURFACE_WITH_KNOTS('',2,1,((#45859,#45860),(#45861,#45862),
(#45863,#45864)),.UNSPECIFIED.,.F.,.F.,.F.,(3,3),(2,2),(0.,1.),(0.,0.0300000000000002),
 .UNSPECIFIED.);
#490=B_SPLINE_SURFACE_WITH_KNOTS('',2,1,((#45874,#45875),(#45876,#45877),
(#45878,#45879)),.UNSPECIFIED.,.F.,.F.,.F.,(3,3),(2,2),(0.,1.),(0.,0.0300000000000002),
 .UNSPECIFIED.);
#491=B_SPLINE_SURFACE_WITH_KNOTS('',2,1,((#45889,#45890),(#45891,#45892),
(#45893,#45894)),.UNSPECIFIED.,.F.,.F.,.F.,(3,3),(2,2),(0.,1.),(0.,0.0300000000000002),
 .UNSPECIFIED.);
#492=B_SPLINE_SURFACE_WITH_KNOTS('',2,1,((#45904,#45905),(#45906,#45907),
(#45908,#45909)),.UNSPECIFIED.,.F.,.F.,.F.,(3,3),(2,2),(0.,1.),(0.,0.0300000000000002),
 .UNSPECIFIED.);
#493=B_SPLINE_SURFACE_WITH_KNOTS('',2,1,((#45919,#45920),(#45921,#45922),
(#45923,#45924)),.UNSPECIFIED.,.F.,.F.,.F.,(3,3),(2,2),(0.,1.),(0.,0.0300000000000002),
 .UNSPECIFIED.);
#494=B_SPLINE_SURFACE_WITH_KNOTS('',2,1,((#45934,#45935),(#45936,#45937),
(#45938,#45939)),.UNSPECIFIED.,.F.,.F.,.F.,(3,3),(2,2),(0.,1.),(0.,0.0300000000000002),
 .UNSPECIFIED.);
#495=B_SPLINE_SURFACE_WITH_KNOTS('',2,1,((#45949,#45950),(#45951,#45952),
(#45953,#45954)),.UNSPECIFIED.,.F.,.F.,.F.,(3,3),(2,2),(0.,1.),(0.,0.0300000000000002),
 .UNSPECIFIED.);
#496=B_SPLINE_SURFACE_WITH_KNOTS('',2,1,((#45964,#45965),(#45966,#45967),
(#45968,#45969)),.UNSPECIFIED.,.F.,.F.,.F.,(3,3),(2,2),(0.,1.),(0.,0.0300000000000002),
 .UNSPECIFIED.);
#497=B_SPLINE_SURFACE_WITH_KNOTS('',2,1,((#45997,#45998),(#45999,#46000),
(#46001,#46002)),.UNSPECIFIED.,.F.,.F.,.F.,(3,3),(2,2),(0.,1.),(0.,0.0300000000000002),
 .UNSPECIFIED.);
#498=B_SPLINE_SURFACE_WITH_KNOTS('',2,1,((#46019,#46020),(#46021,#46022),
(#46023,#46024)),.UNSPECIFIED.,.F.,.F.,.F.,(3,3),(2,2),(0.,1.),(0.,0.0300000000000002),
 .UNSPECIFIED.);
#499=B_SPLINE_SURFACE_WITH_KNOTS('',2,1,((#46034,#46035),(#46036,#46037),
(#46038,#46039)),.UNSPECIFIED.,.F.,.F.,.F.,(3,3),(2,2),(0.,1.),(0.,0.0300000000000002),
 .UNSPECIFIED.);
#500=B_SPLINE_SURFACE_WITH_KNOTS('',2,1,((#46049,#46050),(#46051,#46052),
(#46053,#46054)),.UNSPECIFIED.,.F.,.F.,.F.,(3,3),(2,2),(0.,1.),(0.,0.0300000000000002),
 .UNSPECIFIED.);
#501=B_SPLINE_SURFACE_WITH_KNOTS('',2,1,((#46064,#46065),(#46066,#46067),
(#46068,#46069)),.UNSPECIFIED.,.F.,.F.,.F.,(3,3),(2,2),(0.,1.),(0.,0.0300000000000002),
 .UNSPECIFIED.);
#502=B_SPLINE_SURFACE_WITH_KNOTS('',2,1,((#46079,#46080),(#46081,#46082),
(#46083,#46084)),.UNSPECIFIED.,.F.,.F.,.F.,(3,3),(2,2),(0.,1.),(0.,0.0300000000000002),
 .UNSPECIFIED.);
#503=B_SPLINE_SURFACE_WITH_KNOTS('',2,1,((#46112,#46113),(#46114,#46115),
(#46116,#46117)),.UNSPECIFIED.,.F.,.F.,.F.,(3,3),(2,2),(0.,1.),(0.,0.0300000000000002),
 .UNSPECIFIED.);
#504=B_SPLINE_SURFACE_WITH_KNOTS('',2,1,((#46127,#46128),(#46129,#46130),
(#46131,#46132)),.UNSPECIFIED.,.F.,.F.,.F.,(3,3),(2,2),(0.,1.),(0.,0.0300000000000002),
 .UNSPECIFIED.);
#505=B_SPLINE_SURFACE_WITH_KNOTS('',2,1,((#46142,#46143),(#46144,#46145),
(#46146,#46147)),.UNSPECIFIED.,.F.,.F.,.F.,(3,3),(2,2),(0.,1.),(0.,0.0300000000000002),
 .UNSPECIFIED.);
#506=B_SPLINE_SURFACE_WITH_KNOTS('',2,1,((#46157,#46158),(#46159,#46160),
(#46161,#46162)),.UNSPECIFIED.,.F.,.F.,.F.,(3,3),(2,2),(0.,1.),(0.,0.0300000000000002),
 .UNSPECIFIED.);
#507=B_SPLINE_SURFACE_WITH_KNOTS('',2,1,((#46172,#46173),(#46174,#46175),
(#46176,#46177)),.UNSPECIFIED.,.F.,.F.,.F.,(3,3),(2,2),(0.,1.),(0.,0.0300000000000002),
 .UNSPECIFIED.);
#508=B_SPLINE_SURFACE_WITH_KNOTS('',2,1,((#46187,#46188),(#46189,#46190),
(#46191,#46192)),.UNSPECIFIED.,.F.,.F.,.F.,(3,3),(2,2),(0.,1.),(0.,0.0300000000000002),
 .UNSPECIFIED.);
#509=B_SPLINE_SURFACE_WITH_KNOTS('',2,1,((#46224,#46225),(#46226,#46227),
(#46228,#46229)),.UNSPECIFIED.,.F.,.F.,.F.,(3,3),(2,2),(0.,1.),(0.,0.0300000000000002),
 .UNSPECIFIED.);
#510=B_SPLINE_SURFACE_WITH_KNOTS('',2,1,((#46242,#46243),(#46244,#46245),
(#46246,#46247)),.UNSPECIFIED.,.F.,.F.,.F.,(3,3),(2,2),(0.,1.),(0.,0.0300000000000002),
 .UNSPECIFIED.);
#511=B_SPLINE_SURFACE_WITH_KNOTS('',2,1,((#46257,#46258),(#46259,#46260),
(#46261,#46262)),.UNSPECIFIED.,.F.,.F.,.F.,(3,3),(2,2),(0.,1.),(0.,0.0300000000000002),
 .UNSPECIFIED.);
#512=B_SPLINE_SURFACE_WITH_KNOTS('',2,1,((#46272,#46273),(#46274,#46275),
(#46276,#46277)),.UNSPECIFIED.,.F.,.F.,.F.,(3,3),(2,2),(0.,1.),(0.,0.0300000000000002),
 .UNSPECIFIED.);
#513=B_SPLINE_SURFACE_WITH_KNOTS('',2,1,((#46287,#46288),(#46289,#46290),
(#46291,#46292)),.UNSPECIFIED.,.F.,.F.,.F.,(3,3),(2,2),(0.,1.),(0.,0.0300000000000002),
 .UNSPECIFIED.);
#514=B_SPLINE_SURFACE_WITH_KNOTS('',2,1,((#46302,#46303),(#46304,#46305),
(#46306,#46307)),.UNSPECIFIED.,.F.,.F.,.F.,(3,3),(2,2),(0.,1.),(0.,0.0300000000000002),
 .UNSPECIFIED.);
#515=B_SPLINE_SURFACE_WITH_KNOTS('',2,1,((#46317,#46318),(#46319,#46320),
(#46321,#46322)),.UNSPECIFIED.,.F.,.F.,.F.,(3,3),(2,2),(0.,1.),(0.,0.0300000000000002),
 .UNSPECIFIED.);
#516=B_SPLINE_SURFACE_WITH_KNOTS('',2,1,((#46332,#46333),(#46334,#46335),
(#46336,#46337)),.UNSPECIFIED.,.F.,.F.,.F.,(3,3),(2,2),(0.,1.),(0.,0.0300000000000002),
 .UNSPECIFIED.);
#517=B_SPLINE_SURFACE_WITH_KNOTS('',2,1,((#46347,#46348),(#46349,#46350),
(#46351,#46352)),.UNSPECIFIED.,.F.,.F.,.F.,(3,3),(2,2),(0.,1.),(0.,0.0300000000000002),
 .UNSPECIFIED.);
#518=B_SPLINE_SURFACE_WITH_KNOTS('',2,1,((#46359,#46360),(#46361,#46362),
(#46363,#46364)),.UNSPECIFIED.,.F.,.F.,.F.,(3,3),(2,2),(0.,1.),(0.,0.0300000000000002),
 .UNSPECIFIED.);
#519=B_SPLINE_SURFACE_WITH_KNOTS('',2,1,((#46377,#46378),(#46379,#46380),
(#46381,#46382)),.UNSPECIFIED.,.F.,.F.,.F.,(3,3),(2,2),(0.,1.),(0.,0.0300000000000002),
 .UNSPECIFIED.);
#520=B_SPLINE_SURFACE_WITH_KNOTS('',2,1,((#46392,#46393),(#46394,#46395),
(#46396,#46397)),.UNSPECIFIED.,.F.,.F.,.F.,(3,3),(2,2),(0.,1.),(0.,0.0300000000000002),
 .UNSPECIFIED.);
#521=B_SPLINE_SURFACE_WITH_KNOTS('',2,1,((#46407,#46408),(#46409,#46410),
(#46411,#46412)),.UNSPECIFIED.,.F.,.F.,.F.,(3,3),(2,2),(0.,1.),(0.,0.0300000000000002),
 .UNSPECIFIED.);
#522=B_SPLINE_SURFACE_WITH_KNOTS('',2,1,((#46422,#46423),(#46424,#46425),
(#46426,#46427)),.UNSPECIFIED.,.F.,.F.,.F.,(3,3),(2,2),(0.,1.),(0.,0.0300000000000002),
 .UNSPECIFIED.);
#523=B_SPLINE_SURFACE_WITH_KNOTS('',2,1,((#46437,#46438),(#46439,#46440),
(#46441,#46442)),.UNSPECIFIED.,.F.,.F.,.F.,(3,3),(2,2),(0.,1.),(0.,0.0300000000000002),
 .UNSPECIFIED.);
#524=B_SPLINE_SURFACE_WITH_KNOTS('',2,1,((#46452,#46453),(#46454,#46455),
(#46456,#46457)),.UNSPECIFIED.,.F.,.F.,.F.,(3,3),(2,2),(0.,1.),(0.,0.0300000000000002),
 .UNSPECIFIED.);
#525=B_SPLINE_SURFACE_WITH_KNOTS('',2,1,((#46467,#46468),(#46469,#46470),
(#46471,#46472)),.UNSPECIFIED.,.F.,.F.,.F.,(3,3),(2,2),(0.,1.),(0.,0.0300000000000002),
 .UNSPECIFIED.);
#526=B_SPLINE_SURFACE_WITH_KNOTS('',2,1,((#46482,#46483),(#46484,#46485),
(#46486,#46487)),.UNSPECIFIED.,.F.,.F.,.F.,(3,3),(2,2),(0.,1.),(0.,0.0300000000000002),
 .UNSPECIFIED.);
#527=B_SPLINE_SURFACE_WITH_KNOTS('',2,1,((#46497,#46498),(#46499,#46500),
(#46501,#46502)),.UNSPECIFIED.,.F.,.F.,.F.,(3,3),(2,2),(0.,1.),(0.,0.0300000000000002),
 .UNSPECIFIED.);
#528=B_SPLINE_SURFACE_WITH_KNOTS('',2,1,((#46512,#46513),(#46514,#46515),
(#46516,#46517)),.UNSPECIFIED.,.F.,.F.,.F.,(3,3),(2,2),(0.,1.),(0.,0.0300000000000002),
 .UNSPECIFIED.);
#529=B_SPLINE_SURFACE_WITH_KNOTS('',2,1,((#46527,#46528),(#46529,#46530),
(#46531,#46532)),.UNSPECIFIED.,.F.,.F.,.F.,(3,3),(2,2),(0.,1.),(0.,0.0300000000000002),
 .UNSPECIFIED.);
#530=B_SPLINE_SURFACE_WITH_KNOTS('',2,1,((#46542,#46543),(#46544,#46545),
(#46546,#46547)),.UNSPECIFIED.,.F.,.F.,.F.,(3,3),(2,2),(0.,1.),(0.,0.0300000000000002),
 .UNSPECIFIED.);
#531=B_SPLINE_SURFACE_WITH_KNOTS('',2,1,((#46557,#46558),(#46559,#46560),
(#46561,#46562)),.UNSPECIFIED.,.F.,.F.,.F.,(3,3),(2,2),(0.,1.),(0.,0.0300000000000002),
 .UNSPECIFIED.);
#532=B_SPLINE_SURFACE_WITH_KNOTS('',2,1,((#46572,#46573),(#46574,#46575),
(#46576,#46577)),.UNSPECIFIED.,.F.,.F.,.F.,(3,3),(2,2),(0.,1.),(0.,0.0300000000000002),
 .UNSPECIFIED.);
#533=B_SPLINE_SURFACE_WITH_KNOTS('',2,1,((#46587,#46588),(#46589,#46590),
(#46591,#46592)),.UNSPECIFIED.,.F.,.F.,.F.,(3,3),(2,2),(0.,1.),(0.,0.0300000000000002),
 .UNSPECIFIED.);
#534=B_SPLINE_SURFACE_WITH_KNOTS('',2,1,((#46608,#46609),(#46610,#46611),
(#46612,#46613)),.UNSPECIFIED.,.F.,.F.,.F.,(3,3),(2,2),(0.,1.),(0.,0.0300000000000002),
 .UNSPECIFIED.);
#535=B_SPLINE_SURFACE_WITH_KNOTS('',2,1,((#46623,#46624),(#46625,#46626),
(#46627,#46628)),.UNSPECIFIED.,.F.,.F.,.F.,(3,3),(2,2),(0.,1.),(0.,0.0300000000000002),
 .UNSPECIFIED.);
#536=B_SPLINE_SURFACE_WITH_KNOTS('',2,1,((#46636,#46637),(#46638,#46639),
(#46640,#46641)),.UNSPECIFIED.,.F.,.F.,.F.,(3,3),(2,2),(0.,1.),(0.,0.0300000000000002),
 .UNSPECIFIED.);
#537=B_SPLINE_SURFACE_WITH_KNOTS('',2,1,((#46654,#46655),(#46656,#46657),
(#46658,#46659)),.UNSPECIFIED.,.F.,.F.,.F.,(3,3),(2,2),(0.,1.),(0.,0.0300000000000002),
 .UNSPECIFIED.);
#538=B_SPLINE_SURFACE_WITH_KNOTS('',2,1,((#46669,#46670),(#46671,#46672),
(#46673,#46674)),.UNSPECIFIED.,.F.,.F.,.F.,(3,3),(2,2),(0.,1.),(0.,0.0300000000000002),
 .UNSPECIFIED.);
#539=B_SPLINE_SURFACE_WITH_KNOTS('',2,1,((#46684,#46685),(#46686,#46687),
(#46688,#46689)),.UNSPECIFIED.,.F.,.F.,.F.,(3,3),(2,2),(0.,1.),(0.,0.0300000000000002),
 .UNSPECIFIED.);
#540=B_SPLINE_SURFACE_WITH_KNOTS('',2,1,((#46699,#46700),(#46701,#46702),
(#46703,#46704)),.UNSPECIFIED.,.F.,.F.,.F.,(3,3),(2,2),(0.,1.),(0.,0.0300000000000002),
 .UNSPECIFIED.);
#541=B_SPLINE_SURFACE_WITH_KNOTS('',2,1,((#46714,#46715),(#46716,#46717),
(#46718,#46719)),.UNSPECIFIED.,.F.,.F.,.F.,(3,3),(2,2),(0.,1.),(0.,0.0300000000000002),
 .UNSPECIFIED.);
#542=B_SPLINE_SURFACE_WITH_KNOTS('',2,1,((#46729,#46730),(#46731,#46732),
(#46733,#46734)),.UNSPECIFIED.,.F.,.F.,.F.,(3,3),(2,2),(0.,1.),(0.,0.0300000000000002),
 .UNSPECIFIED.);
#543=B_SPLINE_SURFACE_WITH_KNOTS('',2,1,((#46744,#46745),(#46746,#46747),
(#46748,#46749)),.UNSPECIFIED.,.F.,.F.,.F.,(3,3),(2,2),(0.,1.),(0.,0.0300000000000002),
 .UNSPECIFIED.);
#544=B_SPLINE_SURFACE_WITH_KNOTS('',2,1,((#46756,#46757),(#46758,#46759),
(#46760,#46761)),.UNSPECIFIED.,.F.,.F.,.F.,(3,3),(2,2),(0.,1.),(0.,0.0300000000000002),
 .UNSPECIFIED.);
#545=B_SPLINE_SURFACE_WITH_KNOTS('',2,1,((#46774,#46775),(#46776,#46777),
(#46778,#46779)),.UNSPECIFIED.,.F.,.F.,.F.,(3,3),(2,2),(0.,1.),(0.,0.0300000000000002),
 .UNSPECIFIED.);
#546=B_SPLINE_SURFACE_WITH_KNOTS('',2,1,((#46789,#46790),(#46791,#46792),
(#46793,#46794)),.UNSPECIFIED.,.F.,.F.,.F.,(3,3),(2,2),(0.,1.),(0.,0.0300000000000002),
 .UNSPECIFIED.);
#547=B_SPLINE_SURFACE_WITH_KNOTS('',2,1,((#46804,#46805),(#46806,#46807),
(#46808,#46809)),.UNSPECIFIED.,.F.,.F.,.F.,(3,3),(2,2),(0.,1.),(0.,0.0300000000000002),
 .UNSPECIFIED.);
#548=B_SPLINE_SURFACE_WITH_KNOTS('',2,1,((#46819,#46820),(#46821,#46822),
(#46823,#46824)),.UNSPECIFIED.,.F.,.F.,.F.,(3,3),(2,2),(0.,1.),(0.,0.0300000000000002),
 .UNSPECIFIED.);
#549=B_SPLINE_SURFACE_WITH_KNOTS('',2,1,((#46834,#46835),(#46836,#46837),
(#46838,#46839)),.UNSPECIFIED.,.F.,.F.,.F.,(3,3),(2,2),(0.,1.),(0.,0.0300000000000002),
 .UNSPECIFIED.);
#550=B_SPLINE_SURFACE_WITH_KNOTS('',2,1,((#46849,#46850),(#46851,#46852),
(#46853,#46854)),.UNSPECIFIED.,.F.,.F.,.F.,(3,3),(2,2),(0.,1.),(0.,0.0300000000000002),
 .UNSPECIFIED.);
#551=B_SPLINE_SURFACE_WITH_KNOTS('',2,1,((#46894,#46895),(#46896,#46897),
(#46898,#46899)),.UNSPECIFIED.,.F.,.F.,.F.,(3,3),(2,2),(0.,1.),(0.,0.0300000000000002),
 .UNSPECIFIED.);
#552=B_SPLINE_SURFACE_WITH_KNOTS('',2,1,((#46907,#46908),(#46909,#46910),
(#46911,#46912)),.UNSPECIFIED.,.F.,.F.,.F.,(3,3),(2,2),(0.,1.),(0.,0.0300000000000002),
 .UNSPECIFIED.);
#553=B_SPLINE_SURFACE_WITH_KNOTS('',2,1,((#46925,#46926),(#46927,#46928),
(#46929,#46930)),.UNSPECIFIED.,.F.,.F.,.F.,(3,3),(2,2),(0.,1.),(0.,0.0300000000000002),
 .UNSPECIFIED.);
#554=B_SPLINE_SURFACE_WITH_KNOTS('',2,1,((#46940,#46941),(#46942,#46943),
(#46944,#46945)),.UNSPECIFIED.,.F.,.F.,.F.,(3,3),(2,2),(0.,1.),(0.,0.0300000000000002),
 .UNSPECIFIED.);
#555=B_SPLINE_SURFACE_WITH_KNOTS('',2,1,((#46955,#46956),(#46957,#46958),
(#46959,#46960)),.UNSPECIFIED.,.F.,.F.,.F.,(3,3),(2,2),(0.,1.),(0.,0.0300000000000002),
 .UNSPECIFIED.);
#556=B_SPLINE_SURFACE_WITH_KNOTS('',2,1,((#46976,#46977),(#46978,#46979),
(#46980,#46981)),.UNSPECIFIED.,.F.,.F.,.F.,(3,3),(2,2),(0.,1.),(0.,0.0300000000000002),
 .UNSPECIFIED.);
#557=B_SPLINE_SURFACE_WITH_KNOTS('',2,1,((#46991,#46992),(#46993,#46994),
(#46995,#46996)),.UNSPECIFIED.,.F.,.F.,.F.,(3,3),(2,2),(0.,1.),(0.,0.0300000000000002),
 .UNSPECIFIED.);
#558=B_SPLINE_SURFACE_WITH_KNOTS('',2,1,((#47006,#47007),(#47008,#47009),
(#47010,#47011)),.UNSPECIFIED.,.F.,.F.,.F.,(3,3),(2,2),(0.,1.),(0.,0.0300000000000002),
 .UNSPECIFIED.);
#559=B_SPLINE_SURFACE_WITH_KNOTS('',3,3,((#50367,#50368,#50369,#50370,#50371,
#50372,#50373,#50374,#50375,#50376,#50377,#50378,#50379,#50380,#50381,#50382,
#50383,#50384,#50385,#50386,#50387,#50388,#50389,#50390,#50391,#50392,#50393,
#50394,#50395,#50396,#50397,#50398,#50399,#50400,#50401,#50402,#50403,#50404,
#50405,#50406,#50407,#50408,#50409,#50410,#50411,#50412,#50413,#50414,#50415,
#50416,#50417,#50418,#50419,#50420,#50421,#50422,#50423,#50424,#50425,#50426,
#50427,#50428,#50429,#50430,#50431,#50432,#50433,#50434,#50435,#50436,#50437,
#50438,#50439,#50440,#50441,#50442,#50443,#50444,#50445,#50446,#50447,#50448,
#50449,#50450,#50451,#50452,#50453,#50454,#50455,#50456,#50457,#50458,#50459,
#50460,#50461,#50462,#50463,#50464,#50465,#50466,#50467,#50468,#50469,#50470,
#50471,#50472,#50473,#50474,#50475,#50476,#50477,#50478,#50479,#50480,#50481,
#50482,#50483,#50484,#50485,#50486,#50487,#50488,#50489,#50490,#50491,#50492,
#50493,#50494,#50495,#50496,#50497,#50498,#50499,#50500,#50501,#50502,#50503,
#50504,#50505,#50506,#50507,#50508,#50509,#50510,#50511,#50512),(#50513,
#50514,#50515,#50516,#50517,#50518,#50519,#50520,#50521,#50522,#50523,#50524,
#50525,#50526,#50527,#50528,#50529,#50530,#50531,#50532,#50533,#50534,#50535,
#50536,#50537,#50538,#50539,#50540,#50541,#50542,#50543,#50544,#50545,#50546,
#50547,#50548,#50549,#50550,#50551,#50552,#50553,#50554,#50555,#50556,#50557,
#50558,#50559,#50560,#50561,#50562,#50563,#50564,#50565,#50566,#50567,#50568,
#50569,#50570,#50571,#50572,#50573,#50574,#50575,#50576,#50577,#50578,#50579,
#50580,#50581,#50582,#50583,#50584,#50585,#50586,#50587,#50588,#50589,#50590,
#50591,#50592,#50593,#50594,#50595,#50596,#50597,#50598,#50599,#50600,#50601,
#50602,#50603,#50604,#50605,#50606,#50607,#50608,#50609,#50610,#50611,#50612,
#50613,#50614,#50615,#50616,#50617,#50618,#50619,#50620,#50621,#50622,#50623,
#50624,#50625,#50626,#50627,#50628,#50629,#50630,#50631,#50632,#50633,#50634,
#50635,#50636,#50637,#50638,#50639,#50640,#50641,#50642,#50643,#50644,#50645,
#50646,#50647,#50648,#50649,#50650,#50651,#50652,#50653,#50654,#50655,#50656,
#50657,#50658),(#50659,#50660,#50661,#50662,#50663,#50664,#50665,#50666,
#50667,#50668,#50669,#50670,#50671,#50672,#50673,#50674,#50675,#50676,#50677,
#50678,#50679,#50680,#50681,#50682,#50683,#50684,#50685,#50686,#50687,#50688,
#50689,#50690,#50691,#50692,#50693,#50694,#50695,#50696,#50697,#50698,#50699,
#50700,#50701,#50702,#50703,#50704,#50705,#50706,#50707,#50708,#50709,#50710,
#50711,#50712,#50713,#50714,#50715,#50716,#50717,#50718,#50719,#50720,#50721,
#50722,#50723,#50724,#50725,#50726,#50727,#50728,#50729,#50730,#50731,#50732,
#50733,#50734,#50735,#50736,#50737,#50738,#50739,#50740,#50741,#50742,#50743,
#50744,#50745,#50746,#50747,#50748,#50749,#50750,#50751,#50752,#50753,#50754,
#50755,#50756,#50757,#50758,#50759,#50760,#50761,#50762,#50763,#50764,#50765,
#50766,#50767,#50768,#50769,#50770,#50771,#50772,#50773,#50774,#50775,#50776,
#50777,#50778,#50779,#50780,#50781,#50782,#50783,#50784,#50785,#50786,#50787,
#50788,#50789,#50790,#50791,#50792,#50793,#50794,#50795,#50796,#50797,#50798,
#50799,#50800,#50801,#50802,#50803,#50804),(#50805,#50806,#50807,#50808,
#50809,#50810,#50811,#50812,#50813,#50814,#50815,#50816,#50817,#50818,#50819,
#50820,#50821,#50822,#50823,#50824,#50825,#50826,#50827,#50828,#50829,#50830,
#50831,#50832,#50833,#50834,#50835,#50836,#50837,#50838,#50839,#50840,#50841,
#50842,#50843,#50844,#50845,#50846,#50847,#50848,#50849,#50850,#50851,#50852,
#50853,#50854,#50855,#50856,#50857,#50858,#50859,#50860,#50861,#50862,#50863,
#50864,#50865,#50866,#50867,#50868,#50869,#50870,#50871,#50872,#50873,#50874,
#50875,#50876,#50877,#50878,#50879,#50880,#50881,#50882,#50883,#50884,#50885,
#50886,#50887,#50888,#50889,#50890,#50891,#50892,#50893,#50894,#50895,#50896,
#50897,#50898,#50899,#50900,#50901,#50902,#50903,#50904,#50905,#50906,#50907,
#50908,#50909,#50910,#50911,#50912,#50913,#50914,#50915,#50916,#50917,#50918,
#50919,#50920,#50921,#50922,#50923,#50924,#50925,#50926,#50927,#50928,#50929,
#50930,#50931,#50932,#50933,#50934,#50935,#50936,#50937,#50938,#50939,#50940,
#50941,#50942,#50943,#50944,#50945,#50946,#50947,#50948,#50949,#50950)),
 .UNSPECIFIED.,.F.,.F.,.F.,(4,4),(4,1,1,1,1,1,1,1,1,1,1,1,1,1,1,1,1,1,1,
1,1,1,1,1,1,1,1,1,1,1,1,1,1,1,1,1,1,1,1,1,1,1,1,1,1,1,1,1,1,1,1,1,1,1,1,
1,1,1,1,1,1,1,1,1,1,1,1,1,1,1,1,1,1,1,1,1,1,1,1,1,1,1,1,1,1,1,1,1,1,1,1,
1,1,1,1,1,1,1,1,1,1,1,1,1,1,1,1,1,1,1,1,1,1,1,1,1,1,1,1,1,1,1,1,1,1,1,1,
1,1,1,1,1,1,1,1,1,1,1,1,1,1,1,1,4),(0.,0.0820126057383863),(13.6780597280665,
14.6766929621808,15.675326196295,16.6739594304093,17.6725926645235,18.6712258986378,
19.6698591327521,20.6684923668663,21.6671256009806,22.6657588350948,23.6643920692091,
24.6630253033233,25.6616585374376,26.6602917715518,27.6589250056661,28.6575582397804,
29.6561914738946,30.6548247080089,31.6534579421231,32.6520911762374,33.6507244103516,
34.6493576444659,35.6479908785801,36.6466241126944,37.6452573468086,38.6438905809229,
39.6425238150372,40.6411570491514,41.6397902832657,42.6384235173799,43.6370567514942,
44.6356899856084,45.6343232197227,46.6329564538369,47.6315896879512,48.6302229220655,
49.6288561561797,50.627489390294,51.6261226244082,52.6247558585225,53.6233890926367,
54.622022326751,55.6206555608652,56.6192887949795,57.6179220290938,58.616555263208,
59.6151884973223,60.6138217314365,61.6124549655508,62.611088199665,63.6097214337793,
64.6083546678935,65.6069879020078,66.6056211361221,67.6042543702363,68.6028876043506,
69.6015208384648,70.6001540725791,71.5987873066933,72.5974205408076,73.5960537749218,
74.5946870090361,75.5933202431503,76.5919534772646,77.5905867113789,78.5892199454931,
79.5878531796074,80.5864864137216,81.5851196478359,82.5837528819501,83.5823861160644,
84.5810193501787,85.5796525842929,86.5782858184072,87.5769190525214,88.5755522866357,
89.5741855207499,90.5728187548642,91.5714519889784,92.5700852230927,93.568718457207,
94.5673516913212,95.5659849254355,96.5646181595497,97.563251393664,98.5618846277782,
99.5605178618925,100.559151096007,101.557784330121,102.556417564235,103.555050798349,
104.553684032464,105.552317266578,106.550950500692,107.549583734807,108.548216968921,
109.546850203035,110.545483437149,111.544116671264,112.542749905378,113.541383139492,
114.540016373606,115.538649607721,116.537282841835,117.535916075949,118.534549310063,
119.533182544178,120.531815778292,121.530449012406,122.52908224652,123.527715480635,
124.526348714749,125.524981948863,126.523615182977,127.522248417092,128.520881651206,
129.51951488532,130.518148119434,131.516781353549,132.515414587663,133.514047821777,
134.512681055891,135.511314290006,136.50994752412,137.508580758234,138.507213992348,
139.505847226463,140.504480460577,141.503113694691,142.501746928805,143.50038016292,
144.499013397034,145.497646631148,146.496279865262,147.494913099377,148.493546333491,
149.492179567605,150.490812801719,151.489446035834,152.488079269948,153.486712504062,
154.485345738177,155.483978972291,156.482612206405),.UNSPECIFIED.);
#560=B_SPLINE_SURFACE_WITH_KNOTS('',3,3,((#51107,#51108,#51109,#51110,#51111,
#51112,#51113,#51114,#51115,#51116,#51117,#51118,#51119,#51120,#51121,#51122,
#51123,#51124,#51125,#51126,#51127,#51128,#51129,#51130,#51131,#51132,#51133,
#51134,#51135,#51136,#51137,#51138,#51139,#51140,#51141,#51142,#51143,#51144,
#51145,#51146,#51147,#51148,#51149,#51150,#51151,#51152,#51153,#51154,#51155,
#51156,#51157,#51158,#51159,#51160,#51161,#51162,#51163,#51164,#51165,#51166,
#51167,#51168,#51169,#51170,#51171,#51172,#51173,#51174,#51175,#51176,#51177,
#51178,#51179,#51180,#51181,#51182,#51183,#51184,#51185,#51186,#51187,#51188,
#51189,#51190,#51191,#51192,#51193,#51194,#51195,#51196,#51197,#51198,#51199,
#51200,#51201,#51202,#51203,#51204,#51205,#51206,#51207,#51208,#51209,#51210,
#51211,#51212,#51213,#51214,#51215,#51216,#51217,#51218,#51219,#51220,#51221,
#51222,#51223,#51224,#51225,#51226,#51227,#51228,#51229,#51230,#51231,#51232,
#51233,#51234,#51235,#51236,#51237,#51238,#51239,#51240,#51241,#51242,#51243,
#51244,#51245,#51246,#51247,#51248,#51249,#51250,#51251,#51252),(#51253,
#51254,#51255,#51256,#51257,#51258,#51259,#51260,#51261,#51262,#51263,#51264,
#51265,#51266,#51267,#51268,#51269,#51270,#51271,#51272,#51273,#51274,#51275,
#51276,#51277,#51278,#51279,#51280,#51281,#51282,#51283,#51284,#51285,#51286,
#51287,#51288,#51289,#51290,#51291,#51292,#51293,#51294,#51295,#51296,#51297,
#51298,#51299,#51300,#51301,#51302,#51303,#51304,#51305,#51306,#51307,#51308,
#51309,#51310,#51311,#51312,#51313,#51314,#51315,#51316,#51317,#51318,#51319,
#51320,#51321,#51322,#51323,#51324,#51325,#51326,#51327,#51328,#51329,#51330,
#51331,#51332,#51333,#51334,#51335,#51336,#51337,#51338,#51339,#51340,#51341,
#51342,#51343,#51344,#51345,#51346,#51347,#51348,#51349,#51350,#51351,#51352,
#51353,#51354,#51355,#51356,#51357,#51358,#51359,#51360,#51361,#51362,#51363,
#51364,#51365,#51366,#51367,#51368,#51369,#51370,#51371,#51372,#51373,#51374,
#51375,#51376,#51377,#51378,#51379,#51380,#51381,#51382,#51383,#51384,#51385,
#51386,#51387,#51388,#51389,#51390,#51391,#51392,#51393,#51394,#51395,#51396,
#51397,#51398),(#51399,#51400,#51401,#51402,#51403,#51404,#51405,#51406,
#51407,#51408,#51409,#51410,#51411,#51412,#51413,#51414,#51415,#51416,#51417,
#51418,#51419,#51420,#51421,#51422,#51423,#51424,#51425,#51426,#51427,#51428,
#51429,#51430,#51431,#51432,#51433,#51434,#51435,#51436,#51437,#51438,#51439,
#51440,#51441,#51442,#51443,#51444,#51445,#51446,#51447,#51448,#51449,#51450,
#51451,#51452,#51453,#51454,#51455,#51456,#51457,#51458,#51459,#51460,#51461,
#51462,#51463,#51464,#51465,#51466,#51467,#51468,#51469,#51470,#51471,#51472,
#51473,#51474,#51475,#51476,#51477,#51478,#51479,#51480,#51481,#51482,#51483,
#51484,#51485,#51486,#51487,#51488,#51489,#51490,#51491,#51492,#51493,#51494,
#51495,#51496,#51497,#51498,#51499,#51500,#51501,#51502,#51503,#51504,#51505,
#51506,#51507,#51508,#51509,#51510,#51511,#51512,#51513,#51514,#51515,#51516,
#51517,#51518,#51519,#51520,#51521,#51522,#51523,#51524,#51525,#51526,#51527,
#51528,#51529,#51530,#51531,#51532,#51533,#51534,#51535,#51536,#51537,#51538,
#51539,#51540,#51541,#51542,#51543,#51544),(#51545,#51546,#51547,#51548,
#51549,#51550,#51551,#51552,#51553,#51554,#51555,#51556,#51557,#51558,#51559,
#51560,#51561,#51562,#51563,#51564,#51565,#51566,#51567,#51568,#51569,#51570,
#51571,#51572,#51573,#51574,#51575,#51576,#51577,#51578,#51579,#51580,#51581,
#51582,#51583,#51584,#51585,#51586,#51587,#51588,#51589,#51590,#51591,#51592,
#51593,#51594,#51595,#51596,#51597,#51598,#51599,#51600,#51601,#51602,#51603,
#51604,#51605,#51606,#51607,#51608,#51609,#51610,#51611,#51612,#51613,#51614,
#51615,#51616,#51617,#51618,#51619,#51620,#51621,#51622,#51623,#51624,#51625,
#51626,#51627,#51628,#51629,#51630,#51631,#51632,#51633,#51634,#51635,#51636,
#51637,#51638,#51639,#51640,#51641,#51642,#51643,#51644,#51645,#51646,#51647,
#51648,#51649,#51650,#51651,#51652,#51653,#51654,#51655,#51656,#51657,#51658,
#51659,#51660,#51661,#51662,#51663,#51664,#51665,#51666,#51667,#51668,#51669,
#51670,#51671,#51672,#51673,#51674,#51675,#51676,#51677,#51678,#51679,#51680,
#51681,#51682,#51683,#51684,#51685,#51686,#51687,#51688,#51689,#51690)),
 .UNSPECIFIED.,.F.,.F.,.F.,(4,4),(4,1,1,1,1,1,1,1,1,1,1,1,1,1,1,1,1,1,1,
1,1,1,1,1,1,1,1,1,1,1,1,1,1,1,1,1,1,1,1,1,1,1,1,1,1,1,1,1,1,1,1,1,1,1,1,
1,1,1,1,1,1,1,1,1,1,1,1,1,1,1,1,1,1,1,1,1,1,1,1,1,1,1,1,1,1,1,1,1,1,1,1,
1,1,1,1,1,1,1,1,1,1,1,1,1,1,1,1,1,1,1,1,1,1,1,1,1,1,1,1,1,1,1,1,1,1,1,1,
1,1,1,1,1,1,1,1,1,1,1,1,1,1,1,1,4),(0.,0.0820126057383863),(16.9785412059632,
17.9771744400775,18.9758076741917,19.974440908306,20.9730741424202,21.9717073765345,
22.9703406106487,23.968973844763,24.9676070788772,25.9662403129915,26.9648735471058,
27.96350678122,28.9621400153343,29.9607732494485,30.9594064835628,31.958039717677,
32.9566729517913,33.9553061859055,34.9539394200198,35.9525726541341,36.9512058882483,
37.9498391223626,38.9484723564768,39.9471055905911,40.9457388247053,41.9443720588196,
42.9430052929338,43.9416385270481,44.9402717611624,45.9389049952766,46.9375382293909,
47.9361714635051,48.9348046976194,49.9334379317336,50.9320711658479,51.9307043999621,
52.9293376340764,53.9279708681906,54.9266041023049,55.9252373364192,56.9238705705334,
57.9225038046477,58.9211370387619,59.9197702728762,60.9184035069904,61.9170367411047,
62.9156699752189,63.9143032093332,64.9129364434474,65.9115696775617,66.910202911676,
67.9088361457902,68.9074693799045,69.9061026140187,70.904735848133,71.9033690822472,
72.9020023163615,73.9006355504758,74.89926878459,75.8979020187043,76.8965352528185,
77.8951684869328,78.893801721047,79.8924349551613,80.8910681892755,81.8897014233898,
82.888334657504,83.8869678916183,84.8856011257326,85.8842343598468,86.8828675939611,
87.8815008280753,88.8801340621896,89.8787672963038,90.8774005304181,91.8760337645324,
92.8746669986466,93.8733002327609,94.8719334668751,95.8705667009894,96.8691999351036,
97.8678331692179,98.8664664033321,99.8650996374464,100.863732871561,101.862366105675,
102.860999339789,103.859632573903,104.858265808018,105.856899042132,106.855532276246,
107.85416551036,108.852798744475,109.851431978589,110.850065212703,111.848698446817,
112.847331680932,113.845964915046,114.84459814916,115.843231383274,116.841864617389,
117.840497851503,118.839131085617,119.837764319731,120.836397553846,121.83503078796,
122.833664022074,123.832297256189,124.830930490303,125.829563724417,126.828196958531,
127.826830192646,128.82546342676,129.824096660874,130.822729894988,131.821363129103,
132.819996363217,133.818629597331,134.817262831445,135.81589606556,136.814529299674,
137.813162533788,138.811795767902,139.810429002017,140.809062236131,141.807695470245,
142.806328704359,143.804961938474,144.803595172588,145.802228406702,146.800861640816,
147.799494874931,148.798128109045,149.796761343159,150.795394577273,151.794027811388,
152.792661045502,153.791294279616,154.78992751373,155.788560747845,156.787193981959,
157.785827216073,158.784460450187,159.783093684302),.UNSPECIFIED.);
#561=B_SPLINE_SURFACE_WITH_KNOTS('',3,3,((#53988,#53989,#53990,#53991,#53992,
#53993,#53994,#53995,#53996,#53997,#53998,#53999,#54000,#54001,#54002,#54003,
#54004,#54005,#54006,#54007,#54008,#54009,#54010,#54011,#54012,#54013,#54014,
#54015,#54016,#54017,#54018,#54019,#54020,#54021,#54022,#54023,#54024,#54025,
#54026,#54027,#54028,#54029,#54030,#54031,#54032,#54033,#54034,#54035,#54036,
#54037,#54038,#54039,#54040,#54041,#54042,#54043,#54044,#54045,#54046,#54047,
#54048,#54049,#54050,#54051,#54052,#54053,#54054,#54055,#54056,#54057,#54058,
#54059,#54060,#54061,#54062,#54063,#54064,#54065,#54066,#54067,#54068,#54069,
#54070,#54071,#54072,#54073,#54074,#54075,#54076,#54077,#54078,#54079,#54080,
#54081,#54082,#54083,#54084,#54085,#54086,#54087,#54088,#54089,#54090,#54091,
#54092,#54093,#54094,#54095,#54096,#54097,#54098,#54099,#54100,#54101,#54102,
#54103,#54104,#54105,#54106,#54107,#54108),(#54109,#54110,#54111,#54112,
#54113,#54114,#54115,#54116,#54117,#54118,#54119,#54120,#54121,#54122,#54123,
#54124,#54125,#54126,#54127,#54128,#54129,#54130,#54131,#54132,#54133,#54134,
#54135,#54136,#54137,#54138,#54139,#54140,#54141,#54142,#54143,#54144,#54145,
#54146,#54147,#54148,#54149,#54150,#54151,#54152,#54153,#54154,#54155,#54156,
#54157,#54158,#54159,#54160,#54161,#54162,#54163,#54164,#54165,#54166,#54167,
#54168,#54169,#54170,#54171,#54172,#54173,#54174,#54175,#54176,#54177,#54178,
#54179,#54180,#54181,#54182,#54183,#54184,#54185,#54186,#54187,#54188,#54189,
#54190,#54191,#54192,#54193,#54194,#54195,#54196,#54197,#54198,#54199,#54200,
#54201,#54202,#54203,#54204,#54205,#54206,#54207,#54208,#54209,#54210,#54211,
#54212,#54213,#54214,#54215,#54216,#54217,#54218,#54219,#54220,#54221,#54222,
#54223,#54224,#54225,#54226,#54227,#54228,#54229),(#54230,#54231,#54232,
#54233,#54234,#54235,#54236,#54237,#54238,#54239,#54240,#54241,#54242,#54243,
#54244,#54245,#54246,#54247,#54248,#54249,#54250,#54251,#54252,#54253,#54254,
#54255,#54256,#54257,#54258,#54259,#54260,#54261,#54262,#54263,#54264,#54265,
#54266,#54267,#54268,#54269,#54270,#54271,#54272,#54273,#54274,#54275,#54276,
#54277,#54278,#54279,#54280,#54281,#54282,#54283,#54284,#54285,#54286,#54287,
#54288,#54289,#54290,#54291,#54292,#54293,#54294,#54295,#54296,#54297,#54298,
#54299,#54300,#54301,#54302,#54303,#54304,#54305,#54306,#54307,#54308,#54309,
#54310,#54311,#54312,#54313,#54314,#54315,#54316,#54317,#54318,#54319,#54320,
#54321,#54322,#54323,#54324,#54325,#54326,#54327,#54328,#54329,#54330,#54331,
#54332,#54333,#54334,#54335,#54336,#54337,#54338,#54339,#54340,#54341,#54342,
#54343,#54344,#54345,#54346,#54347,#54348,#54349,#54350),(#54351,#54352,
#54353,#54354,#54355,#54356,#54357,#54358,#54359,#54360,#54361,#54362,#54363,
#54364,#54365,#54366,#54367,#54368,#54369,#54370,#54371,#54372,#54373,#54374,
#54375,#54376,#54377,#54378,#54379,#54380,#54381,#54382,#54383,#54384,#54385,
#54386,#54387,#54388,#54389,#54390,#54391,#54392,#54393,#54394,#54395,#54396,
#54397,#54398,#54399,#54400,#54401,#54402,#54403,#54404,#54405,#54406,#54407,
#54408,#54409,#54410,#54411,#54412,#54413,#54414,#54415,#54416,#54417,#54418,
#54419,#54420,#54421,#54422,#54423,#54424,#54425,#54426,#54427,#54428,#54429,
#54430,#54431,#54432,#54433,#54434,#54435,#54436,#54437,#54438,#54439,#54440,
#54441,#54442,#54443,#54444,#54445,#54446,#54447,#54448,#54449,#54450,#54451,
#54452,#54453,#54454,#54455,#54456,#54457,#54458,#54459,#54460,#54461,#54462,
#54463,#54464,#54465,#54466,#54467,#54468,#54469,#54470,#54471)),
 .UNSPECIFIED.,.F.,.F.,.F.,(4,4),(4,1,1,1,1,1,1,1,1,1,1,1,1,1,1,1,1,1,1,
1,1,1,1,1,1,1,1,1,1,1,1,1,1,1,1,1,1,1,1,1,1,1,1,1,1,1,1,1,1,1,1,1,1,1,1,
1,1,1,1,1,1,1,1,1,1,1,1,1,1,1,1,1,1,1,1,1,1,1,1,1,1,1,1,1,1,1,1,1,1,1,1,
1,1,1,1,1,1,1,1,1,1,1,1,1,1,1,1,1,1,1,1,1,1,1,1,1,1,1,4),(0.,0.0989001011121828),
(8.30505915324875,8.80095158446445,9.29684401568014,9.79273644689584,10.2886288781115,
10.7845213093272,11.2804137405429,11.7763061717586,12.2721986029743,12.76809103419,
13.2639834654057,13.7598758966214,14.2557683278371,14.7516607590528,15.2475531902685,
15.7434456214842,16.2393380526999,16.7352304839156,17.2311229151313,17.727015346347,
18.2229077775627,18.7188002087784,19.2146926399941,19.7105850712098,20.2064775024255,
20.7023699336412,21.1982623648568,21.6941547960725,22.1900472272882,22.6859396585039,
23.1818320897196,23.6777245209353,24.173616952151,24.6695093833667,25.1654018145824,
25.6612942457981,26.1571866770138,26.6530791082295,27.1489715394452,27.6448639706609,
28.1407564018766,28.6366488330923,29.132541264308,29.6284336955237,30.1243261267394,
30.6202185579551,31.1161109891708,31.6120034203865,32.1078958516022,32.6037882828178,
33.0996807140335,33.5955731452492,34.0914655764649,34.5873580076806,35.0832504388963,
35.579142870112,36.0750353013277,36.5709277325434,37.0668201637591,37.5627125949748,
38.0586050261905,38.5544974574062,39.0503898886219,39.5462823198376,40.0421747510533,
40.538067182269,41.0339596134847,41.5298520447004,42.0257444759161,42.5216369071318,
43.0175293383475,43.5134217695632,44.0093142007789,44.5052066319946,45.0010990632102,
45.4969914944259,45.9928839256416,46.4887763568573,46.984668788073,47.4805612192887,
47.9764536505044,48.4723460817201,48.9682385129358,49.4641309441515,49.9600233753672,
50.4559158065829,50.9518082377986,51.4477006690143,51.94359310023,52.4394855314457,
52.9353779626614,53.4312703938771,53.9271628250928,54.4230552563085,54.9189476875242,
55.4148401187399,55.9107325499556,56.4066249811712,56.9025174123869,57.3984098436026,
57.8943022748183,58.390194706034,58.8860871372497,59.3819795684654,59.8778719996811,
60.3737644308968,60.8696568621125,61.3655492933282,61.8614417245439,62.3573341557596,
62.8532265869753,63.349119018191,63.8450114494067,64.3409038806224,64.8367963118381,
65.3326887430538,65.8285811742695,66.3244736054852,66.8203660367009),
 .UNSPECIFIED.);
#562=B_SPLINE_SURFACE_WITH_KNOTS('',3,3,((#54612,#54613,#54614,#54615,#54616,
#54617,#54618,#54619,#54620,#54621,#54622,#54623,#54624,#54625,#54626,#54627,
#54628,#54629,#54630,#54631,#54632,#54633,#54634,#54635,#54636,#54637,#54638,
#54639,#54640,#54641,#54642,#54643,#54644,#54645,#54646,#54647,#54648,#54649,
#54650,#54651,#54652,#54653,#54654,#54655,#54656,#54657,#54658,#54659,#54660,
#54661,#54662,#54663,#54664,#54665,#54666,#54667,#54668,#54669,#54670,#54671,
#54672,#54673,#54674,#54675,#54676,#54677,#54678,#54679,#54680,#54681,#54682,
#54683,#54684,#54685,#54686,#54687,#54688,#54689,#54690,#54691,#54692,#54693,
#54694,#54695,#54696,#54697,#54698,#54699,#54700,#54701,#54702,#54703,#54704,
#54705,#54706,#54707,#54708,#54709,#54710,#54711,#54712,#54713,#54714,#54715,
#54716,#54717,#54718,#54719,#54720,#54721,#54722,#54723,#54724,#54725,#54726,
#54727,#54728,#54729,#54730,#54731,#54732),(#54733,#54734,#54735,#54736,
#54737,#54738,#54739,#54740,#54741,#54742,#54743,#54744,#54745,#54746,#54747,
#54748,#54749,#54750,#54751,#54752,#54753,#54754,#54755,#54756,#54757,#54758,
#54759,#54760,#54761,#54762,#54763,#54764,#54765,#54766,#54767,#54768,#54769,
#54770,#54771,#54772,#54773,#54774,#54775,#54776,#54777,#54778,#54779,#54780,
#54781,#54782,#54783,#54784,#54785,#54786,#54787,#54788,#54789,#54790,#54791,
#54792,#54793,#54794,#54795,#54796,#54797,#54798,#54799,#54800,#54801,#54802,
#54803,#54804,#54805,#54806,#54807,#54808,#54809,#54810,#54811,#54812,#54813,
#54814,#54815,#54816,#54817,#54818,#54819,#54820,#54821,#54822,#54823,#54824,
#54825,#54826,#54827,#54828,#54829,#54830,#54831,#54832,#54833,#54834,#54835,
#54836,#54837,#54838,#54839,#54840,#54841,#54842,#54843,#54844,#54845,#54846,
#54847,#54848,#54849,#54850,#54851,#54852,#54853),(#54854,#54855,#54856,
#54857,#54858,#54859,#54860,#54861,#54862,#54863,#54864,#54865,#54866,#54867,
#54868,#54869,#54870,#54871,#54872,#54873,#54874,#54875,#54876,#54877,#54878,
#54879,#54880,#54881,#54882,#54883,#54884,#54885,#54886,#54887,#54888,#54889,
#54890,#54891,#54892,#54893,#54894,#54895,#54896,#54897,#54898,#54899,#54900,
#54901,#54902,#54903,#54904,#54905,#54906,#54907,#54908,#54909,#54910,#54911,
#54912,#54913,#54914,#54915,#54916,#54917,#54918,#54919,#54920,#54921,#54922,
#54923,#54924,#54925,#54926,#54927,#54928,#54929,#54930,#54931,#54932,#54933,
#54934,#54935,#54936,#54937,#54938,#54939,#54940,#54941,#54942,#54943,#54944,
#54945,#54946,#54947,#54948,#54949,#54950,#54951,#54952,#54953,#54954,#54955,
#54956,#54957,#54958,#54959,#54960,#54961,#54962,#54963,#54964,#54965,#54966,
#54967,#54968,#54969,#54970,#54971,#54972,#54973,#54974),(#54975,#54976,
#54977,#54978,#54979,#54980,#54981,#54982,#54983,#54984,#54985,#54986,#54987,
#54988,#54989,#54990,#54991,#54992,#54993,#54994,#54995,#54996,#54997,#54998,
#54999,#55000,#55001,#55002,#55003,#55004,#55005,#55006,#55007,#55008,#55009,
#55010,#55011,#55012,#55013,#55014,#55015,#55016,#55017,#55018,#55019,#55020,
#55021,#55022,#55023,#55024,#55025,#55026,#55027,#55028,#55029,#55030,#55031,
#55032,#55033,#55034,#55035,#55036,#55037,#55038,#55039,#55040,#55041,#55042,
#55043,#55044,#55045,#55046,#55047,#55048,#55049,#55050,#55051,#55052,#55053,
#55054,#55055,#55056,#55057,#55058,#55059,#55060,#55061,#55062,#55063,#55064,
#55065,#55066,#55067,#55068,#55069,#55070,#55071,#55072,#55073,#55074,#55075,
#55076,#55077,#55078,#55079,#55080,#55081,#55082,#55083,#55084,#55085,#55086,
#55087,#55088,#55089,#55090,#55091,#55092,#55093,#55094,#55095)),
 .UNSPECIFIED.,.F.,.F.,.F.,(4,4),(4,1,1,1,1,1,1,1,1,1,1,1,1,1,1,1,1,1,1,
1,1,1,1,1,1,1,1,1,1,1,1,1,1,1,1,1,1,1,1,1,1,1,1,1,1,1,1,1,1,1,1,1,1,1,1,
1,1,1,1,1,1,1,1,1,1,1,1,1,1,1,1,1,1,1,1,1,1,1,1,1,1,1,1,1,1,1,1,1,1,1,1,
1,1,1,1,1,1,1,1,1,1,1,1,1,1,1,1,1,1,1,1,1,1,1,1,1,1,1,4),(0.,0.0989001011121828),
(11.6147305479242,12.1106229791399,12.6065154103556,13.1024078415713,13.598300272787,
14.0941927040027,14.5900851352184,15.0859775664341,15.5818699976498,16.0777624288655,
16.5736548600812,17.0695472912969,17.5654397225126,18.0613321537283,18.557224584944,
19.0531170161597,19.5490094473754,20.0449018785911,20.5407943098068,21.0366867410225,
21.5325791722382,22.0284716034539,22.5243640346695,23.0202564658852,23.5161488971009,
24.0120413283166,24.5079337595323,25.003826190748,25.4997186219637,25.9956110531794,
26.4915034843951,26.9873959156108,27.4832883468265,27.9791807780422,28.4750732092579,
28.9709656404736,29.4668580716893,29.962750502905,30.4586429341207,30.9545353653364,
31.4504277965521,31.9463202277678,32.4422126589835,32.9381050901992,33.4339975214149,
33.9298899526305,34.4257823838462,34.9216748150619,35.4175672462776,35.9134596774933,
36.409352108709,36.9052445399247,37.4011369711404,37.8970294023561,38.3929218335718,
38.8888142647875,39.3847066960032,39.8805991272189,40.3764915584346,40.8723839896503,
41.368276420866,41.8641688520817,42.3600612832974,42.8559537145131,43.3518461457288,
43.8477385769445,44.3436310081602,44.8395234393758,45.3354158705915,45.8313083018072,
46.3272007330229,46.8230931642386,47.3189855954543,47.81487802667,48.3107704578857,
48.8066628891014,49.3025553203171,49.7984477515328,50.2943401827485,50.7902326139642,
51.2861250451799,51.7820174763956,52.2779099076113,52.773802338827,53.2696947700427,
53.7655872012584,54.2614796324741,54.7573720636898,55.2532644949055,55.7491569261211,
56.2450493573368,56.7409417885525,57.2368342197682,57.7327266509839,58.2286190821996,
58.7245115134153,59.220403944631,59.7162963758467,60.2121888070624,60.7080812382781,
61.2039736694938,61.6998661007095,62.1957585319252,62.6916509631409,63.1875433943566,
63.6834358255723,64.179328256788,64.6752206880037,65.1711131192194,65.6670055504351,
66.1628979816508,66.6587904128665,67.1546828440821,67.6505752752978,68.1464677065135,
68.6423601377292,69.1382525689449,69.6341450001606,70.1300374313763),
 .UNSPECIFIED.);
#563=B_SPLINE_SURFACE_WITH_KNOTS('',3,3,((#55202,#55203,#55204,#55205,#55206,
#55207,#55208,#55209,#55210,#55211,#55212,#55213,#55214,#55215,#55216,#55217,
#55218,#55219,#55220,#55221,#55222,#55223,#55224,#55225,#55226,#55227,#55228,
#55229,#55230,#55231,#55232,#55233,#55234,#55235,#55236,#55237,#55238,#55239,
#55240,#55241,#55242,#55243,#55244,#55245,#55246,#55247,#55248,#55249,#55250,
#55251,#55252,#55253,#55254,#55255,#55256,#55257,#55258,#55259,#55260,#55261,
#55262,#55263,#55264,#55265,#55266,#55267,#55268,#55269,#55270,#55271,#55272,
#55273,#55274,#55275,#55276,#55277,#55278,#55279,#55280,#55281,#55282,#55283,
#55284,#55285,#55286,#55287,#55288,#55289,#55290,#55291,#55292,#55293,#55294,
#55295,#55296,#55297,#55298,#55299,#55300,#55301,#55302),(#55303,#55304,
#55305,#55306,#55307,#55308,#55309,#55310,#55311,#55312,#55313,#55314,#55315,
#55316,#55317,#55318,#55319,#55320,#55321,#55322,#55323,#55324,#55325,#55326,
#55327,#55328,#55329,#55330,#55331,#55332,#55333,#55334,#55335,#55336,#55337,
#55338,#55339,#55340,#55341,#55342,#55343,#55344,#55345,#55346,#55347,#55348,
#55349,#55350,#55351,#55352,#55353,#55354,#55355,#55356,#55357,#55358,#55359,
#55360,#55361,#55362,#55363,#55364,#55365,#55366,#55367,#55368,#55369,#55370,
#55371,#55372,#55373,#55374,#55375,#55376,#55377,#55378,#55379,#55380,#55381,
#55382,#55383,#55384,#55385,#55386,#55387,#55388,#55389,#55390,#55391,#55392,
#55393,#55394,#55395,#55396,#55397,#55398,#55399,#55400,#55401,#55402,#55403),
(#55404,#55405,#55406,#55407,#55408,#55409,#55410,#55411,#55412,#55413,
#55414,#55415,#55416,#55417,#55418,#55419,#55420,#55421,#55422,#55423,#55424,
#55425,#55426,#55427,#55428,#55429,#55430,#55431,#55432,#55433,#55434,#55435,
#55436,#55437,#55438,#55439,#55440,#55441,#55442,#55443,#55444,#55445,#55446,
#55447,#55448,#55449,#55450,#55451,#55452,#55453,#55454,#55455,#55456,#55457,
#55458,#55459,#55460,#55461,#55462,#55463,#55464,#55465,#55466,#55467,#55468,
#55469,#55470,#55471,#55472,#55473,#55474,#55475,#55476,#55477,#55478,#55479,
#55480,#55481,#55482,#55483,#55484,#55485,#55486,#55487,#55488,#55489,#55490,
#55491,#55492,#55493,#55494,#55495,#55496,#55497,#55498,#55499,#55500,#55501,
#55502,#55503,#55504),(#55505,#55506,#55507,#55508,#55509,#55510,#55511,
#55512,#55513,#55514,#55515,#55516,#55517,#55518,#55519,#55520,#55521,#55522,
#55523,#55524,#55525,#55526,#55527,#55528,#55529,#55530,#55531,#55532,#55533,
#55534,#55535,#55536,#55537,#55538,#55539,#55540,#55541,#55542,#55543,#55544,
#55545,#55546,#55547,#55548,#55549,#55550,#55551,#55552,#55553,#55554,#55555,
#55556,#55557,#55558,#55559,#55560,#55561,#55562,#55563,#55564,#55565,#55566,
#55567,#55568,#55569,#55570,#55571,#55572,#55573,#55574,#55575,#55576,#55577,
#55578,#55579,#55580,#55581,#55582,#55583,#55584,#55585,#55586,#55587,#55588,
#55589,#55590,#55591,#55592,#55593,#55594,#55595,#55596,#55597,#55598,#55599,
#55600,#55601,#55602,#55603,#55604,#55605),(#55606,#55607,#55608,#55609,
#55610,#55611,#55612,#55613,#55614,#55615,#55616,#55617,#55618,#55619,#55620,
#55621,#55622,#55623,#55624,#55625,#55626,#55627,#55628,#55629,#55630,#55631,
#55632,#55633,#55634,#55635,#55636,#55637,#55638,#55639,#55640,#55641,#55642,
#55643,#55644,#55645,#55646,#55647,#55648,#55649,#55650,#55651,#55652,#55653,
#55654,#55655,#55656,#55657,#55658,#55659,#55660,#55661,#55662,#55663,#55664,
#55665,#55666,#55667,#55668,#55669,#55670,#55671,#55672,#55673,#55674,#55675,
#55676,#55677,#55678,#55679,#55680,#55681,#55682,#55683,#55684,#55685,#55686,
#55687,#55688,#55689,#55690,#55691,#55692,#55693,#55694,#55695,#55696,#55697,
#55698,#55699,#55700,#55701,#55702,#55703,#55704,#55705,#55706)),
 .UNSPECIFIED.,.F.,.F.,.F.,(4,1,4),(4,1,1,1,1,1,1,1,1,1,1,1,1,1,1,1,1,1,
1,1,1,1,1,1,1,1,1,1,1,1,1,1,1,1,1,1,1,1,1,1,1,1,1,1,1,1,1,1,1,1,1,1,1,1,
1,1,1,1,1,1,1,1,1,1,1,1,1,1,1,1,1,1,1,1,1,1,1,1,1,1,1,1,1,1,1,1,1,1,1,1,
1,1,1,1,1,1,1,1,4),(0.,0.467498906784196,1.09083078249646),(6.28318530717955,
6.77358368901883,7.26398207085812,7.7543804526974,8.24477883453668,8.73517721637597,
9.22557559821525,9.71597398005454,10.2063723618938,10.6967707437331,11.1871691255724,
11.6775675074117,12.167965889251,12.6583642710902,13.1487626529295,13.6391610347688,
14.1295594166081,14.6199577984474,15.1103561802867,15.6007545621259,16.0911529439652,
16.5815513258045,17.0719497076438,17.5623480894831,18.0527464713224,18.5431448531616,
19.0335432350009,19.5239416168402,20.0143399986795,20.5047383805188,20.9951367623581,
21.4855351441973,21.9759335260366,22.4663319078759,22.9567302897152,23.4471286715545,
23.9375270533938,24.427925435233,24.9183238170723,25.4087221989116,25.8991205807509,
26.3895189625902,26.8799173444295,27.3703157262687,27.860714108108,28.3511124899473,
28.8415108717866,29.3319092536259,29.8223076354652,30.3127060173044,30.8031043991437,
31.293502780983,31.7839011628223,32.2742995446616,32.7646979265009,33.2550963083402,
33.7454946901794,34.2358930720187,34.726291453858,35.2166898356973,35.7070882175366,
36.1974865993759,36.6878849812151,37.1782833630544,37.6686817448937,38.159080126733,
38.6494785085723,39.1398768904116,39.6302752722508,40.1206736540901,40.6110720359294,
41.1014704177687,41.591868799608,42.0822671814473,42.5726655632865,43.0630639451258,
43.5534623269651,44.0438607088044,44.5342590906437,45.024657472483,45.5150558543222,
46.0054542361615,46.4958526180008,46.9862509998401,47.4766493816794,47.9670477635187,
48.457446145358,48.9478445271972,49.4382429090365,49.9286412908758,50.4190396727151,
50.9094380545544,51.3998364363937,51.8902348182329,52.3806332000722,52.8710315819115,
53.3614299637508,53.8518283455901,54.3422267274294),.UNSPECIFIED.);
#564=B_SPLINE_SURFACE_WITH_KNOTS('',3,3,((#56119,#56120,#56121,#56122,#56123,
#56124,#56125,#56126,#56127,#56128,#56129,#56130,#56131,#56132,#56133,#56134,
#56135,#56136,#56137,#56138,#56139,#56140,#56141,#56142,#56143,#56144,#56145,
#56146,#56147,#56148,#56149,#56150,#56151,#56152,#56153,#56154,#56155,#56156,
#56157,#56158,#56159,#56160,#56161,#56162,#56163,#56164,#56165,#56166,#56167,
#56168,#56169,#56170,#56171,#56172,#56173,#56174,#56175,#56176,#56177,#56178,
#56179,#56180,#56181,#56182,#56183,#56184,#56185,#56186,#56187,#56188,#56189,
#56190,#56191,#56192,#56193,#56194,#56195,#56196,#56197,#56198,#56199,#56200,
#56201,#56202,#56203,#56204,#56205,#56206,#56207,#56208,#56209,#56210,#56211,
#56212,#56213,#56214,#56215,#56216,#56217,#56218,#56219),(#56220,#56221,
#56222,#56223,#56224,#56225,#56226,#56227,#56228,#56229,#56230,#56231,#56232,
#56233,#56234,#56235,#56236,#56237,#56238,#56239,#56240,#56241,#56242,#56243,
#56244,#56245,#56246,#56247,#56248,#56249,#56250,#56251,#56252,#56253,#56254,
#56255,#56256,#56257,#56258,#56259,#56260,#56261,#56262,#56263,#56264,#56265,
#56266,#56267,#56268,#56269,#56270,#56271,#56272,#56273,#56274,#56275,#56276,
#56277,#56278,#56279,#56280,#56281,#56282,#56283,#56284,#56285,#56286,#56287,
#56288,#56289,#56290,#56291,#56292,#56293,#56294,#56295,#56296,#56297,#56298,
#56299,#56300,#56301,#56302,#56303,#56304,#56305,#56306,#56307,#56308,#56309,
#56310,#56311,#56312,#56313,#56314,#56315,#56316,#56317,#56318,#56319,#56320),
(#56321,#56322,#56323,#56324,#56325,#56326,#56327,#56328,#56329,#56330,
#56331,#56332,#56333,#56334,#56335,#56336,#56337,#56338,#56339,#56340,#56341,
#56342,#56343,#56344,#56345,#56346,#56347,#56348,#56349,#56350,#56351,#56352,
#56353,#56354,#56355,#56356,#56357,#56358,#56359,#56360,#56361,#56362,#56363,
#56364,#56365,#56366,#56367,#56368,#56369,#56370,#56371,#56372,#56373,#56374,
#56375,#56376,#56377,#56378,#56379,#56380,#56381,#56382,#56383,#56384,#56385,
#56386,#56387,#56388,#56389,#56390,#56391,#56392,#56393,#56394,#56395,#56396,
#56397,#56398,#56399,#56400,#56401,#56402,#56403,#56404,#56405,#56406,#56407,
#56408,#56409,#56410,#56411,#56412,#56413,#56414,#56415,#56416,#56417,#56418,
#56419,#56420,#56421),(#56422,#56423,#56424,#56425,#56426,#56427,#56428,
#56429,#56430,#56431,#56432,#56433,#56434,#56435,#56436,#56437,#56438,#56439,
#56440,#56441,#56442,#56443,#56444,#56445,#56446,#56447,#56448,#56449,#56450,
#56451,#56452,#56453,#56454,#56455,#56456,#56457,#56458,#56459,#56460,#56461,
#56462,#56463,#56464,#56465,#56466,#56467,#56468,#56469,#56470,#56471,#56472,
#56473,#56474,#56475,#56476,#56477,#56478,#56479,#56480,#56481,#56482,#56483,
#56484,#56485,#56486,#56487,#56488,#56489,#56490,#56491,#56492,#56493,#56494,
#56495,#56496,#56497,#56498,#56499,#56500,#56501,#56502,#56503,#56504,#56505,
#56506,#56507,#56508,#56509,#56510,#56511,#56512,#56513,#56514,#56515,#56516,
#56517,#56518,#56519,#56520,#56521,#56522)),.UNSPECIFIED.,.F.,.F.,.F.,(4,
4),(4,1,1,1,1,1,1,1,1,1,1,1,1,1,1,1,1,1,1,1,1,1,1,1,1,1,1,1,1,1,1,1,1,1,
1,1,1,1,1,1,1,1,1,1,1,1,1,1,1,1,1,1,1,1,1,1,1,1,1,1,1,1,1,1,1,1,1,1,1,1,
1,1,1,1,1,1,1,1,1,1,1,1,1,1,1,1,1,1,1,1,1,1,1,1,1,1,1,1,4),(0.,0.0671853436149873),
(7.04827039213812,7.54574010072061,8.0432098093031,8.54067951788559,9.03814922646808,
9.53561893505058,10.0330886436331,10.5305583522156,11.028028060798,11.5254977693805,
12.022967477963,12.5204371865455,13.017906895128,13.5153766037105,14.012846312293,
14.5103160208755,15.007785729458,15.5052554380405,16.002725146623,16.5001948552054,
16.9976645637879,17.4951342723704,17.9926039809529,18.4900736895354,18.9875433981179,
19.4850131067004,19.9824828152829,20.4799525238654,20.9774222324479,21.4748919410303,
21.9723616496128,22.4698313581953,22.9673010667778,23.4647707753603,23.9622404839428,
24.4597101925253,24.9571799011078,25.4546496096903,25.9521193182728,26.4495890268552,
26.9470587354377,27.4445284440202,27.9419981526027,28.4394678611852,28.9369375697677,
29.4344072783502,29.9318769869327,30.4293466955152,30.9268164040977,31.4242861126801,
31.9217558212626,32.4192255298451,32.9166952384276,33.4141649470101,33.9116346555926,
34.4091043641751,34.9065740727576,35.4040437813401,35.9015134899226,36.3989831985051,
36.8964529070875,37.39392261567,37.8913923242525,38.388862032835,38.8863317414175,
39.38380145,39.8812711585825,40.378740867165,40.8762105757475,41.37368028433,
41.8711499929124,42.3686197014949,42.8660894100774,43.3635591186599,43.8610288272424,
44.3584985358249,44.8559682444074,45.3534379529899,45.8509076615724,46.3483773701549,
46.8458470787373,47.3433167873198,47.8407864959023,48.3382562044848,48.8357259130673,
49.3331956216498,49.8306653302323,50.3281350388148,50.8256047473973,51.3230744559798,
51.8205441645622,52.3180138731447,52.8154835817272,53.3129532903097,53.8104229988922,
54.3078927074747,54.8053624160572,55.3028321246397,55.8003018332222),
 .UNSPECIFIED.);
#565=B_SPLINE_SURFACE_WITH_KNOTS('',3,3,((#56725,#56726,#56727,#56728,#56729,
#56730,#56731,#56732,#56733,#56734,#56735,#56736,#56737,#56738,#56739,#56740,
#56741,#56742,#56743,#56744,#56745,#56746,#56747,#56748,#56749,#56750,#56751,
#56752,#56753,#56754,#56755,#56756,#56757,#56758,#56759,#56760,#56761,#56762,
#56763,#56764,#56765,#56766,#56767,#56768,#56769,#56770,#56771,#56772,#56773,
#56774,#56775,#56776,#56777,#56778,#56779,#56780,#56781,#56782,#56783,#56784,
#56785,#56786,#56787,#56788,#56789,#56790,#56791,#56792,#56793,#56794,#56795,
#56796,#56797,#56798,#56799,#56800,#56801,#56802,#56803,#56804,#56805,#56806,
#56807,#56808,#56809,#56810,#56811,#56812,#56813,#56814,#56815,#56816,#56817,
#56818,#56819,#56820,#56821,#56822,#56823,#56824,#56825),(#56826,#56827,
#56828,#56829,#56830,#56831,#56832,#56833,#56834,#56835,#56836,#56837,#56838,
#56839,#56840,#56841,#56842,#56843,#56844,#56845,#56846,#56847,#56848,#56849,
#56850,#56851,#56852,#56853,#56854,#56855,#56856,#56857,#56858,#56859,#56860,
#56861,#56862,#56863,#56864,#56865,#56866,#56867,#56868,#56869,#56870,#56871,
#56872,#56873,#56874,#56875,#56876,#56877,#56878,#56879,#56880,#56881,#56882,
#56883,#56884,#56885,#56886,#56887,#56888,#56889,#56890,#56891,#56892,#56893,
#56894,#56895,#56896,#56897,#56898,#56899,#56900,#56901,#56902,#56903,#56904,
#56905,#56906,#56907,#56908,#56909,#56910,#56911,#56912,#56913,#56914,#56915,
#56916,#56917,#56918,#56919,#56920,#56921,#56922,#56923,#56924,#56925,#56926),
(#56927,#56928,#56929,#56930,#56931,#56932,#56933,#56934,#56935,#56936,
#56937,#56938,#56939,#56940,#56941,#56942,#56943,#56944,#56945,#56946,#56947,
#56948,#56949,#56950,#56951,#56952,#56953,#56954,#56955,#56956,#56957,#56958,
#56959,#56960,#56961,#56962,#56963,#56964,#56965,#56966,#56967,#56968,#56969,
#56970,#56971,#56972,#56973,#56974,#56975,#56976,#56977,#56978,#56979,#56980,
#56981,#56982,#56983,#56984,#56985,#56986,#56987,#56988,#56989,#56990,#56991,
#56992,#56993,#56994,#56995,#56996,#56997,#56998,#56999,#57000,#57001,#57002,
#57003,#57004,#57005,#57006,#57007,#57008,#57009,#57010,#57011,#57012,#57013,
#57014,#57015,#57016,#57017,#57018,#57019,#57020,#57021,#57022,#57023,#57024,
#57025,#57026,#57027),(#57028,#57029,#57030,#57031,#57032,#57033,#57034,
#57035,#57036,#57037,#57038,#57039,#57040,#57041,#57042,#57043,#57044,#57045,
#57046,#57047,#57048,#57049,#57050,#57051,#57052,#57053,#57054,#57055,#57056,
#57057,#57058,#57059,#57060,#57061,#57062,#57063,#57064,#57065,#57066,#57067,
#57068,#57069,#57070,#57071,#57072,#57073,#57074,#57075,#57076,#57077,#57078,
#57079,#57080,#57081,#57082,#57083,#57084,#57085,#57086,#57087,#57088,#57089,
#57090,#57091,#57092,#57093,#57094,#57095,#57096,#57097,#57098,#57099,#57100,
#57101,#57102,#57103,#57104,#57105,#57106,#57107,#57108,#57109,#57110,#57111,
#57112,#57113,#57114,#57115,#57116,#57117,#57118,#57119,#57120,#57121,#57122,
#57123,#57124,#57125,#57126,#57127,#57128),(#57129,#57130,#57131,#57132,
#57133,#57134,#57135,#57136,#57137,#57138,#57139,#57140,#57141,#57142,#57143,
#57144,#57145,#57146,#57147,#57148,#57149,#57150,#57151,#57152,#57153,#57154,
#57155,#57156,#57157,#57158,#57159,#57160,#57161,#57162,#57163,#57164,#57165,
#57166,#57167,#57168,#57169,#57170,#57171,#57172,#57173,#57174,#57175,#57176,
#57177,#57178,#57179,#57180,#57181,#57182,#57183,#57184,#57185,#57186,#57187,
#57188,#57189,#57190,#57191,#57192,#57193,#57194,#57195,#57196,#57197,#57198,
#57199,#57200,#57201,#57202,#57203,#57204,#57205,#57206,#57207,#57208,#57209,
#57210,#57211,#57212,#57213,#57214,#57215,#57216,#57217,#57218,#57219,#57220,
#57221,#57222,#57223,#57224,#57225,#57226,#57227,#57228,#57229)),
 .UNSPECIFIED.,.F.,.F.,.F.,(4,1,4),(4,1,1,1,1,1,1,1,1,1,1,1,1,1,1,1,1,1,
1,1,1,1,1,1,1,1,1,1,1,1,1,1,1,1,1,1,1,1,1,1,1,1,1,1,1,1,1,1,1,1,1,1,1,1,
1,1,1,1,1,1,1,1,1,1,1,1,1,1,1,1,1,1,1,1,1,1,1,1,1,1,1,1,1,1,1,1,1,1,1,1,
1,1,1,1,1,1,1,1,4),(0.,0.467498906784196,1.09083078249646),(8.50634549793093,
8.99674387977021,9.4871422616095,9.97754064344878,10.4679390252881,10.9583374071273,
11.4487357889666,11.9391341708059,12.4295325526452,12.9199309344845,13.4103293163238,
13.9007276981631,14.3911260800023,14.8815244618416,15.3719228436809,15.8623212255202,
16.3527196073595,16.8431179891988,17.333516371038,17.8239147528773,18.3143131347166,
18.8047115165559,19.2951098983952,19.7855082802345,20.2759066620737,20.766305043913,
21.2567034257523,21.7471018075916,22.2375001894309,22.7278985712702,23.2182969531094,
23.7086953349487,24.199093716788,24.6894920986273,25.1798904804666,25.6702888623059,
26.1606872441451,26.6510856259844,27.1414840078237,27.631882389663,28.1222807715023,
28.6126791533416,29.1030775351808,29.5934759170201,30.0838742988594,30.5742726806987,
31.064671062538,31.5550694443773,32.0454678262166,32.5358662080558,33.0262645898951,
33.5166629717344,34.0070613535737,34.497459735413,34.9878581172523,35.4782564990915,
35.9686548809308,36.4590532627701,36.9494516446094,37.4398500264487,37.930248408288,
38.4206467901272,38.9110451719665,39.4014435538058,39.8918419356451,40.3822403174844,
40.8726386993237,41.3630370811629,41.8534354630022,42.3438338448415,42.8342322266808,
43.3246306085201,43.8150289903594,44.3054273721986,44.7958257540379,45.2862241358772,
45.7766225177165,46.2670208995558,46.7574192813951,47.2478176632343,47.7382160450736,
48.2286144269129,48.7190128087522,49.2094111905915,49.6998095724308,50.1902079542701,
50.6806063361093,51.1710047179486,51.6614030997879,52.1518014816272,52.6421998634665,
53.1325982453058,53.622996627145,54.1133950089843,54.6037933908236,55.0941917726629,
55.5845901545022,56.0749885363415,56.5653869181807),.UNSPECIFIED.);
#566=B_SPLINE_SURFACE_WITH_KNOTS('',3,3,((#57322,#57323,#57324,#57325,#57326,
#57327,#57328,#57329,#57330,#57331,#57332,#57333,#57334,#57335,#57336,#57337,
#57338,#57339,#57340,#57341,#57342,#57343,#57344,#57345,#57346,#57347,#57348,
#57349,#57350,#57351,#57352,#57353,#57354,#57355,#57356,#57357,#57358,#57359,
#57360,#57361,#57362,#57363,#57364,#57365,#57366,#57367,#57368,#57369,#57370,
#57371,#57372,#57373,#57374,#57375,#57376,#57377,#57378,#57379,#57380,#57381,
#57382,#57383,#57384,#57385,#57386,#57387,#57388,#57389,#57390,#57391,#57392,
#57393,#57394,#57395,#57396,#57397,#57398,#57399,#57400,#57401,#57402,#57403,
#57404,#57405,#57406,#57407,#57408,#57409,#57410,#57411,#57412,#57413,#57414,
#57415,#57416,#57417,#57418,#57419,#57420,#57421,#57422),(#57423,#57424,
#57425,#57426,#57427,#57428,#57429,#57430,#57431,#57432,#57433,#57434,#57435,
#57436,#57437,#57438,#57439,#57440,#57441,#57442,#57443,#57444,#57445,#57446,
#57447,#57448,#57449,#57450,#57451,#57452,#57453,#57454,#57455,#57456,#57457,
#57458,#57459,#57460,#57461,#57462,#57463,#57464,#57465,#57466,#57467,#57468,
#57469,#57470,#57471,#57472,#57473,#57474,#57475,#57476,#57477,#57478,#57479,
#57480,#57481,#57482,#57483,#57484,#57485,#57486,#57487,#57488,#57489,#57490,
#57491,#57492,#57493,#57494,#57495,#57496,#57497,#57498,#57499,#57500,#57501,
#57502,#57503,#57504,#57505,#57506,#57507,#57508,#57509,#57510,#57511,#57512,
#57513,#57514,#57515,#57516,#57517,#57518,#57519,#57520,#57521,#57522,#57523),
(#57524,#57525,#57526,#57527,#57528,#57529,#57530,#57531,#57532,#57533,
#57534,#57535,#57536,#57537,#57538,#57539,#57540,#57541,#57542,#57543,#57544,
#57545,#57546,#57547,#57548,#57549,#57550,#57551,#57552,#57553,#57554,#57555,
#57556,#57557,#57558,#57559,#57560,#57561,#57562,#57563,#57564,#57565,#57566,
#57567,#57568,#57569,#57570,#57571,#57572,#57573,#57574,#57575,#57576,#57577,
#57578,#57579,#57580,#57581,#57582,#57583,#57584,#57585,#57586,#57587,#57588,
#57589,#57590,#57591,#57592,#57593,#57594,#57595,#57596,#57597,#57598,#57599,
#57600,#57601,#57602,#57603,#57604,#57605,#57606,#57607,#57608,#57609,#57610,
#57611,#57612,#57613,#57614,#57615,#57616,#57617,#57618,#57619,#57620,#57621,
#57622,#57623,#57624),(#57625,#57626,#57627,#57628,#57629,#57630,#57631,
#57632,#57633,#57634,#57635,#57636,#57637,#57638,#57639,#57640,#57641,#57642,
#57643,#57644,#57645,#57646,#57647,#57648,#57649,#57650,#57651,#57652,#57653,
#57654,#57655,#57656,#57657,#57658,#57659,#57660,#57661,#57662,#57663,#57664,
#57665,#57666,#57667,#57668,#57669,#57670,#57671,#57672,#57673,#57674,#57675,
#57676,#57677,#57678,#57679,#57680,#57681,#57682,#57683,#57684,#57685,#57686,
#57687,#57688,#57689,#57690,#57691,#57692,#57693,#57694,#57695,#57696,#57697,
#57698,#57699,#57700,#57701,#57702,#57703,#57704,#57705,#57706,#57707,#57708,
#57709,#57710,#57711,#57712,#57713,#57714,#57715,#57716,#57717,#57718,#57719,
#57720,#57721,#57722,#57723,#57724,#57725),(#57726,#57727,#57728,#57729,
#57730,#57731,#57732,#57733,#57734,#57735,#57736,#57737,#57738,#57739,#57740,
#57741,#57742,#57743,#57744,#57745,#57746,#57747,#57748,#57749,#57750,#57751,
#57752,#57753,#57754,#57755,#57756,#57757,#57758,#57759,#57760,#57761,#57762,
#57763,#57764,#57765,#57766,#57767,#57768,#57769,#57770,#57771,#57772,#57773,
#57774,#57775,#57776,#57777,#57778,#57779,#57780,#57781,#57782,#57783,#57784,
#57785,#57786,#57787,#57788,#57789,#57790,#57791,#57792,#57793,#57794,#57795,
#57796,#57797,#57798,#57799,#57800,#57801,#57802,#57803,#57804,#57805,#57806,
#57807,#57808,#57809,#57810,#57811,#57812,#57813,#57814,#57815,#57816,#57817,
#57818,#57819,#57820,#57821,#57822,#57823,#57824,#57825,#57826)),
 .UNSPECIFIED.,.F.,.F.,.F.,(4,1,4),(4,1,1,1,1,1,1,1,1,1,1,1,1,1,1,1,1,1,
1,1,1,1,1,1,1,1,1,1,1,1,1,1,1,1,1,1,1,1,1,1,1,1,1,1,1,1,1,1,1,1,1,1,1,1,
1,1,1,1,1,1,1,1,1,1,1,1,1,1,1,1,1,1,1,1,1,1,1,1,1,1,1,1,1,1,1,1,1,1,1,1,
1,1,1,1,1,1,1,1,4),(-1.09083078249646,-0.623331875712262,0.),(9.57812533864917,
10.0685237204885,10.5589221023277,11.049320484167,11.5397188660063,12.0301172478456,
12.5205156296849,13.0109140115242,13.5013123933634,13.9917107752027,14.482109157042,
14.9725075388813,15.4629059207206,15.9533043025599,16.4437026843991,16.9341010662384,
17.4244994480777,17.914897829917,18.4052962117563,18.8956945935956,19.3860929754348,
19.8764913572741,20.3668897391134,20.8572881209527,21.347686502792,21.8380848846313,
22.3284832664706,22.8188816483098,23.3092800301491,23.7996784119884,24.2900767938277,
24.780475175667,25.2708735575063,25.7612719393455,26.2516703211848,26.7420687030241,
27.2324670848634,27.7228654667027,28.213263848542,28.7036622303812,29.1940606122205,
29.6844589940598,30.1748573758991,30.6652557577384,31.1556541395777,31.6460525214169,
32.1364509032562,32.6268492850955,33.1172476669348,33.6076460487741,34.0980444306134,
34.5884428124527,35.0788411942919,35.5692395761312,36.0596379579705,36.5500363398098,
37.0404347216491,37.5308331034883,38.0212314853276,38.5116298671669,39.0020282490062,
39.4924266308455,39.9828250126848,40.4732233945241,40.9636217763633,41.4540201582026,
41.9444185400419,42.4348169218812,42.9252153037205,43.4156136855598,43.906012067399,
44.3964104492383,44.8868088310776,45.3772072129169,45.8676055947562,46.3580039765955,
46.8484023584347,47.338800740274,47.8291991221133,48.3195975039526,48.8099958857919,
49.3003942676312,49.7907926494704,50.2811910313097,50.771589413149,51.2619877949883,
51.7523861768276,52.2427845586669,52.7331829405062,53.2235813223454,53.7139797041847,
54.204378086024,54.6947764678633,55.1851748497026,55.6755732315419,56.1659716133811,
56.6563699952204,57.1467683770597,57.637166758899),.UNSPECIFIED.);
#567=B_SPLINE_SURFACE_WITH_KNOTS('',3,3,((#57934,#57935,#57936,#57937,#57938,
#57939,#57940,#57941,#57942,#57943,#57944,#57945,#57946,#57947,#57948,#57949,
#57950,#57951,#57952,#57953,#57954,#57955,#57956,#57957,#57958,#57959,#57960,
#57961,#57962,#57963,#57964,#57965,#57966,#57967,#57968,#57969,#57970,#57971,
#57972,#57973,#57974,#57975,#57976,#57977,#57978,#57979,#57980,#57981,#57982,
#57983,#57984,#57985,#57986,#57987,#57988,#57989,#57990,#57991,#57992,#57993,
#57994,#57995,#57996,#57997,#57998,#57999,#58000,#58001,#58002,#58003,#58004,
#58005,#58006,#58007,#58008,#58009,#58010,#58011,#58012,#58013,#58014,#58015,
#58016,#58017,#58018,#58019,#58020,#58021,#58022,#58023,#58024,#58025,#58026,
#58027,#58028,#58029,#58030,#58031,#58032,#58033,#58034),(#58035,#58036,
#58037,#58038,#58039,#58040,#58041,#58042,#58043,#58044,#58045,#58046,#58047,
#58048,#58049,#58050,#58051,#58052,#58053,#58054,#58055,#58056,#58057,#58058,
#58059,#58060,#58061,#58062,#58063,#58064,#58065,#58066,#58067,#58068,#58069,
#58070,#58071,#58072,#58073,#58074,#58075,#58076,#58077,#58078,#58079,#58080,
#58081,#58082,#58083,#58084,#58085,#58086,#58087,#58088,#58089,#58090,#58091,
#58092,#58093,#58094,#58095,#58096,#58097,#58098,#58099,#58100,#58101,#58102,
#58103,#58104,#58105,#58106,#58107,#58108,#58109,#58110,#58111,#58112,#58113,
#58114,#58115,#58116,#58117,#58118,#58119,#58120,#58121,#58122,#58123,#58124,
#58125,#58126,#58127,#58128,#58129,#58130,#58131,#58132,#58133,#58134,#58135),
(#58136,#58137,#58138,#58139,#58140,#58141,#58142,#58143,#58144,#58145,
#58146,#58147,#58148,#58149,#58150,#58151,#58152,#58153,#58154,#58155,#58156,
#58157,#58158,#58159,#58160,#58161,#58162,#58163,#58164,#58165,#58166,#58167,
#58168,#58169,#58170,#58171,#58172,#58173,#58174,#58175,#58176,#58177,#58178,
#58179,#58180,#58181,#58182,#58183,#58184,#58185,#58186,#58187,#58188,#58189,
#58190,#58191,#58192,#58193,#58194,#58195,#58196,#58197,#58198,#58199,#58200,
#58201,#58202,#58203,#58204,#58205,#58206,#58207,#58208,#58209,#58210,#58211,
#58212,#58213,#58214,#58215,#58216,#58217,#58218,#58219,#58220,#58221,#58222,
#58223,#58224,#58225,#58226,#58227,#58228,#58229,#58230,#58231,#58232,#58233,
#58234,#58235,#58236),(#58237,#58238,#58239,#58240,#58241,#58242,#58243,
#58244,#58245,#58246,#58247,#58248,#58249,#58250,#58251,#58252,#58253,#58254,
#58255,#58256,#58257,#58258,#58259,#58260,#58261,#58262,#58263,#58264,#58265,
#58266,#58267,#58268,#58269,#58270,#58271,#58272,#58273,#58274,#58275,#58276,
#58277,#58278,#58279,#58280,#58281,#58282,#58283,#58284,#58285,#58286,#58287,
#58288,#58289,#58290,#58291,#58292,#58293,#58294,#58295,#58296,#58297,#58298,
#58299,#58300,#58301,#58302,#58303,#58304,#58305,#58306,#58307,#58308,#58309,
#58310,#58311,#58312,#58313,#58314,#58315,#58316,#58317,#58318,#58319,#58320,
#58321,#58322,#58323,#58324,#58325,#58326,#58327,#58328,#58329,#58330,#58331,
#58332,#58333,#58334,#58335,#58336,#58337)),.UNSPECIFIED.,.F.,.F.,.F.,(4,
4),(4,1,1,1,1,1,1,1,1,1,1,1,1,1,1,1,1,1,1,1,1,1,1,1,1,1,1,1,1,1,1,1,1,1,
1,1,1,1,1,1,1,1,1,1,1,1,1,1,1,1,1,1,1,1,1,1,1,1,1,1,1,1,1,1,1,1,1,1,1,1,
1,1,1,1,1,1,1,1,1,1,1,1,1,1,1,1,1,1,1,1,1,1,1,1,1,1,1,1,4),(0.,0.0671853436149873),
(10.3432104236078,10.8406801321902,11.3381498407727,11.8356195493552,12.3330892579377,
12.8305589665202,13.3280286751027,13.8254983836852,14.3229680922677,14.8204378008502,
15.3179075094327,15.8153772180151,16.3128469265976,16.8103166351801,17.3077863437626,
17.8052560523451,18.3027257609276,18.8001954695101,19.2976651780926,19.7951348866751,
20.2926045952576,20.79007430384,21.2875440124225,21.785013721005,22.2824834295875,
22.77995313817,23.2774228467525,23.774892555335,24.2723622639175,24.7698319725,
25.2673016810825,25.7647713896649,26.2622410982474,26.7597108068299,27.2571805154124,
27.7546502239949,28.2521199325774,28.7495896411599,29.2470593497424,29.7445290583249,
30.2419987669074,30.7394684754899,31.2369381840723,31.7344078926548,32.2318776012373,
32.7293473098198,33.2268170184023,33.7242867269848,34.2217564355673,34.7192261441498,
35.2166958527323,35.7141655613148,36.2116352698972,36.7091049784797,37.2065746870622,
37.7040443956447,38.2015141042272,38.6989838128097,39.1964535213922,39.6939232299747,
40.1913929385572,40.6888626471397,41.1863323557221,41.6838020643046,42.1812717728871,
42.6787414814696,43.1762111900521,43.6736808986346,44.1711506072171,44.6686203157996,
45.1660900243821,45.6635597329646,46.1610294415471,46.6584991501295,47.155968858712,
47.6534385672945,48.150908275877,48.6483779844595,49.145847693042,49.6433174016245,
50.140787110207,50.6382568187895,51.135726527372,51.6331962359544,52.1306659445369,
52.6281356531194,53.1256053617019,53.6230750702844,54.1205447788669,54.6180144874494,
55.1154841960319,55.6129539046144,56.1104236131969,56.6078933217793,57.1053630303618,
57.6028327389443,58.1003024475268,58.5977721561093,59.0952418646918),
 .UNSPECIFIED.);
#568=B_SPLINE_SURFACE_WITH_KNOTS('',3,3,((#58490,#58491,#58492,#58493,#58494,
#58495,#58496,#58497,#58498,#58499,#58500,#58501,#58502,#58503,#58504,#58505,
#58506,#58507,#58508,#58509,#58510,#58511,#58512,#58513,#58514,#58515,#58516,
#58517,#58518,#58519,#58520,#58521,#58522,#58523,#58524,#58525,#58526,#58527,
#58528,#58529,#58530,#58531,#58532,#58533,#58534,#58535,#58536,#58537,#58538,
#58539,#58540,#58541,#58542,#58543,#58544,#58545,#58546,#58547,#58548,#58549,
#58550,#58551,#58552,#58553,#58554,#58555,#58556,#58557,#58558,#58559,#58560,
#58561,#58562,#58563,#58564,#58565,#58566,#58567,#58568,#58569,#58570,#58571,
#58572,#58573,#58574,#58575,#58576,#58577,#58578,#58579,#58580,#58581,#58582,
#58583,#58584,#58585,#58586,#58587,#58588,#58589,#58590),(#58591,#58592,
#58593,#58594,#58595,#58596,#58597,#58598,#58599,#58600,#58601,#58602,#58603,
#58604,#58605,#58606,#58607,#58608,#58609,#58610,#58611,#58612,#58613,#58614,
#58615,#58616,#58617,#58618,#58619,#58620,#58621,#58622,#58623,#58624,#58625,
#58626,#58627,#58628,#58629,#58630,#58631,#58632,#58633,#58634,#58635,#58636,
#58637,#58638,#58639,#58640,#58641,#58642,#58643,#58644,#58645,#58646,#58647,
#58648,#58649,#58650,#58651,#58652,#58653,#58654,#58655,#58656,#58657,#58658,
#58659,#58660,#58661,#58662,#58663,#58664,#58665,#58666,#58667,#58668,#58669,
#58670,#58671,#58672,#58673,#58674,#58675,#58676,#58677,#58678,#58679,#58680,
#58681,#58682,#58683,#58684,#58685,#58686,#58687,#58688,#58689,#58690,#58691),
(#58692,#58693,#58694,#58695,#58696,#58697,#58698,#58699,#58700,#58701,
#58702,#58703,#58704,#58705,#58706,#58707,#58708,#58709,#58710,#58711,#58712,
#58713,#58714,#58715,#58716,#58717,#58718,#58719,#58720,#58721,#58722,#58723,
#58724,#58725,#58726,#58727,#58728,#58729,#58730,#58731,#58732,#58733,#58734,
#58735,#58736,#58737,#58738,#58739,#58740,#58741,#58742,#58743,#58744,#58745,
#58746,#58747,#58748,#58749,#58750,#58751,#58752,#58753,#58754,#58755,#58756,
#58757,#58758,#58759,#58760,#58761,#58762,#58763,#58764,#58765,#58766,#58767,
#58768,#58769,#58770,#58771,#58772,#58773,#58774,#58775,#58776,#58777,#58778,
#58779,#58780,#58781,#58782,#58783,#58784,#58785,#58786,#58787,#58788,#58789,
#58790,#58791,#58792),(#58793,#58794,#58795,#58796,#58797,#58798,#58799,
#58800,#58801,#58802,#58803,#58804,#58805,#58806,#58807,#58808,#58809,#58810,
#58811,#58812,#58813,#58814,#58815,#58816,#58817,#58818,#58819,#58820,#58821,
#58822,#58823,#58824,#58825,#58826,#58827,#58828,#58829,#58830,#58831,#58832,
#58833,#58834,#58835,#58836,#58837,#58838,#58839,#58840,#58841,#58842,#58843,
#58844,#58845,#58846,#58847,#58848,#58849,#58850,#58851,#58852,#58853,#58854,
#58855,#58856,#58857,#58858,#58859,#58860,#58861,#58862,#58863,#58864,#58865,
#58866,#58867,#58868,#58869,#58870,#58871,#58872,#58873,#58874,#58875,#58876,
#58877,#58878,#58879,#58880,#58881,#58882,#58883,#58884,#58885,#58886,#58887,
#58888,#58889,#58890,#58891,#58892,#58893),(#58894,#58895,#58896,#58897,
#58898,#58899,#58900,#58901,#58902,#58903,#58904,#58905,#58906,#58907,#58908,
#58909,#58910,#58911,#58912,#58913,#58914,#58915,#58916,#58917,#58918,#58919,
#58920,#58921,#58922,#58923,#58924,#58925,#58926,#58927,#58928,#58929,#58930,
#58931,#58932,#58933,#58934,#58935,#58936,#58937,#58938,#58939,#58940,#58941,
#58942,#58943,#58944,#58945,#58946,#58947,#58948,#58949,#58950,#58951,#58952,
#58953,#58954,#58955,#58956,#58957,#58958,#58959,#58960,#58961,#58962,#58963,
#58964,#58965,#58966,#58967,#58968,#58969,#58970,#58971,#58972,#58973,#58974,
#58975,#58976,#58977,#58978,#58979,#58980,#58981,#58982,#58983,#58984,#58985,
#58986,#58987,#58988,#58989,#58990,#58991,#58992,#58993,#58994)),
 .UNSPECIFIED.,.F.,.F.,.F.,(4,1,4),(4,1,1,1,1,1,1,1,1,1,1,1,1,1,1,1,1,1,
1,1,1,1,1,1,1,1,1,1,1,1,1,1,1,1,1,1,1,1,1,1,1,1,1,1,1,1,1,1,1,1,1,1,1,1,
1,1,1,1,1,1,1,1,1,1,1,1,1,1,1,1,1,1,1,1,1,1,1,1,1,1,1,1,1,1,1,1,1,1,1,1,
1,1,1,1,1,1,1,1,4),(-1.09083078249646,-0.623331875712262,0.),(11.8012855294006,
12.2916839112398,12.7820822930791,13.2724806749184,13.7628790567577,14.253277438597,
14.7436758204363,15.2340742022755,15.7244725841148,16.2148709659541,16.7052693477934,
17.1956677296327,17.686066111472,18.1764644933112,18.6668628751505,19.1572612569898,
19.6476596388291,20.1380580206684,20.6284564025077,21.118854784347,21.6092531661862,
22.0996515480255,22.5900499298648,23.0804483117041,23.5708466935434,24.0612450753827,
24.5516434572219,25.0420418390612,25.5324402209005,26.0228386027398,26.5132369845791,
27.0036353664184,27.4940337482576,27.9844321300969,28.4748305119362,28.9652288937755,
29.4556272756148,29.9460256574541,30.4364240392933,30.9268224211326,31.4172208029719,
31.9076191848112,32.3980175666505,32.8884159484898,33.378814330329,33.8692127121683,
34.3596110940076,34.8500094758469,35.3404078576862,35.8308062395255,36.3212046213647,
36.811603003204,37.3020013850433,37.7923997668826,38.2827981487219,38.7731965305612,
39.2635949124004,39.7539932942397,40.244391676079,40.7347900579183,41.2251884397576,
41.7155868215969,42.2059852034361,42.6963835852754,43.1867819671147,43.677180348954,
44.1675787307933,44.6579771126326,45.1483754944719,45.6387738763111,46.1291722581504,
46.6195706399897,47.109969021829,47.6003674036683,48.0907657855076,48.5811641673468,
49.0715625491861,49.5619609310254,50.0523593128647,50.542757694704,51.0331560765433,
51.5235544583825,52.0139528402218,52.5043512220611,52.9947496039004,53.4851479857397,
53.975546367579,54.4659447494182,54.9563431312575,55.4467415130968,55.9371398949361,
56.4275382767754,56.9179366586147,57.4083350404539,57.8987334222932,58.3891318041325,
58.8795301859718,59.3699285678111,59.8603269496504),.UNSPECIFIED.);
#569=B_SPLINE_CURVE_WITH_KNOTS('',3,(#30893,#30894,#30895,#30896,#30897,
#30898),.UNSPECIFIED.,.F.,.F.,(4,2,4),(-0.0953956468456381,-0.0476986988383283,
0.),.UNSPECIFIED.);
#570=B_SPLINE_CURVE_WITH_KNOTS('',3,(#30921,#30922,#30923,#30924,#30925,
#30926),.UNSPECIFIED.,.F.,.F.,(4,2,4),(-0.0953955489316151,-0.0476968906569989,
0.),.UNSPECIFIED.);
#571=B_SPLINE_CURVE_WITH_KNOTS('',3,(#30982,#30983,#30984,#30985,#30986,
#30987,#30988,#30989,#30990,#30991),.UNSPECIFIED.,.F.,.F.,(4,1,1,1,1,1,
1,4),(0.0848980286013396,0.519992957590172,0.956926240256775,1.39385952292338,
1.83079280558998,2.26772608825659,2.70465937092319,3.14159265358979),
 .UNSPECIFIED.);
#572=B_SPLINE_CURVE_WITH_KNOTS('',3,(#30994,#30995,#30996,#30997,#30998,
#30999,#31000,#31001,#31002,#31003),.UNSPECIFIED.,.F.,.F.,(4,1,1,1,1,1,
1,4),(-3.14159265358979,-2.70465937092319,-2.26772608825659,-1.83079280558998,
-1.39385952292338,-0.956926240256775,-0.519992957590172,-0.0830596749235681),
 .UNSPECIFIED.);
#573=B_SPLINE_CURVE_WITH_KNOTS('',3,(#31012,#31013,#31014,#31015,#31016,
#31017,#31018,#31019,#31020,#31021,#31022,#31023,#31024,#31025,#31026,#31027,
#31028),.UNSPECIFIED.,.T.,.F.,(4,1,1,1,1,1,1,1,1,1,1,1,1,1,4),(-3.14159265358979,
-2.69279370307697,-2.24399475256414,-1.64559615188037,-1.34639685153848,
-0.747998250854713,-0.448798950512828,0.149599650170943,0.448798950512828,
1.0471975511966,1.34639685153848,1.79519580205131,2.24399475256414,2.69279370307697,
3.14159265358979),.UNSPECIFIED.);
#574=B_SPLINE_CURVE_WITH_KNOTS('',3,(#31070,#31071,#31072,#31073,#31074,
#31075,#31076,#31077,#31078,#31079),.UNSPECIFIED.,.F.,.F.,(4,1,1,1,1,1,
1,4),(0.083059674921698,0.519992957588569,0.95692624025544,1.39385952292231,
1.83079280558918,2.26772608825605,2.70465937092292,3.14159265358979),
 .UNSPECIFIED.);
#575=B_SPLINE_CURVE_WITH_KNOTS('',3,(#31080,#31081,#31082,#31083,#31084,
#31085,#31086,#31087,#31088,#31089),.UNSPECIFIED.,.F.,.F.,(4,1,1,1,1,1,
1,4),(-3.14159265358979,-2.70465937092292,-2.26772608825605,-1.83079280558918,
-1.39385952292231,-0.95692624025544,-0.519992957588569,-0.0848980305822978),
 .UNSPECIFIED.);
#576=B_SPLINE_CURVE_WITH_KNOTS('',3,(#31092,#31093,#31094,#31095,#31096,
#31097,#31098,#31099,#31100,#31101,#31102,#31103,#31104,#31105,#31106,#31107,
#31108),.UNSPECIFIED.,.T.,.F.,(4,1,1,1,1,1,1,1,1,1,1,1,1,1,4),(-3.14159265358979,
-2.69279370307697,-2.24399475256414,-1.79519580205131,-1.34639685153848,
-1.0471975511966,-0.448798950512828,-0.149599650170943,0.448798950512828,
0.747998250854713,1.34639685153848,1.64559615188037,2.24399475256414,2.69279370307697,
3.14159265358979),.UNSPECIFIED.);
#577=B_SPLINE_CURVE_WITH_KNOTS('',3,(#31189,#31190,#31191,#31192,#31193,
#31194,#31195,#31196,#31197,#31198,#31199,#31200,#31201,#31202,#31203,#31204,
#31205,#31206,#31207,#31208,#31209,#31210,#31211,#31212,#31213,#31214,#31215,
#31216,#31217,#31218,#31219,#31220,#31221,#31222,#31223,#31224),
 .UNSPECIFIED.,.F.,.F.,(4,2,2,2,2,2,2,2,2,2,2,2,2,2,2,2,2,4),(-8.09601808660967,
-6.95211114501378,-5.94311837811659,-4.55541281139976,-3.41582959923829,
-3.01501785802626,-2.8942748329529,-2.84936482218812,-2.82500498483727,
-2.8058948573567,-2.78504274409744,-2.75364696269285,-2.68586477663438,
-2.5294569358349,-2.14040235758073,-1.34382220888079,-0.648089834050052,
0.),.UNSPECIFIED.);
#578=B_SPLINE_CURVE_WITH_KNOTS('',3,(#31233,#31234,#31235,#31236,#31237,
#31238,#31239,#31240,#31241,#31242,#31243,#31244,#31245,#31246,#31247,#31248),
 .UNSPECIFIED.,.F.,.F.,(4,2,2,2,2,2,2,4),(-8.25962359305892,-7.06880639418565,
-6.02569177482105,-4.59002353937466,-3.42632229394732,-3.02472929447217,
-2.902401118056,-2.8848490611025),.UNSPECIFIED.);
#579=B_SPLINE_CURVE_WITH_KNOTS('',3,(#31251,#31252,#31253,#31254,#31255,
#31256,#31257,#31258,#31259,#31260,#31261,#31262,#31263,#31264,#31265,#31266,
#31267,#31268,#31269,#31270,#31271,#31272),.UNSPECIFIED.,.F.,.F.,(4,2,2,
2,2,2,2,2,2,2,4),(-2.8848490611025,-2.85598304066293,-2.83035400420251,
-2.80984607017121,-2.78716062094501,-2.75249343197851,-2.66253946470509,
-2.14039903787906,-1.34382126836984,-0.648090922770533,0.),
 .UNSPECIFIED.);
#580=B_SPLINE_CURVE_WITH_KNOTS('',3,(#32105,#32106,#32107,#32108,#32109,
#32110,#32111,#32112,#32113,#32114,#32115,#32116,#32117,#32118,#32119,#32120,
#32121,#32122,#32123,#32124,#32125,#32126,#32127,#32128,#32129,#32130,#32131,
#32132,#32133,#32134,#32135,#32136,#32137,#32138,#32139,#32140,#32141,#32142,
#32143,#32144,#32145,#32146,#32147,#32148,#32149,#32150,#32151,#32152,#32153,
#32154,#32155,#32156,#32157,#32158,#32159,#32160,#32161,#32162,#32163,#32164,
#32165,#32166,#32167,#32168,#32169,#32170,#32171,#32172,#32173,#32174,#32175,
#32176,#32177,#32178,#32179,#32180,#32181,#32182,#32183,#32184),
 .UNSPECIFIED.,.F.,.F.,(4,1,1,1,1,1,1,1,1,1,1,1,1,1,1,1,1,1,1,1,1,1,1,1,
1,1,1,1,1,1,1,1,1,1,1,1,1,1,1,1,1,1,1,1,1,1,1,1,1,1,1,1,1,1,1,1,1,1,1,1,
1,1,1,1,1,1,1,1,1,1,1,1,1,1,1,1,1,4),(0.0345080125489109,0.0357142857142857,
0.0535714285714286,0.0714285714285714,0.0892857142857143,0.107142857142857,
0.125,0.133928571428571,0.142857142857143,0.158730158730159,0.174603174603175,
0.19047619047619,0.202380952380952,0.214285714285714,0.226190476190476,
0.238095238095238,0.25,0.261904761904762,0.273809523809524,0.279761904761905,
0.285714285714286,0.297619047619048,0.30952380952381,0.321428571428571,
0.333333333333333,0.349206349206349,0.365079365079365,0.373015873015873,
0.380952380952381,0.396825396825397,0.412698412698413,0.428571428571429,
0.444444444444444,0.46031746031746,0.476190476190476,0.492063492063492,
0.507936507936508,0.523809523809524,0.535714285714286,0.547619047619048,
0.55952380952381,0.571428571428571,0.583333333333333,0.595238095238095,
0.607142857142857,0.619047619047619,0.630952380952381,0.642857142857143,
0.654761904761905,0.666666666666667,0.682539682539682,0.698412698412698,
0.706349206349206,0.714285714285714,0.722222222222222,0.73015873015873,
0.746031746031746,0.761904761904762,0.773809523809524,0.785714285714286,
0.797619047619047,0.809523809523809,0.821428571428571,0.833333333333333,
0.845238095238095,0.857142857142857,0.861607142857143,0.866071428571429,
0.875,0.892857142857143,0.910714285714286,0.928571428571429,0.946428571428571,
0.964285714285714,0.973214285714286,0.982142857142857,0.991071428571429,
1.),.UNSPECIFIED.);
#581=B_SPLINE_CURVE_WITH_KNOTS('',3,(#32302,#32303,#32304,#32305,#32306,
#32307,#32308,#32309,#32310,#32311,#32312),.UNSPECIFIED.,.F.,.F.,(4,1,1,
1,1,1,1,1,4),(53.4070751110265,53.7139797041847,54.204378086024,54.6947764678633,
55.1851748497025,55.6755732315418,56.1659716133811,56.6563699952204,56.8720816739404),
 .UNSPECIFIED.);
#582=B_SPLINE_CURVE_WITH_KNOTS('',3,(#32315,#32316,#32317,#32318,#32319,
#32320,#32321,#32322,#32323,#32324),.UNSPECIFIED.,.F.,.F.,(4,1,1,1,1,1,
1,4),(53.4070751110265,53.622996627145,54.1133950089843,54.6037933908236,
55.0941917726629,55.5845901545022,56.0749885363414,56.5653869181807),
 .UNSPECIFIED.);
#583=B_SPLINE_CURVE_WITH_KNOTS('',3,(#32329,#32330,#32331,#32332,#32333,
#32334,#32335,#32336,#32337,#32338,#32339,#32340,#32341,#32342,#32343,#32344,
#32345),.UNSPECIFIED.,.F.,.F.,(4,1,1,1,1,1,1,1,1,1,1,1,1,1,4),(47.1238898038469,
47.338800740274,47.8291991221133,48.3195975039526,48.8099958857919,49.3003942676311,
49.7907926494704,50.2811910313097,50.771589413149,51.2619877949883,51.7523861768276,
52.2427845586669,52.7331829405061,53.2235813223454,53.4070751110265),
 .UNSPECIFIED.);
#584=B_SPLINE_CURVE_WITH_KNOTS('',3,(#32346,#32347,#32348,#32349,#32350,
#32351,#32352,#32353,#32354,#32355,#32356,#32357,#32358,#32359,#32360,#32361,
#32362),.UNSPECIFIED.,.F.,.F.,(4,1,1,1,1,1,1,1,1,1,1,1,1,1,4),(47.1238898038469,
47.2478176632343,47.7382160450736,48.2286144269129,48.7190128087522,49.2094111905915,
49.6998095724308,50.19020795427,50.6806063361093,51.1710047179486,51.6614030997879,
52.1518014816272,52.6421998634665,53.1325982453057,53.4070751110265),
 .UNSPECIFIED.);
#585=B_SPLINE_CURVE_WITH_KNOTS('',3,(#32367,#32368,#32369,#32370,#32371,
#32372,#32373,#32374,#32375,#32376,#32377,#32378,#32379,#32380,#32381,#32382,
#32383),.UNSPECIFIED.,.F.,.F.,(4,1,1,1,1,1,1,1,1,1,1,1,1,1,4),(40.8407044966673,
40.9636217763633,41.4540201582026,41.9444185400419,42.4348169218812,42.9252153037205,
43.4156136855597,43.906012067399,44.3964104492383,44.8868088310776,45.3772072129169,
45.8676055947562,46.3580039765954,46.8484023584347,47.1238898038469),
 .UNSPECIFIED.);
#586=B_SPLINE_CURVE_WITH_KNOTS('',3,(#32384,#32385,#32386,#32387,#32388,
#32389,#32390,#32391,#32392,#32393,#32394,#32395,#32396,#32397,#32398,#32399,
#32400),.UNSPECIFIED.,.F.,.F.,(4,1,1,1,1,1,1,1,1,1,1,1,1,1,4),(40.8407044966673,
40.8726386993237,41.3630370811629,41.8534354630022,42.3438338448415,42.8342322266808,
43.3246306085201,43.8150289903594,44.3054273721986,44.7958257540379,45.2862241358772,
45.7766225177165,46.2670208995558,46.7574192813951,47.1238898038469),
 .UNSPECIFIED.);
#587=B_SPLINE_CURVE_WITH_KNOTS('',3,(#32405,#32406,#32407,#32408,#32409,
#32410,#32411,#32412,#32413,#32414,#32415,#32416,#32417,#32418,#32419,#32420,
#32421),.UNSPECIFIED.,.F.,.F.,(4,1,1,1,1,1,1,1,1,1,1,1,1,1,4),(34.5575191894877,
34.5884428124526,35.0788411942919,35.5692395761312,36.0596379579705,36.5500363398098,
37.0404347216491,37.5308331034883,38.0212314853276,38.5116298671669,39.0020282490062,
39.4924266308455,39.9828250126848,40.473223394524,40.8407044966673),
 .UNSPECIFIED.);
#588=B_SPLINE_CURVE_WITH_KNOTS('',3,(#32422,#32423,#32424,#32425,#32426,
#32427,#32428,#32429,#32430,#32431,#32432,#32433,#32434,#32435,#32436,#32437),
 .UNSPECIFIED.,.F.,.F.,(4,1,1,1,1,1,1,1,1,1,1,1,1,4),(34.5575191894877,
34.9878581172523,35.4782564990915,35.9686548809308,36.4590532627701,36.9494516446094,
37.4398500264487,37.930248408288,38.4206467901272,38.9110451719665,39.4014435538058,
39.8918419356451,40.3822403174844,40.8407044966673),.UNSPECIFIED.);
#589=B_SPLINE_CURVE_WITH_KNOTS('',3,(#32442,#32443,#32444,#32445,#32446,
#32447,#32448,#32449,#32450,#32451,#32452,#32453,#32454,#32455,#32456,#32457),
 .UNSPECIFIED.,.F.,.F.,(4,1,1,1,1,1,1,1,1,1,1,1,1,4),(28.2743338823081,
28.7036622303812,29.1940606122205,29.6844589940598,30.1748573758991,30.6652557577384,
31.1556541395777,31.6460525214169,32.1364509032562,32.6268492850955,33.1172476669348,
33.6076460487741,34.0980444306134,34.5575191894877),.UNSPECIFIED.);
#590=B_SPLINE_CURVE_WITH_KNOTS('',3,(#32458,#32459,#32460,#32461,#32462,
#32463,#32464,#32465,#32466,#32467,#32468,#32469,#32470,#32471,#32472,#32473,
#32474),.UNSPECIFIED.,.F.,.F.,(4,1,1,1,1,1,1,1,1,1,1,1,1,1,4),(28.2743338823081,
28.6126791533416,29.1030775351808,29.5934759170201,30.0838742988594,30.5742726806987,
31.064671062538,31.5550694443773,32.0454678262165,32.5358662080558,33.0262645898951,
33.5166629717344,34.0070613535737,34.497459735413,34.5575191894877),
 .UNSPECIFIED.);
#591=B_SPLINE_CURVE_WITH_KNOTS('',3,(#32479,#32480,#32481,#32482,#32483,
#32484,#32485,#32486,#32487,#32488,#32489,#32490,#32491,#32492,#32493,#32494,
#32495),.UNSPECIFIED.,.F.,.F.,(4,1,1,1,1,1,1,1,1,1,1,1,1,1,4),(21.9911485751285,
22.3284832664706,22.8188816483098,23.3092800301491,23.7996784119884,24.2900767938277,
24.780475175667,25.2708735575063,25.7612719393455,26.2516703211848,26.7420687030241,
27.2324670848634,27.7228654667027,28.213263848542,28.2743338823081),
 .UNSPECIFIED.);
#592=B_SPLINE_CURVE_WITH_KNOTS('',3,(#32496,#32497,#32498,#32499,#32500,
#32501,#32502,#32503,#32504,#32505,#32506,#32507,#32508,#32509,#32510,#32511,
#32512),.UNSPECIFIED.,.F.,.F.,(4,1,1,1,1,1,1,1,1,1,1,1,1,1,4),(21.9911485751285,
22.2375001894309,22.7278985712702,23.2182969531094,23.7086953349487,24.199093716788,
24.6894920986273,25.1798904804666,25.6702888623059,26.1606872441451,26.6510856259844,
27.1414840078237,27.631882389663,28.1222807715023,28.2743338823081),
 .UNSPECIFIED.);
#593=B_SPLINE_CURVE_WITH_KNOTS('',3,(#32517,#32518,#32519,#32520,#32521,
#32522,#32523,#32524,#32525,#32526,#32527,#32528,#32529,#32530,#32531,#32532,
#32533),.UNSPECIFIED.,.F.,.F.,(4,1,1,1,1,1,1,1,1,1,1,1,1,1,4),(15.7079632679489,
15.9533043025599,16.4437026843992,16.9341010662384,17.4244994480777,17.914897829917,
18.4052962117563,18.8956945935956,19.3860929754349,19.8764913572741,20.3668897391134,
20.8572881209527,21.347686502792,21.8380848846313,21.9911485751285),
 .UNSPECIFIED.);
#594=B_SPLINE_CURVE_WITH_KNOTS('',3,(#32534,#32535,#32536,#32537,#32538,
#32539,#32540,#32541,#32542,#32543,#32544,#32545,#32546,#32547,#32548,#32549,
#32550),.UNSPECIFIED.,.F.,.F.,(4,1,1,1,1,1,1,1,1,1,1,1,1,1,4),(15.7079632679489,
15.8623212255202,16.3527196073595,16.8431179891988,17.333516371038,17.8239147528773,
18.3143131347166,18.8047115165559,19.2951098983952,19.7855082802345,20.2759066620737,
20.766305043913,21.2567034257523,21.7471018075916,21.9911485751285),
 .UNSPECIFIED.);
#595=B_SPLINE_CURVE_WITH_KNOTS('',3,(#32557,#32558,#32559,#32560,#32561,
#32562,#32563,#32564,#32565,#32566,#32567,#32568,#32569,#32570,#32571,#32572),
 .UNSPECIFIED.,.F.,.F.,(4,1,1,1,1,1,1,1,1,1,1,1,1,4),(9.57812533864918,
10.0685237204885,10.5589221023278,11.049320484167,11.5397188660063,12.0301172478456,
12.5205156296849,13.0109140115242,13.5013123933635,13.9917107752027,14.482109157042,
14.9725075388813,15.4629059207206,15.7079632679489),.UNSPECIFIED.);
#596=B_SPLINE_CURVE_WITH_KNOTS('',3,(#32573,#32574,#32575,#32576,#32577,
#32578,#32579,#32580,#32581,#32582,#32583,#32584,#32585,#32586,#32587,#32588,
#32589),.UNSPECIFIED.,.F.,.F.,(4,1,1,1,1,1,1,1,1,1,1,1,1,1,4),(9.42477796076936,
9.48714226160951,9.97754064344879,10.4679390252881,10.9583374071274,11.4487357889666,
11.9391341708059,12.4295325526452,12.9199309344845,13.4103293163238,13.9007276981631,
14.3911260800023,14.8815244618416,15.3719228436809,15.7079632679489),
 .UNSPECIFIED.);
#597=B_SPLINE_CURVE_WITH_KNOTS('',3,(#33097,#33098,#33099,#33100,#33101,
#33102,#33103,#33104),.UNSPECIFIED.,.F.,.F.,(4,2,2,4),(0.,0.303392014531492,
0.493985861454512,0.655896371978029),.UNSPECIFIED.);
#598=B_SPLINE_CURVE_WITH_KNOTS('',3,(#33106,#33107,#33108,#33109,#33110,
#33111,#33112,#33113,#33114,#33115,#33116,#33117,#33118,#33119,#33120,#33121,
#33122,#33123,#33124,#33125,#33126,#33127,#33128,#33129,#33130,#33131,#33132,
#33133,#33134,#33135,#33136,#33137,#33138,#33139,#33140,#33141,#33142,#33143,
#33144,#33145,#33146,#33147,#33148,#33149,#33150,#33151,#33152,#33153,#33154,
#33155,#33156,#33157,#33158,#33159,#33160,#33161,#33162,#33163,#33164,#33165,
#33166,#33167,#33168,#33169,#33170,#33171,#33172,#33173,#33174,#33175,#33176,
#33177,#33178,#33179,#33180,#33181,#33182,#33183,#33184,#33185,#33186,#33187,
#33188,#33189,#33190,#33191,#33192,#33193,#33194,#33195,#33196,#33197,#33198,
#33199,#33200,#33201,#33202,#33203,#33204,#33205,#33206,#33207,#33208,#33209,
#33210,#33211,#33212,#33213,#33214,#33215,#33216,#33217,#33218,#33219,#33220,
#33221,#33222,#33223,#33224,#33225,#33226,#33227,#33228,#33229,#33230,#33231,
#33232,#33233,#33234,#33235,#33236,#33237,#33238,#33239,#33240,#33241,#33242,
#33243,#33244,#33245,#33246,#33247,#33248,#33249,#33250,#33251,#33252,#33253,
#33254,#33255,#33256,#33257,#33258,#33259,#33260,#33261,#33262,#33263,#33264,
#33265,#33266,#33267,#33268,#33269,#33270,#33271,#33272,#33273,#33274,#33275,
#33276,#33277,#33278,#33279,#33280,#33281,#33282,#33283,#33284,#33285,#33286,
#33287,#33288,#33289,#33290,#33291,#33292,#33293,#33294,#33295,#33296,#33297,
#33298,#33299,#33300,#33301,#33302,#33303,#33304,#33305,#33306,#33307,#33308,
#33309,#33310,#33311,#33312,#33313,#33314,#33315,#33316,#33317,#33318,#33319,
#33320,#33321,#33322,#33323,#33324,#33325,#33326,#33327,#33328,#33329,#33330,
#33331,#33332,#33333,#33334,#33335,#33336,#33337,#33338,#33339,#33340,#33341,
#33342,#33343,#33344,#33345,#33346,#33347,#33348,#33349,#33350,#33351,#33352,
#33353,#33354,#33355,#33356,#33357,#33358,#33359,#33360,#33361,#33362,#33363,
#33364,#33365,#33366,#33367,#33368,#33369,#33370,#33371,#33372,#33373,#33374,
#33375,#33376,#33377,#33378,#33379,#33380,#33381,#33382,#33383,#33384,#33385,
#33386,#33387,#33388,#33389,#33390,#33391,#33392,#33393,#33394,#33395,#33396,
#33397),.UNSPECIFIED.,.F.,.F.,(4,3,3,3,3,3,3,3,3,3,3,3,3,3,3,3,3,3,3,3,
3,3,3,3,3,3,3,3,3,3,3,3,3,3,3,3,3,3,3,3,3,3,3,3,3,3,3,3,3,3,3,3,3,3,3,3,
3,3,3,3,3,3,3,3,3,3,3,3,3,3,3,3,3,3,3,3,3,3,3,3,3,3,3,3,3,3,3,3,3,3,3,3,
3,3,3,3,3,4),(0.,0.490398381839284,0.980796763678568,1.47119514551785,1.96159352735713,
2.45199190919642,2.9423902910357,3.43278867287498,3.92318705471427,4.41358543655355,
4.90398381839284,5.39438220023212,5.8847805820714,6.37517896391069,6.86557734574997,
7.35597572758925,7.84637410942854,8.33677249126782,8.8271708731071,9.31756925494639,
9.80796763678567,10.298366018625,10.7887644004642,11.2791627823035,11.7695611641428,
12.2599595459821,12.7503579278214,13.2407563096607,13.7311546914999,14.2215530733392,
14.7119514551785,15.2023498370178,15.6927482188571,16.1831466006964,16.6735449825356,
17.1639433643749,17.6543417462142,18.1447401280535,18.6351385098928,19.1255368917321,
19.6159352735713,20.1063336554106,20.5967320372499,21.0871304190892,21.5775288009285,
22.0679271827678,22.558325564607,23.0487239464463,23.5391223282856,24.0295207101249,
24.5199190919642,25.0103174738035,25.5007158556427,25.991114237482,26.4815126193213,
26.9719110011606,27.4623093829999,27.9527077648392,28.4431061466784,28.9335045285177,
29.423902910357,29.9143012921963,30.4046996740356,30.8950980558749,31.3854964377141,
31.8758948195534,32.3662932013927,32.856691583232,33.3470899650713,33.8374883469106,
34.3278867287498,34.8182851105891,35.3086834924284,35.7990818742677,36.289480256107,
36.7798786379463,37.2702770197855,37.7606754016248,38.2510737834641,38.7414721653034,
39.2318705471427,39.722268928982,40.2126673108212,40.7030656926605,41.1934640744998,
41.6838624563391,42.1742608381784,42.6646592200177,43.1550576018569,43.6454559836962,
44.1358543655355,44.6262527473748,45.1166511292141,45.6070495110534,46.0974478928927,
46.5878462747319,47.0782446565712,47.2939563352912),.UNSPECIFIED.);
#599=B_SPLINE_CURVE_WITH_KNOTS('',3,(#33399,#33400,#33401,#33402,#33403,
#33404,#33405,#33406),.UNSPECIFIED.,.F.,.F.,(4,2,2,4),(-0.65589582858317,
-0.493988108841952,-0.303390394118172,0.),.UNSPECIFIED.);
#600=B_SPLINE_CURVE_WITH_KNOTS('',3,(#33407,#33408,#33409,#33410,#33411,
#33412,#33413,#33414,#33415,#33416,#33417,#33418,#33419,#33420,#33421,#33422,
#33423,#33424,#33425,#33426,#33427,#33428,#33429,#33430,#33431,#33432,#33433,
#33434,#33435,#33436,#33437,#33438,#33439,#33440,#33441,#33442,#33443,#33444,
#33445,#33446,#33447,#33448,#33449,#33450,#33451,#33452,#33453,#33454,#33455,
#33456,#33457,#33458,#33459,#33460,#33461,#33462,#33463,#33464,#33465,#33466,
#33467,#33468,#33469,#33470,#33471,#33472,#33473,#33474,#33475,#33476,#33477,
#33478,#33479,#33480,#33481,#33482,#33483,#33484,#33485,#33486,#33487,#33488,
#33489,#33490,#33491,#33492,#33493,#33494,#33495,#33496,#33497,#33498,#33499,
#33500,#33501,#33502,#33503,#33504,#33505,#33506),.UNSPECIFIED.,.F.,.F.,
(4,1,1,1,1,1,1,1,1,1,1,1,1,1,1,1,1,1,1,1,1,1,1,1,1,1,1,1,1,1,1,1,1,1,1,
1,1,1,1,1,1,1,1,1,1,1,1,1,1,1,1,1,1,1,1,1,1,1,1,1,1,1,1,1,1,1,1,1,1,1,1,
1,1,1,1,1,1,1,1,1,1,1,1,1,1,1,1,1,1,1,1,1,1,1,1,1,1,4),(7.04827039213814,
7.26398207085813,7.75438045269741,8.24477883453669,8.73517721637598,9.22557559821526,
9.71597398005454,10.2063723618938,10.6967707437331,11.1871691255724,11.6775675074117,
12.167965889251,12.6583642710902,13.1487626529295,13.6391610347688,14.1295594166081,
14.6199577984474,15.1103561802867,15.6007545621259,16.0911529439652,16.5815513258045,
17.0719497076438,17.5623480894831,18.0527464713224,18.5431448531616,19.0335432350009,
19.5239416168402,20.0143399986795,20.5047383805188,20.9951367623581,21.4855351441973,
21.9759335260366,22.4663319078759,22.9567302897152,23.4471286715545,23.9375270533938,
24.427925435233,24.9183238170723,25.4087221989116,25.8991205807509,26.3895189625902,
26.8799173444295,27.3703157262687,27.860714108108,28.3511124899473,28.8415108717866,
29.3319092536259,29.8223076354652,30.3127060173044,30.8031043991437,31.293502780983,
31.7839011628223,32.2742995446616,32.7646979265009,33.2550963083402,33.7454946901794,
34.2358930720187,34.726291453858,35.2166898356973,35.7070882175366,36.1974865993759,
36.6878849812151,37.1782833630544,37.6686817448937,38.159080126733,38.6494785085723,
39.1398768904116,39.6302752722508,40.1206736540901,40.6110720359294,41.1014704177687,
41.591868799608,42.0822671814473,42.5726655632865,43.0630639451258,43.5534623269651,
44.0438607088044,44.5342590906437,45.024657472483,45.5150558543222,46.0054542361615,
46.4958526180008,46.9862509998401,47.4766493816794,47.9670477635187,48.4574461453579,
48.9478445271972,49.4382429090365,49.9286412908758,50.4190396727151,50.9094380545544,
51.3998364363936,51.8902348182329,52.3806332000722,52.8710315819115,53.3614299637508,
53.8518283455901,54.3422267274293),.UNSPECIFIED.);
#601=B_SPLINE_CURVE_WITH_KNOTS('',3,(#33912,#33913,#33914,#33915,#33916,
#33917,#33918,#33919,#33920,#33921,#33922,#33923,#33924,#33925,#33926,#33927,
#33928,#33929,#33930,#33931,#33932,#33933,#33934,#33935,#33936,#33937,#33938,
#33939,#33940,#33941,#33942,#33943,#33944,#33945,#33946,#33947,#33948,#33949,
#33950,#33951,#33952,#33953,#33954,#33955,#33956,#33957,#33958,#33959,#33960,
#33961,#33962,#33963),.UNSPECIFIED.,.F.,.F.,(4,3,3,3,3,3,3,3,3,3,3,3,3,
3,3,3,3,4),(0.,0.113340575159357,0.226679014314907,0.308971226978626,0.33157413936908,
0.375660801919025,0.487626538864722,0.577647057858466,0.619647639286856,
0.64272677861779,0.752674952041405,0.769690750751205,0.865631662359576,
0.890410497383802,0.914699066264647,1.0235933763044,1.1305555281797,1.15345439718469),
 .UNSPECIFIED.);
#602=B_SPLINE_CURVE_WITH_KNOTS('',3,(#33965,#33966,#33967,#33968,#33969,
#33970,#33971,#33972,#33973,#33974,#33975,#33976,#33977,#33978,#33979,#33980,
#33981,#33982,#33983,#33984,#33985,#33986,#33987,#33988,#33989,#33990,#33991,
#33992,#33993,#33994,#33995,#33996,#33997,#33998,#33999,#34000,#34001,#34002,
#34003,#34004,#34005,#34006,#34007,#34008,#34009,#34010,#34011,#34012,#34013),
 .UNSPECIFIED.,.F.,.F.,(4,3,3,3,3,3,3,3,3,3,3,3,3,3,3,3,4),(-1.15345439718468,
-1.04561219422333,-0.936713145930038,-0.898860433224647,-0.874966557602631,
-0.796527420497185,-0.698191229719559,-0.637686241518532,-0.608878950476881,
-0.496956393340814,-0.403182657386682,-0.351450861947777,-0.316015134691263,
-0.293361871620024,-0.18057397642641,-0.0674064753207201,0.),
 .UNSPECIFIED.);
#603=B_SPLINE_CURVE_WITH_KNOTS('',3,(#34014,#34015,#34016,#34017,#34018,
#34019,#34020,#34021,#34022,#34023,#34024,#34025,#34026,#34027,#34028,#34029,
#34030,#34031,#34032,#34033,#34034,#34035,#34036,#34037,#34038,#34039,#34040,
#34041,#34042,#34043,#34044,#34045,#34046,#34047,#34048,#34049,#34050,#34051,
#34052,#34053,#34054,#34055,#34056,#34057,#34058,#34059,#34060,#34061,#34062,
#34063,#34064,#34065,#34066,#34067,#34068,#34069,#34070,#34071,#34072,#34073,
#34074,#34075,#34076,#34077,#34078,#34079,#34080,#34081,#34082,#34083,#34084,
#34085,#34086,#34087,#34088,#34089,#34090,#34091,#34092,#34093,#34094,#34095,
#34096,#34097,#34098,#34099,#34100,#34101,#34102,#34103,#34104,#34105,#34106,
#34107,#34108,#34109,#34110,#34111,#34112),.UNSPECIFIED.,.F.,.F.,(4,1,1,
1,1,1,1,1,1,1,1,1,1,1,1,1,1,1,1,1,1,1,1,1,1,1,1,1,1,1,1,1,1,1,1,1,1,1,1,
1,1,1,1,1,1,1,1,1,1,1,1,1,1,1,1,1,1,1,1,1,1,1,1,1,1,1,1,1,1,1,1,1,1,1,1,
1,1,1,1,1,1,1,1,1,1,1,1,1,1,1,1,1,1,1,1,1,4),(8.50634549793094,8.5406795178856,
9.03814922646809,9.53561893505058,10.0330886436331,10.5305583522156,11.0280280607981,
11.5254977693805,12.022967477963,12.5204371865455,13.017906895128,13.5153766037105,
14.012846312293,14.5103160208755,15.007785729458,15.5052554380405,16.002725146623,
16.5001948552054,16.9976645637879,17.4951342723704,17.9926039809529,18.4900736895354,
18.9875433981179,19.4850131067004,19.9824828152829,20.4799525238654,20.9774222324479,
21.4748919410303,21.9723616496128,22.4698313581953,22.9673010667778,23.4647707753603,
23.9622404839428,24.4597101925253,24.9571799011078,25.4546496096903,25.9521193182728,
26.4495890268552,26.9470587354377,27.4445284440202,27.9419981526027,28.4394678611852,
28.9369375697677,29.4344072783502,29.9318769869327,30.4293466955152,30.9268164040977,
31.4242861126801,31.9217558212626,32.4192255298451,32.9166952384276,33.4141649470101,
33.9116346555926,34.4091043641751,34.9065740727576,35.4040437813401,35.9015134899225,
36.398983198505,36.8964529070875,37.39392261567,37.8913923242525,38.388862032835,
38.8863317414175,39.38380145,39.8812711585825,40.378740867165,40.8762105757474,
41.3736802843299,41.8711499929124,42.3686197014949,42.8660894100774,43.3635591186599,
43.8610288272424,44.3584985358249,44.8559682444074,45.3534379529899,45.8509076615723,
46.3483773701548,46.8458470787373,47.3433167873198,47.8407864959023,48.3382562044848,
48.8357259130673,49.3331956216498,49.8306653302323,50.3281350388148,50.8256047473972,
51.3230744559797,51.8205441645622,52.3180138731447,52.8154835817272,53.3129532903097,
53.8104229988922,54.3078927074747,54.8053624160572,55.3028321246397,55.8003018332221),
 .UNSPECIFIED.);
#604=B_SPLINE_CURVE_WITH_KNOTS('',3,(#34618,#34619,#34620,#34621,#34622,
#34623,#34624,#34625),.UNSPECIFIED.,.F.,.F.,(4,2,2,4),(0.,0.169060128143195,
0.259665069689286,0.357335207358759),.UNSPECIFIED.);
#605=B_SPLINE_CURVE_WITH_KNOTS('',3,(#34627,#34628,#34629,#34630,#34631,
#34632,#34633,#34634),.UNSPECIFIED.,.F.,.F.,(4,2,2,4),(-0.357325312875839,
-0.2596648130129,-0.169069150031592,0.),.UNSPECIFIED.);
#606=B_SPLINE_CURVE_WITH_KNOTS('',3,(#34635,#34636,#34637,#34638),
 .UNSPECIFIED.,.F.,.F.,(4,4),(9.27143058288951,9.42477796076936),
 .UNSPECIFIED.);
#607=B_SPLINE_CURVE_WITH_KNOTS('',3,(#34644,#34645,#34646,#34647,#34648,
#34649,#34650,#34651),.UNSPECIFIED.,.F.,.F.,(4,2,2,4),(-0.415677006509016,
-0.300108570891024,-0.193253093542031,0.),.UNSPECIFIED.);
#608=B_SPLINE_CURVE_WITH_KNOTS('',3,(#34653,#34654,#34655,#34656,#34657,
#34658,#34659,#34660,#34661,#34662,#34663,#34664,#34665,#34666,#34667,#34668,
#34669,#34670,#34671,#34672,#34673,#34674,#34675,#34676,#34677,#34678,#34679,
#34680,#34681,#34682,#34683,#34684,#34685,#34686,#34687,#34688,#34689,#34690,
#34691,#34692,#34693,#34694,#34695,#34696,#34697,#34698,#34699,#34700,#34701),
 .UNSPECIFIED.,.F.,.F.,(4,3,3,3,3,3,3,3,3,3,3,3,3,3,3,3,4),(-1.15166532125566,
-1.03829677946555,-0.925260930580166,-0.889798588874509,-0.857950257399306,
-0.776795567921363,-0.678445564828452,-0.620287810074686,-0.586753712344115,
-0.476556476809781,-0.383395555549721,-0.332702788626051,-0.305063279660781,
-0.282851348861602,-0.174044273864526,-0.0667784584747076,0.),
 .UNSPECIFIED.);
#609=B_SPLINE_CURVE_WITH_KNOTS('',3,(#34702,#34703,#34704,#34705,#34706,
#34707),.UNSPECIFIED.,.F.,.F.,(4,2,4),(-0.659276662925395,-0.291453031942622,
0.),.UNSPECIFIED.);
#610=B_SPLINE_CURVE_WITH_KNOTS('',3,(#35216,#35217,#35218,#35219,#35220,
#35221),.UNSPECIFIED.,.F.,.F.,(4,2,4),(0.,0.291454760594741,0.659275699695529),
 .UNSPECIFIED.);
#611=B_SPLINE_CURVE_WITH_KNOTS('',3,(#35222,#35223,#35224,#35225,#35226,
#35227,#35228,#35229,#35230,#35231,#35232,#35233,#35234,#35235,#35236,#35237,
#35238,#35239,#35240,#35241,#35242,#35243,#35244,#35245,#35246,#35247,#35248,
#35249,#35250,#35251,#35252,#35253,#35254,#35255,#35256,#35257,#35258,#35259,
#35260,#35261,#35262,#35263,#35264,#35265,#35266,#35267,#35268,#35269,#35270,
#35271,#35272,#35273,#35274,#35275,#35276,#35277,#35278,#35279,#35280,#35281,
#35282,#35283,#35284,#35285,#35286,#35287,#35288,#35289,#35290,#35291,#35292,
#35293,#35294,#35295,#35296,#35297,#35298,#35299,#35300,#35301,#35302,#35303,
#35304,#35305,#35306,#35307,#35308,#35309,#35310,#35311,#35312,#35313,#35314,
#35315,#35316,#35317,#35318,#35319,#35320,#35321),.UNSPECIFIED.,.F.,.F.,
(4,1,1,1,1,1,1,1,1,1,1,1,1,1,1,1,1,1,1,1,1,1,1,1,1,1,1,1,1,1,1,1,1,1,1,
1,1,1,1,1,1,1,1,1,1,1,1,1,1,1,1,1,1,1,1,1,1,1,1,1,1,1,1,1,1,1,1,1,1,1,1,
1,1,1,1,1,1,1,1,1,1,1,1,1,1,1,1,1,1,1,1,1,1,1,1,1,1,4),(10.3432104236078,
10.5589221023278,11.049320484167,11.5397188660063,12.0301172478456,12.5205156296849,
13.0109140115242,13.5013123933635,13.9917107752027,14.482109157042,14.9725075388813,
15.4629059207206,15.9533043025599,16.4437026843992,16.9341010662384,17.4244994480777,
17.914897829917,18.4052962117563,18.8956945935956,19.3860929754349,19.8764913572741,
20.3668897391134,20.8572881209527,21.347686502792,21.8380848846313,22.3284832664706,
22.8188816483098,23.3092800301491,23.7996784119884,24.2900767938277,24.780475175667,
25.2708735575063,25.7612719393455,26.2516703211848,26.7420687030241,27.2324670848634,
27.7228654667027,28.213263848542,28.7036622303812,29.1940606122205,29.6844589940598,
30.1748573758991,30.6652557577384,31.1556541395777,31.6460525214169,32.1364509032562,
32.6268492850955,33.1172476669348,33.6076460487741,34.0980444306134,34.5884428124526,
35.0788411942919,35.5692395761312,36.0596379579705,36.5500363398098,37.0404347216491,
37.5308331034883,38.0212314853276,38.5116298671669,39.0020282490062,39.4924266308455,
39.9828250126848,40.473223394524,40.9636217763633,41.4540201582026,41.9444185400419,
42.4348169218812,42.9252153037205,43.4156136855597,43.906012067399,44.3964104492383,
44.8868088310776,45.3772072129169,45.8676055947562,46.3580039765954,46.8484023584347,
47.338800740274,47.8291991221133,48.3195975039526,48.8099958857919,49.3003942676311,
49.7907926494704,50.2811910313097,50.771589413149,51.2619877949883,51.7523861768276,
52.2427845586669,52.7331829405061,53.2235813223454,53.7139797041847,54.204378086024,
54.6947764678633,55.1851748497025,55.6755732315418,56.1659716133811,56.6563699952204,
57.1467683770597,57.637166758899),.UNSPECIFIED.);
#612=B_SPLINE_CURVE_WITH_KNOTS('',3,(#35727,#35728,#35729,#35730,#35731,
#35732,#35733,#35734,#35735,#35736,#35737,#35738,#35739,#35740,#35741,#35742,
#35743,#35744,#35745,#35746,#35747,#35748,#35749,#35750,#35751,#35752,#35753,
#35754,#35755,#35756,#35757,#35758,#35759,#35760,#35761,#35762,#35763,#35764,
#35765,#35766,#35767,#35768,#35769,#35770,#35771,#35772,#35773,#35774,#35775,
#35776,#35777,#35778),.UNSPECIFIED.,.F.,.F.,(4,3,3,3,3,3,3,3,3,3,3,3,3,
3,3,3,3,4),(0.,0.107536136059931,0.216397453782157,0.296736912822655,0.319843387978689,
0.356604402276694,0.46652467054214,0.547074483570674,0.595815754020393,
0.619047604484214,0.731049962231847,0.749314772119407,0.849902409403466,
0.873496419878896,0.898389588300942,1.01139267280479,1.12432918309124,1.15166532125564),
 .UNSPECIFIED.);
#613=B_SPLINE_CURVE_WITH_KNOTS('',3,(#35779,#35780,#35781,#35782,#35783,
#35784,#35785,#35786,#35787,#35788,#35789,#35790,#35791,#35792,#35793,#35794,
#35795,#35796,#35797,#35798,#35799,#35800,#35801,#35802,#35803,#35804,#35805,
#35806,#35807,#35808,#35809,#35810,#35811,#35812,#35813,#35814,#35815,#35816,
#35817,#35818,#35819,#35820,#35821,#35822,#35823,#35824,#35825,#35826,#35827,
#35828,#35829,#35830,#35831,#35832,#35833,#35834,#35835,#35836,#35837,#35838,
#35839,#35840,#35841,#35842,#35843,#35844,#35845,#35846,#35847,#35848,#35849,
#35850,#35851,#35852,#35853,#35854,#35855,#35856,#35857,#35858,#35859,#35860,
#35861,#35862,#35863,#35864,#35865,#35866,#35867,#35868,#35869,#35870,#35871,
#35872,#35873,#35874,#35875,#35876,#35877),.UNSPECIFIED.,.F.,.F.,(4,1,1,
1,1,1,1,1,1,1,1,1,1,1,1,1,1,1,1,1,1,1,1,1,1,1,1,1,1,1,1,1,1,1,1,1,1,1,1,
1,1,1,1,1,1,1,1,1,1,1,1,1,1,1,1,1,1,1,1,1,1,1,1,1,1,1,1,1,1,1,1,1,1,1,1,
1,1,1,1,1,1,1,1,1,1,1,1,1,1,1,1,1,1,1,1,1,4),(11.8012855294006,11.8356195493552,
12.3330892579377,12.8305589665202,13.3280286751027,13.8254983836852,14.3229680922677,
14.8204378008502,15.3179075094327,15.8153772180151,16.3128469265976,16.8103166351801,
17.3077863437626,17.8052560523451,18.3027257609276,18.8001954695101,19.2976651780926,
19.7951348866751,20.2926045952576,20.79007430384,21.2875440124225,21.785013721005,
22.2824834295875,22.77995313817,23.2774228467525,23.774892555335,24.2723622639175,
24.7698319725,25.2673016810825,25.7647713896649,26.2622410982474,26.7597108068299,
27.2571805154124,27.7546502239949,28.2521199325774,28.7495896411599,29.2470593497424,
29.7445290583249,30.2419987669074,30.7394684754899,31.2369381840723,31.7344078926548,
32.2318776012373,32.7293473098198,33.2268170184023,33.7242867269848,34.2217564355673,
34.7192261441498,35.2166958527323,35.7141655613148,36.2116352698972,36.7091049784797,
37.2065746870622,37.7040443956447,38.2015141042272,38.6989838128097,39.1964535213922,
39.6939232299747,40.1913929385572,40.6888626471397,41.1863323557221,41.6838020643046,
42.1812717728871,42.6787414814696,43.1762111900521,43.6736808986346,44.1711506072171,
44.6686203157996,45.1660900243821,45.6635597329645,46.161029441547,46.6584991501295,
47.155968858712,47.6534385672945,48.150908275877,48.6483779844595,49.145847693042,
49.6433174016245,50.140787110207,50.6382568187894,51.1357265273719,51.6331962359544,
52.1306659445369,52.6281356531194,53.1256053617019,53.6230750702844,54.1205447788669,
54.6180144874494,55.1154841960319,55.6129539046143,56.1104236131968,56.6078933217793,
57.1053630303618,57.6028327389443,58.1003024475268,58.5977721561093,59.0952418646918),
 .UNSPECIFIED.);
#614=B_SPLINE_CURVE_WITH_KNOTS('',3,(#36383,#36384,#36385,#36386,#36387,
#36388,#36389,#36390),.UNSPECIFIED.,.F.,.F.,(4,2,2,4),(0.,0.193236966585146,
0.300098749787204,0.415673620384002),.UNSPECIFIED.);
#615=B_SPLINE_CURVE_WITH_KNOTS('',3,(#37146,#37147,#37148,#37149,#37150,
#37151,#37152,#37153,#37154,#37155,#37156),.UNSPECIFIED.,.F.,.F.,(4,1,1,
1,1,1,1,1,4),(34.5575191894877,34.9358901509145,35.4235394742273,35.91118879754,
36.3988381208528,36.8864874441656,37.3741367674784,37.8617860907912,38.0719996524582),
 .UNSPECIFIED.);
#616=B_SPLINE_CURVE_WITH_KNOTS('',3,(#37159,#37160,#37161,#37162,#37163,
#37164,#37165,#37166,#37167,#37168),.UNSPECIFIED.,.F.,.F.,(4,1,1,1,1,1,
1,4),(34.5575191894877,34.8394089568218,35.3270582801346,35.8147076034474,
36.3023569267602,36.790006250073,37.2776555733858,37.7653048966986),
 .UNSPECIFIED.);
#617=B_SPLINE_CURVE_WITH_KNOTS('',3,(#37173,#37174,#37175,#37176,#37177,
#37178,#37179,#37180,#37181,#37182,#37183,#37184,#37185,#37186,#37187,#37188,
#37189),.UNSPECIFIED.,.F.,.F.,(4,1,1,1,1,1,1,1,1,1,1,1,1,1,4),(28.2743338823081,
28.5964489478482,29.0840982711609,29.5717475944737,30.0593969177865,30.5470462410993,
31.0346955644121,31.5223448877249,32.0099942110377,32.4976435343505,32.9852928576633,
33.4729421809761,33.9605915042889,34.4482408276017,34.5575191894877),
 .UNSPECIFIED.);
#618=B_SPLINE_CURVE_WITH_KNOTS('',3,(#37190,#37191,#37192,#37193,#37194,
#37195,#37196,#37197,#37198,#37199,#37200,#37201,#37202,#37203,#37204,#37205,
#37206),.UNSPECIFIED.,.F.,.F.,(4,1,1,1,1,1,1,1,1,1,1,1,1,1,4),(28.2743338823081,
28.4999677537555,28.9876170770683,29.4752664003811,29.9629157236939,30.4505650470067,
30.9382143703195,31.4258636936323,31.913513016945,32.4011623402578,32.8888116635706,
33.3764609868834,33.8641103101962,34.351759633509,34.5575191894877),
 .UNSPECIFIED.);
#619=B_SPLINE_CURVE_WITH_KNOTS('',3,(#37211,#37212,#37213,#37214,#37215,
#37216,#37217,#37218,#37219,#37220,#37221,#37222,#37223,#37224,#37225,#37226,
#37227),.UNSPECIFIED.,.F.,.F.,(4,1,1,1,1,1,1,1,1,1,1,1,1,1,4),(21.9911485751285,
22.2570077447818,22.7446570680946,23.2323063914074,23.7199557147202,24.207605038033,
24.6952543613458,25.1829036846586,25.6705530079714,26.1582023312842,26.645851654597,
27.1335009779098,27.6211503012226,28.1087996245354,28.2743338823081),
 .UNSPECIFIED.);
#620=B_SPLINE_CURVE_WITH_KNOTS('',3,(#37228,#37229,#37230,#37231,#37232,
#37233,#37234,#37235,#37236,#37237,#37238,#37239,#37240,#37241,#37242,#37243,
#37244),.UNSPECIFIED.,.F.,.F.,(4,1,1,1,1,1,1,1,1,1,1,1,1,1,4),(21.9911485751285,
22.1605265506892,22.648175874002,23.1358251973148,23.6234745206276,24.1111238439404,
24.5987731672532,25.0864224905659,25.5740718138787,26.0617211371915,26.5493704605043,
27.0370197838171,27.5246691071299,28.0123184304427,28.2743338823081),
 .UNSPECIFIED.);
#621=B_SPLINE_CURVE_WITH_KNOTS('',3,(#37249,#37250,#37251,#37252,#37253,
#37254,#37255,#37256,#37257,#37258,#37259,#37260,#37261,#37262,#37263,#37264,
#37265),.UNSPECIFIED.,.F.,.F.,(4,1,1,1,1,1,1,1,1,1,1,1,1,1,4),(15.707963267949,
15.9175665417155,16.4052158650283,16.8928651883411,17.3805145116539,17.8681638349667,
18.3558131582795,18.8434624815923,19.3311118049051,19.8187611282179,20.3064104515307,
20.7940597748435,21.2817090981563,21.7693584214691,21.9911485751285),
 .UNSPECIFIED.);
#622=B_SPLINE_CURVE_WITH_KNOTS('',3,(#37266,#37267,#37268,#37269,#37270,
#37271,#37272,#37273,#37274,#37275,#37276,#37277,#37278,#37279,#37280,#37281,
#37282),.UNSPECIFIED.,.F.,.F.,(4,1,1,1,1,1,1,1,1,1,1,1,1,1,4),(15.707963267949,
15.8210853476229,16.3087346709357,16.7963839942485,17.2840333175613,17.771682640874,
18.2593319641868,18.7469812874996,19.2346306108124,19.7222799341252,20.209929257438,
20.6975785807508,21.1852279040636,21.6728772273764,21.9911485751285),
 .UNSPECIFIED.);
#623=B_SPLINE_CURVE_WITH_KNOTS('',3,(#37289,#37290,#37291,#37292,#37293,
#37294,#37295,#37296,#37297,#37298,#37299,#37300,#37301,#37302,#37303,#37304),
 .UNSPECIFIED.,.F.,.F.,(4,1,1,1,1,1,1,1,1,1,1,1,1,4),(9.57812533864923,
10.065774661962,10.5534239852748,11.0410733085876,11.5287226319004,12.0163719552132,
12.504021278526,12.9916706018388,13.4793199251516,13.9669692484644,14.4546185717772,
14.94226789509,15.4299172184027,15.707963267949),.UNSPECIFIED.);
#624=B_SPLINE_CURVE_WITH_KNOTS('',3,(#37305,#37306,#37307,#37308,#37309,
#37310,#37311,#37312,#37313,#37314,#37315,#37316,#37317,#37318,#37319,#37320,
#37321),.UNSPECIFIED.,.F.,.F.,(4,1,1,1,1,1,1,1,1,1,1,1,1,1,4),(9.42477796076937,
9.48164414455657,9.96929346786936,10.4569427911822,10.9445921144949,11.4322414378077,
11.9198907611205,12.4075400844333,12.8951894077461,13.3828387310589,13.8704880543717,
14.3581373776845,14.8457867009973,15.3334360243101,15.707963267949),
 .UNSPECIFIED.);
#625=B_SPLINE_CURVE_WITH_KNOTS('',3,(#37327,#37328,#37329,#37330,#37331,
#37332,#37333,#37334,#37335,#37336,#37337,#37338,#37339,#37340,#37341,#37342),
 .UNSPECIFIED.,.F.,.F.,(4,3,3,3,3,4),(-4.09323272002467,-3.9955596755733,
-3.49611471612663,-2.99666975667997,-2.49722479723331,-2.07135887395548),
 .UNSPECIFIED.);
#626=B_SPLINE_CURVE_WITH_KNOTS('',3,(#37345,#37346,#37347,#37348,#37349,
#37350,#37351,#37352,#37353,#37354),.UNSPECIFIED.,.F.,.F.,(4,3,3,4),(0.,
0.499444959446661,0.998889918893321,1.11971880752059),.UNSPECIFIED.);
#627=B_SPLINE_CURVE_WITH_KNOTS('',3,(#37359,#37360,#37361,#37362,#37363,
#37364,#37365,#37366,#37367,#37368,#37369,#37370,#37371,#37372,#37373,#37374,
#37375,#37376,#37377,#37378,#37379,#37380,#37381,#37382,#37383,#37384,#37385,
#37386,#37387,#37388,#37389,#37390,#37391,#37392,#37393,#37394,#37395,#37396,
#37397,#37398),.UNSPECIFIED.,.F.,.F.,(4,3,3,3,3,3,3,3,3,3,3,3,3,4),(-10.3764180272043,
-9.98889918893324,-9.48945422948658,-8.99000927003992,-8.49056431059325,
-7.99111935114659,-7.49167439169993,-6.99222943225327,-6.49278447280661,
-5.99333951335995,-5.49389455391328,-4.99444959446662,-4.49500463501996,
-4.09323272002467),.UNSPECIFIED.);
#628=B_SPLINE_CURVE_WITH_KNOTS('',3,(#37399,#37400,#37401,#37402,#37403,
#37404,#37405,#37406,#37407,#37408,#37409,#37410,#37411,#37412,#37413,#37414,
#37415,#37416,#37417,#37418,#37419,#37420,#37421,#37422,#37423,#37424,#37425,
#37426,#37427,#37428,#37429,#37430,#37431,#37432,#37433,#37434,#37435,#37436,
#37437,#37438),.UNSPECIFIED.,.F.,.F.,(4,3,3,3,3,3,3,3,3,3,3,3,3,4),(1.11971880752059,
1.49833487833998,1.99777983778665,2.4972247972333,2.99666975667997,3.49611471612663,
3.99555967557329,4.49500463501995,4.99444959446662,5.49389455391328,5.99333951335994,
6.4927844728066,6.99222943225326,7.40290411470018),.UNSPECIFIED.);
#629=B_SPLINE_CURVE_WITH_KNOTS('',3,(#37443,#37444,#37445,#37446,#37447,
#37448,#37449,#37450,#37451,#37452,#37453,#37454,#37455,#37456,#37457,#37458,
#37459,#37460,#37461,#37462,#37463,#37464,#37465,#37466,#37467,#37468,#37469,
#37470,#37471,#37472,#37473,#37474,#37475,#37476,#37477,#37478,#37479,#37480,
#37481,#37482,#37483,#37484,#37485),.UNSPECIFIED.,.F.,.F.,(4,3,3,3,3,3,
3,3,3,3,3,3,3,3,4),(-16.6596033343838,-16.4816836617398,-15.9822387022932,
-15.4827937428465,-14.9833487833999,-14.4839038239532,-13.9844588645065,
-13.4850139050599,-12.9855689456132,-12.4861239861666,-11.9866790267199,
-11.4872340672732,-10.9877891078266,-10.4883441483799,-10.3764180272043),
 .UNSPECIFIED.);
#630=B_SPLINE_CURVE_WITH_KNOTS('',3,(#37486,#37487,#37488,#37489,#37490,
#37491,#37492,#37493,#37494,#37495,#37496,#37497,#37498,#37499,#37500,#37501,
#37502,#37503,#37504,#37505,#37506,#37507,#37508,#37509,#37510,#37511,#37512,
#37513,#37514,#37515,#37516,#37517,#37518,#37519,#37520,#37521,#37522,#37523,
#37524,#37525,#37526,#37527,#37528),.UNSPECIFIED.,.F.,.F.,(4,3,3,3,3,3,
3,3,3,3,3,3,3,3,4),(7.40290411470018,7.49167439169993,7.99111935114659,
8.49056431059325,8.99000927003991,9.48945422948658,9.98889918893324,10.4883441483799,
10.9877891078266,11.4872340672732,11.9866790267199,12.4861239861666,12.9855689456132,
13.4850139050599,13.6860894218798),.UNSPECIFIED.);
#631=B_SPLINE_CURVE_WITH_KNOTS('',3,(#37533,#37534,#37535,#37536,#37537,
#37538,#37539,#37540,#37541,#37542,#37543,#37544,#37545,#37546,#37547,#37548,
#37549,#37550,#37551,#37552,#37553,#37554,#37555,#37556,#37557,#37558,#37559,
#37560,#37561,#37562,#37563,#37564,#37565,#37566,#37567,#37568,#37569,#37570,
#37571,#37572),.UNSPECIFIED.,.F.,.F.,(4,3,3,3,3,3,3,3,3,3,3,3,3,4),(-22.9427886415634,
-22.4750231750998,-21.9755782156531,-21.4761332562065,-20.9766882967598,
-20.4772433373131,-19.9777983778665,-19.4783534184198,-18.9789084589732,
-18.4794634995265,-17.9800185400798,-17.4805735806332,-16.9811286211865,
-16.6596033343838),.UNSPECIFIED.);
#632=B_SPLINE_CURVE_WITH_KNOTS('',3,(#37573,#37574,#37575,#37576,#37577,
#37578,#37579,#37580,#37581,#37582,#37583,#37584,#37585,#37586,#37587,#37588,
#37589,#37590,#37591,#37592,#37593,#37594,#37595,#37596,#37597,#37598,#37599,
#37600,#37601,#37602,#37603,#37604,#37605,#37606,#37607,#37608,#37609,#37610,
#37611,#37612),.UNSPECIFIED.,.F.,.F.,(4,3,3,3,3,3,3,3,3,3,3,3,3,4),(13.6860894218798,
13.9844588645065,14.4839038239532,14.9833487833999,15.4827937428465,15.9822387022932,
16.4816836617398,16.9811286211865,17.4805735806332,17.9800185400798,18.4794634995265,
18.9789084589732,19.4783534184198,19.9692747290593),.UNSPECIFIED.);
#633=B_SPLINE_CURVE_WITH_KNOTS('',3,(#37617,#37618,#37619,#37620,#37621,
#37622,#37623,#37624,#37625,#37626,#37627,#37628,#37629,#37630,#37631,#37632,
#37633,#37634,#37635,#37636,#37637,#37638,#37639,#37640,#37641,#37642,#37643,
#37644,#37645,#37646,#37647,#37648,#37649,#37650,#37651,#37652,#37653,#37654,
#37655,#37656,#37657,#37658,#37659),.UNSPECIFIED.,.F.,.F.,(4,3,3,3,3,3,
3,3,3,3,3,3,3,3,4),(-29.225973948743,-28.9678076479064,-28.4683626884597,
-27.9689177290131,-27.4694727695664,-26.9700278101197,-26.4705828506731,
-25.9711378912264,-25.4716929317798,-24.9722479723331,-24.4728030128864,
-23.9733580534398,-23.4739130939931,-22.9744681345465,-22.9427886415634),
 .UNSPECIFIED.);
#634=B_SPLINE_CURVE_WITH_KNOTS('',3,(#37660,#37661,#37662,#37663,#37664,
#37665,#37666,#37667,#37668,#37669,#37670,#37671,#37672,#37673,#37674,#37675,
#37676,#37677,#37678,#37679,#37680,#37681,#37682,#37683,#37684,#37685,#37686,
#37687,#37688,#37689,#37690,#37691,#37692,#37693,#37694,#37695,#37696,#37697,
#37698,#37699,#37700,#37701,#37702),.UNSPECIFIED.,.F.,.F.,(4,3,3,3,3,3,
3,3,3,3,3,3,3,3,4),(19.9692747290593,19.9777983778665,20.4772433373131,
20.9766882967598,21.4761332562065,21.9755782156531,22.4750231750998,22.9744681345464,
23.4739130939931,23.9733580534398,24.4728030128864,24.9722479723331,25.4716929317798,
25.9711378912264,26.2524600362389),.UNSPECIFIED.);
#635=B_SPLINE_CURVE_WITH_KNOTS('',3,(#37707,#37708,#37709,#37710,#37711,
#37712,#37713,#37714,#37715,#37716,#37717,#37718,#37719,#37720,#37721,#37722,
#37723,#37724,#37725,#37726,#37727,#37728,#37729,#37730,#37731,#37732,#37733,
#37734,#37735,#37736,#37737,#37738,#37739,#37740,#37741,#37742,#37743,#37744,
#37745,#37746,#37747,#37748,#37749),.UNSPECIFIED.,.F.,.F.,(4,3,3,3,3,3,
3,3,3,3,3,3,3,3,4),(-35.5091592559226,-35.460592120713,-34.9611471612663,
-34.4617022018197,-33.962257242373,-33.4628122829264,-32.9633673234797,
-32.463922364033,-31.9644774045864,-31.4650324451397,-30.965587485693,-30.4661425262464,
-29.9666975667997,-29.4672526073531,-29.225973948743),.UNSPECIFIED.);
#636=B_SPLINE_CURVE_WITH_KNOTS('',3,(#37750,#37751,#37752,#37753,#37754,
#37755,#37756,#37757,#37758,#37759,#37760,#37761,#37762,#37763,#37764,#37765,
#37766,#37767,#37768,#37769,#37770,#37771,#37772,#37773,#37774,#37775,#37776,
#37777,#37778,#37779,#37780,#37781,#37782,#37783,#37784,#37785,#37786,#37787,
#37788,#37789,#37790,#37791,#37792),.UNSPECIFIED.,.F.,.F.,(4,3,3,3,3,3,
3,3,3,3,3,3,3,3,4),(26.2524600362389,26.4705828506731,26.9700278101197,
27.4694727695664,27.9689177290131,28.4683626884597,28.9678076479064,29.467252607353,
29.9666975667997,30.4661425262464,30.965587485693,31.4650324451397,31.9644774045864,
32.463922364033,32.5356453434185),.UNSPECIFIED.);
#637=B_SPLINE_CURVE_WITH_KNOTS('',3,(#37797,#37798,#37799,#37800,#37801,
#37802,#37803,#37804,#37805,#37806,#37807,#37808,#37809,#37810,#37811,#37812,
#37813,#37814,#37815,#37816,#37817,#37818,#37819,#37820,#37821,#37822,#37823,
#37824,#37825,#37826,#37827,#37828,#37829,#37830,#37831,#37832,#37833,#37834,
#37835,#37836),.UNSPECIFIED.,.F.,.F.,(4,3,3,3,3,3,3,3,3,3,3,3,3,4),(-41.7923445631022,
-41.453931634073,-40.9544866746263,-40.4550417151796,-39.955596755733,-39.4561517962863,
-38.9567068368396,-38.457261877393,-37.9578169179463,-37.4583719584997,
-36.958926999053,-36.4594820396063,-35.9600370801597,-35.5091592559226),
 .UNSPECIFIED.);
#638=B_SPLINE_CURVE_WITH_KNOTS('',3,(#37837,#37838,#37839,#37840,#37841,
#37842,#37843,#37844,#37845,#37846,#37847,#37848,#37849,#37850,#37851,#37852,
#37853,#37854,#37855,#37856,#37857,#37858,#37859,#37860,#37861,#37862,#37863,
#37864,#37865,#37866,#37867,#37868,#37869,#37870,#37871,#37872,#37873,#37874,
#37875,#37876),.UNSPECIFIED.,.F.,.F.,(4,3,3,3,3,3,3,3,3,3,3,3,3,4),(32.5356453434185,
32.9633673234797,33.4628122829263,33.962257242373,34.4617022018197,34.9611471612663,
35.460592120713,35.9600370801597,36.4594820396063,36.958926999053,37.4583719584996,
37.9578169179463,38.457261877393,38.8188306505981),.UNSPECIFIED.);
#639=B_SPLINE_CURVE_WITH_KNOTS('',3,(#37882,#37883,#37884,#37885,#37886,
#37887,#37888,#37889),.UNSPECIFIED.,.F.,.F.,(4,1,1,1,1,4),(53.4070751110265,
53.5681071414439,54.0675521008905,54.5669970603372,55.0664420197839,55.4923079430617),
 .UNSPECIFIED.);
#640=B_SPLINE_CURVE_WITH_KNOTS('',3,(#37892,#37893,#37894,#37895,#37896),
 .UNSPECIFIED.,.F.,.F.,(4,1,4),(53.4070751110265,53.754550462895,54.2539954223417),
 .UNSPECIFIED.);
#641=B_SPLINE_CURVE_WITH_KNOTS('',3,(#37901,#37902,#37903,#37904,#37905,
#37906,#37907,#37908,#37909,#37910,#37911,#37912,#37913,#37914,#37915,#37916),
 .UNSPECIFIED.,.F.,.F.,(4,1,1,1,1,1,1,1,1,1,1,1,1,4),(47.1238898038469,
47.5747676280839,48.0742125875306,48.5736575469773,49.0731025064239,49.5725474658706,
50.0719924253172,50.5714373847639,51.0708823442106,51.5703273036572,52.0697722631039,
52.5692172225505,53.0686621819972,53.4070751110265),.UNSPECIFIED.);
#642=B_SPLINE_CURVE_WITH_KNOTS('',3,(#37917,#37918,#37919,#37920,#37921,
#37922,#37923,#37924,#37925,#37926,#37927,#37928,#37929,#37930,#37931,#37932,
#37933),.UNSPECIFIED.,.F.,.F.,(4,1,1,1,1,1,1,1,1,1,1,1,1,1,4),(47.1238898038469,
47.2617659900884,47.7612109495351,48.2606559089817,48.7601008684284,49.2595458278751,
49.7589907873217,50.2584357467684,50.757880706215,51.2573256656617,51.7567706251084,
52.256215584555,52.7556605440017,53.2551055034483,53.4070751110265),
 .UNSPECIFIED.);
#643=B_SPLINE_CURVE_WITH_KNOTS('',3,(#37938,#37939,#37940,#37941,#37942,
#37943,#37944,#37945,#37946,#37947,#37948,#37949,#37950,#37951,#37952,#37953,
#37954),.UNSPECIFIED.,.F.,.F.,(4,1,1,1,1,1,1,1,1,1,1,1,1,1,4),(40.8407044966673,
41.0819831552773,41.581428114724,42.0808730741707,42.5803180336173,43.079762993064,
43.5792079525106,44.0786529119573,44.578097871404,45.0775428308506,45.5769877902973,
46.0764327497439,46.5758777091906,47.0753226686373,47.1238898038469),
 .UNSPECIFIED.);
#644=B_SPLINE_CURVE_WITH_KNOTS('',3,(#37955,#37956,#37957,#37958,#37959,
#37960,#37961,#37962,#37963,#37964,#37965,#37966,#37967,#37968,#37969,#37970),
 .UNSPECIFIED.,.F.,.F.,(4,1,1,1,1,1,1,1,1,1,1,1,1,4),(40.8407044966673,
41.2684264767285,41.7678714361751,42.2673163956218,42.7667613550684,43.2662063145151,
43.7656512739618,44.2650962334084,44.7645411928551,45.2639861523018,45.7634311117484,
46.2628760711951,46.7623210306417,47.1238898038469),.UNSPECIFIED.);
#645=B_SPLINE_CURVE_WITH_KNOTS('',3,(#37975,#37976,#37977,#37978,#37979,
#37980,#37981,#37982,#37983,#37984,#37985,#37986,#37987,#37988,#37989,#37990,
#37991),.UNSPECIFIED.,.F.,.F.,(4,1,1,1,1,1,1,1,1,1,1,1,1,1,4),(34.5575191894877,
34.5891986824707,35.0886436419174,35.588088601364,36.0875335608107,36.5869785202574,
37.086423479704,37.5858684391507,38.0853133985973,38.584758358044,39.0842033174907,
39.5836482769373,40.083093236384,40.5825381958307,40.8407044966673),
 .UNSPECIFIED.);
#646=B_SPLINE_CURVE_WITH_KNOTS('',3,(#37992,#37993,#37994,#37995,#37996,
#37997,#37998,#37999,#38000,#38001,#38002,#38003,#38004,#38005,#38006,#38007,
#38008),.UNSPECIFIED.,.F.,.F.,(4,1,1,1,1,1,1,1,1,1,1,1,1,1,4),(34.5575191894877,
34.7756420039219,35.2750869633685,35.7745319228152,36.2739768822618,36.7734218417085,
37.2728668011552,37.7723117606018,38.2717567200485,38.7712016794951,39.2706466389418,
39.7700915983885,40.2695365578351,40.7689815172818,40.8407044966673),
 .UNSPECIFIED.);
#647=B_SPLINE_CURVE_WITH_KNOTS('',3,(#38013,#38014,#38015,#38016,#38017,
#38018,#38019,#38020,#38021,#38022,#38023,#38024,#38025,#38026,#38027,#38028),
 .UNSPECIFIED.,.F.,.F.,(4,1,1,1,1,1,1,1,1,1,1,1,1,4),(28.2743338823081,
28.5958591691108,29.0953041285574,29.5947490880041,30.0941940474508,30.5936390068974,
31.0930839663441,31.5925289257907,32.0919738852374,32.5914188446841,33.0908638041307,
33.5903087635774,34.0897537230241,34.5575191894877),.UNSPECIFIED.);
#648=B_SPLINE_CURVE_WITH_KNOTS('',3,(#38029,#38030,#38031,#38032,#38033,
#38034,#38035,#38036,#38037,#38038,#38039,#38040,#38041,#38042,#38043,#38044,
#38045),.UNSPECIFIED.,.F.,.F.,(4,1,1,1,1,1,1,1,1,1,1,1,1,1,4),(28.2743338823081,
28.2828575311152,28.7823024905619,29.2817474500086,29.7811924094552,30.2806373689019,
30.7800823283486,31.2795272877952,31.7789722472419,32.2784172066885,32.7778621661352,
33.2773071255819,33.7767520850285,34.2761970444752,34.5575191894877),
 .UNSPECIFIED.);
#649=B_SPLINE_CURVE_WITH_KNOTS('',3,(#38050,#38051,#38052,#38053,#38054,
#38055,#38056,#38057,#38058,#38059,#38060,#38061,#38062,#38063,#38064,#38065,
#38066),.UNSPECIFIED.,.F.,.F.,(4,1,1,1,1,1,1,1,1,1,1,1,1,1,4),(21.9911485751285,
22.1030746963042,22.6025196557508,23.1019646151975,23.6014095746442,24.1008545340908,
24.6002994935375,25.0997444529841,25.5991894124308,26.0986343718775,26.5980793313241,
27.0975242907708,27.5969692502175,28.0964142096641,28.2743338823081),
 .UNSPECIFIED.);
#650=B_SPLINE_CURVE_WITH_KNOTS('',3,(#38067,#38068,#38069,#38070,#38071,
#38072,#38073,#38074,#38075,#38076,#38077,#38078,#38079,#38080,#38081,#38082),
 .UNSPECIFIED.,.F.,.F.,(4,1,1,1,1,1,1,1,1,1,1,1,1,4),(21.9911485751285,
22.2895180177553,22.788962977202,23.2884079366486,23.7878528960953,24.287297855542,
24.7867428149886,25.2861877744353,25.7856327338819,26.2850776933286,26.7845226527753,
27.2839676122219,27.7834125716686,28.2743338823081),.UNSPECIFIED.);
#651=B_SPLINE_CURVE_WITH_KNOTS('',3,(#38087,#38088,#38089,#38090,#38091,
#38092,#38093,#38094,#38095,#38096,#38097,#38098,#38099,#38100,#38101,#38102),
 .UNSPECIFIED.,.F.,.F.,(4,1,1,1,1,1,1,1,1,1,1,1,1,4),(15.7079632679489,
16.1097351829442,16.6091801423909,17.1086251018376,17.6080700612842,18.1075150207309,
18.6069599801775,19.1064049396242,19.6058498990709,20.1052948585175,20.6047398179642,
21.1041847774109,21.6036297368575,21.9911485751285),.UNSPECIFIED.);
#652=B_SPLINE_CURVE_WITH_KNOTS('',3,(#38103,#38104,#38105,#38106,#38107,
#38108,#38109,#38110,#38111,#38112,#38113,#38114,#38115,#38116,#38117,#38118,
#38119),.UNSPECIFIED.,.F.,.F.,(4,1,1,1,1,1,1,1,1,1,1,1,1,1,4),(15.7079632679489,
15.7967335449487,16.2961785043954,16.795623463842,17.2950684232887,17.7945133827353,
18.293958342182,18.7934033016287,19.2928482610753,19.792293220522,20.2917381799687,
20.7911831394153,21.290628098862,21.7900730583086,21.9911485751285),
 .UNSPECIFIED.);
#653=B_SPLINE_CURVE_WITH_KNOTS('',3,(#38122,#38123,#38124,#38125,#38126,
#38127,#38128,#38129,#38130,#38131,#38132,#38133,#38134,#38135,#38136,#38137,
#38138,#38139,#38140,#38141,#38142,#38143,#38144,#38145,#38146,#38147,#38148,
#38149,#38150,#38151,#38152,#38153,#38154,#38155,#38156,#38157,#38158,#38159,
#38160,#38161,#38162,#38163,#38164,#38165,#38166,#38167,#38168,#38169,#38170,
#38171,#38172,#38173,#38174,#38175,#38176,#38177,#38178,#38179,#38180,#38181,
#38182,#38183,#38184,#38185,#38186,#38187,#38188,#38189,#38190,#38191,#38192,
#38193,#38194),.UNSPECIFIED.,.F.,.F.,(4,3,3,3,3,3,3,3,3,3,3,3,3,3,3,3,3,
3,3,3,3,3,3,3,4),(-1.35394557174001,-1.30892768444359,-1.23102926805986,
-1.19688794819057,-1.17004272714157,-1.08368837302513,-1.04606736794041,
-1.01553569614099,-0.997334018908685,-0.903275013057271,-0.840846396492717,
-0.792075238959429,-0.767723825473952,-0.674993002634861,-0.591861111789504,
-0.541890483864056,-0.513413628060138,-0.415103168314629,-0.342465439253432,
-0.295139204862908,-0.267683354098771,-0.246657321726534,-0.147343803841858,
-0.0476021900320448,0.),.UNSPECIFIED.);
#654=B_SPLINE_CURVE_WITH_KNOTS('',3,(#38199,#38200,#38201,#38202,#38203,
#38204,#38205,#38206,#38207,#38208,#38209,#38210,#38211,#38212,#38213,#38214,
#38215,#38216,#38217,#38218,#38219,#38220,#38221,#38222,#38223,#38224,#38225,
#38226,#38227,#38228,#38229,#38230,#38231,#38232,#38233,#38234,#38235,#38236,
#38237,#38238,#38239,#38240,#38241,#38242,#38243,#38244,#38245,#38246,#38247,
#38248,#38249,#38250,#38251,#38252,#38253,#38254,#38255,#38256,#38257,#38258,
#38259,#38260,#38261,#38262,#38263,#38264,#38265,#38266,#38267,#38268,#38269,
#38270,#38271),.UNSPECIFIED.,.F.,.F.,(4,3,3,3,3,3,3,3,3,3,3,3,3,3,3,3,3,
3,3,3,3,3,3,3,4),(-1.3501974997237,-1.29933842216202,-1.21445175298089,
-1.17996490551909,-1.15395803466285,-1.05687489005017,-0.995259379032231,
-0.973262385119946,-0.959791745437487,-0.862294128942176,-0.765592015437111,
-0.740849630173425,-0.722135556856507,-0.62974877054122,-0.549747247506987,
-0.504760312423779,-0.483247297343189,-0.389544187887911,-0.30974267840429,
-0.263847143486886,-0.242838513083088,-0.223579745215157,-0.131366862398016,
-0.0408081318941806,0.),.UNSPECIFIED.);
#655=B_SPLINE_CURVE_WITH_KNOTS('',3,(#38652,#38653,#38654,#38655,#38656,
#38657,#38658,#38659,#38660,#38661,#38662,#38663,#38664,#38665,#38666,#38667,
#38668,#38669,#38670,#38671,#38672,#38673,#38674,#38675,#38676,#38677,#38678,
#38679,#38680,#38681,#38682,#38683,#38684,#38685),.UNSPECIFIED.,.F.,.F.,
(4,3,3,3,3,3,3,3,3,3,3,4),(38.8188306505981,38.9567068368396,39.4561517962863,
39.955596755733,40.4550417151796,40.9544866746263,41.4539316340729,41.9533765935196,
42.4528215529663,42.9522665124129,43.4517114718596,43.8775773951374),
 .UNSPECIFIED.);
#656=B_SPLINE_CURVE_WITH_KNOTS('',3,(#38687,#38688,#38689,#38690,#38691,
#38692,#38693,#38694,#38695,#38696,#38697,#38698,#38699,#38700,#38701,#38702,
#38703,#38704,#38705,#38706,#38707,#38708,#38709,#38710,#38711,#38712,#38713,
#38714,#38715,#38716,#38717,#38718,#38719,#38720,#38721,#38722,#38723,#38724,
#38725,#38726,#38727,#38728,#38729,#38730,#38731,#38732,#38733,#38734,#38735,
#38736,#38737,#38738,#38739,#38740,#38741,#38742,#38743,#38744,#38745,#38746,
#38747,#38748,#38749,#38750,#38751,#38752,#38753,#38754,#38755,#38756,#38757,
#38758,#38759),.UNSPECIFIED.,.F.,.F.,(4,3,3,3,3,3,3,3,3,3,3,3,3,3,3,3,3,
3,3,3,3,3,3,3,4),(-1.35394557173993,-1.3089276844435,-1.23102926805979,
-1.19688793436548,-1.17004272418587,-1.08368837154726,-1.04606737005723,
-1.01553569577731,-0.997334018908637,-0.903275019134099,-0.840846379666836,
-0.792075216486473,-0.767723818900745,-0.674993002634844,-0.591861111789487,
-0.5418904765301,-0.513413625146155,-0.415103169643614,-0.342465439253416,
-0.295139212184705,-0.267683438959337,-0.246657340266153,-0.14734376022256,
-0.0476021992245664,0.),.UNSPECIFIED.);
#657=B_SPLINE_CURVE_WITH_KNOTS('',3,(#38760,#38761,#38762,#38763,#38764,
#38765,#38766,#38767,#38768,#38769,#38770,#38771,#38772,#38773),
 .UNSPECIFIED.,.F.,.F.,(4,1,1,1,1,1,1,1,1,1,1,4),(10.3764180272042,10.8022839504821,
11.3017289099287,11.8011738693754,12.3006188288221,12.8000637882687,13.2995087477154,
13.7989537071621,14.2983986666087,14.7978436260554,15.297288585502,15.7079632679489),
 .UNSPECIFIED.);
#658=B_SPLINE_CURVE_WITH_KNOTS('',3,(#38777,#38778,#38779,#38780,#38781,
#38782,#38783,#38784,#38785,#38786,#38787,#38788),.UNSPECIFIED.,.F.,.F.,
(4,1,1,1,1,1,1,1,1,4),(11.6147305479243,12.1141755073709,12.6136204668176,
13.1130654262643,13.6125103857109,14.1119553451576,14.6114003046042,15.1108452640509,
15.6102902234976,15.7079632679489),.UNSPECIFIED.);
#659=B_SPLINE_CURVE_WITH_KNOTS('',3,(#39169,#39170,#39171,#39172,#39173,
#39174,#39175,#39176,#39177,#39178,#39179,#39180,#39181,#39182,#39183,#39184,
#39185,#39186,#39187,#39188,#39189,#39190,#39191,#39192,#39193,#39194,#39195,
#39196,#39197,#39198,#39199,#39200,#39201,#39202,#39203,#39204,#39205,#39206,
#39207,#39208,#39209,#39210,#39211,#39212,#39213,#39214,#39215,#39216,#39217,
#39218,#39219,#39220,#39221,#39222,#39223,#39224,#39225,#39226,#39227,#39228,
#39229,#39230,#39231,#39232,#39233,#39234,#39235,#39236,#39237,#39238,#39239,
#39240,#39241),.UNSPECIFIED.,.F.,.F.,(4,3,3,3,3,3,3,3,3,3,3,3,3,3,3,3,3,
3,3,3,3,3,3,3,4),(-1.35019749972372,-1.29933842216204,-1.2144517529809,
-1.1799649098461,-1.15395803765335,-1.05687489154542,-0.995259377759728,
-0.973262384530162,-0.959791745437486,-0.862294124972048,-0.765591977626827,
-0.740849464395243,-0.722135242327674,-0.629748770541223,-0.549747247506988,
-0.5047603153859,-0.483247294935022,-0.389544230430759,-0.309742678404285,
-0.263847165242411,-0.242838634274085,-0.223579987122219,-0.131367108976752,
-0.0408082650079221,0.),.UNSPECIFIED.);
#660=B_SPLINE_CURVE_WITH_KNOTS('',3,(#39242,#39243,#39244,#39245,#39246,
#39247,#39248,#39249,#39250,#39251,#39252,#39253,#39254,#39255,#39256,#39257,
#39258,#39259,#39260,#39261,#39262,#39263,#39264,#39265,#39266,#39267,#39268,
#39269),.UNSPECIFIED.,.F.,.F.,(4,3,3,3,3,3,3,3,3,4),(-45.9489362690929,
-45.4494913096462,-44.9500463501996,-44.4506013907529,-43.9511564313063,
-43.4517114718596,-42.9522665124129,-42.4528215529663,-41.9533765935196,
-41.7923445631022),.UNSPECIFIED.);
#661=B_SPLINE_CURVE_WITH_KNOTS('',3,(#39589,#39590,#39591,#39592,#39593,
#39594,#39595,#39596),.UNSPECIFIED.,.F.,.F.,(4,2,2,4),(0.,0.237315706087857,
0.388427486543153,0.517252919461271),.UNSPECIFIED.);
#662=B_SPLINE_CURVE_WITH_KNOTS('',3,(#39598,#39599,#39600,#39601,#39602,
#39603,#39604,#39605,#39606,#39607,#39608,#39609,#39610,#39611,#39612,#39613,
#39614,#39615,#39616,#39617,#39618,#39619,#39620,#39621,#39622,#39623,#39624,
#39625,#39626,#39627,#39628,#39629,#39630,#39631,#39632,#39633,#39634,#39635,
#39636,#39637,#39638,#39639,#39640,#39641,#39642,#39643,#39644,#39645,#39646,
#39647,#39648,#39649,#39650,#39651,#39652,#39653,#39654,#39655,#39656,#39657,
#39658,#39659,#39660,#39661,#39662,#39663,#39664,#39665,#39666,#39667,#39668,
#39669,#39670,#39671,#39672,#39673,#39674,#39675,#39676,#39677,#39678,#39679,
#39680,#39681,#39682,#39683,#39684,#39685,#39686,#39687,#39688,#39689,#39690,
#39691,#39692,#39693,#39694,#39695,#39696,#39697,#39698,#39699,#39700,#39701,
#39702,#39703,#39704,#39705,#39706,#39707,#39708,#39709,#39710,#39711,#39712,
#39713,#39714,#39715,#39716,#39717,#39718,#39719,#39720,#39721,#39722,#39723,
#39724,#39725,#39726,#39727,#39728,#39729,#39730,#39731,#39732,#39733,#39734,
#39735,#39736,#39737,#39738,#39739,#39740,#39741,#39742,#39743,#39744,#39745,
#39746,#39747,#39748,#39749,#39750,#39751,#39752,#39753,#39754,#39755,#39756,
#39757,#39758,#39759,#39760,#39761,#39762,#39763,#39764,#39765,#39766,#39767,
#39768,#39769,#39770,#39771,#39772,#39773,#39774,#39775),.UNSPECIFIED.,
 .F.,.F.,(4,3,3,3,3,3,3,3,3,3,3,3,3,3,3,3,3,3,3,3,3,3,3,3,3,3,3,3,3,3,3,
3,3,3,3,3,3,3,3,3,3,3,3,3,3,3,3,3,3,3,3,3,3,3,3,3,3,3,3,4),(0.,0.487649323312794,
0.975298646625587,1.46294796993838,1.95059729325117,2.43824661656396,2.92589593987676,
3.41354526318955,3.90119458650234,4.38884390981513,4.87649323312793,5.36414255644072,
5.85179187975351,6.33944120306631,6.8270905263791,7.31473984969189,7.80238917300469,
8.29003849631748,8.77768781963027,9.26533714294306,9.75298646625586,10.2406357895687,
10.7282851128814,11.2159344361942,11.703583759507,12.1912330828198,12.6788824061326,
13.1665317294454,13.6541810527582,14.141830376071,14.6294796993838,15.1171290226966,
15.6047783460094,16.0924276693222,16.580076992635,17.0677263159478,17.5553756392605,
18.0430249625733,18.5306742858861,19.0183236091989,19.5059729325117,19.9936222558245,
20.4812715791373,20.9689209024501,21.4565702257629,21.9442195490757,22.4318688723885,
22.9195181957013,23.4071675190141,23.8948168423269,24.3824661656396,24.8701154889524,
25.3577648122652,25.845414135578,26.3330634588908,26.8207127822036,27.3083621055164,
27.7960114288292,28.283660752142,28.493874313809),.UNSPECIFIED.);
#663=B_SPLINE_CURVE_WITH_KNOTS('',3,(#39777,#39778,#39779,#39780,#39781,
#39782,#39783,#39784),.UNSPECIFIED.,.F.,.F.,(4,2,2,4),(-0.517251340629339,
-0.388433724430474,-0.237311387866167,0.),.UNSPECIFIED.);
#664=B_SPLINE_CURVE_WITH_KNOTS('',3,(#39785,#39786,#39787,#39788,#39789,
#39790,#39791,#39792,#39793,#39794,#39795,#39796,#39797,#39798,#39799,#39800,
#39801,#39802,#39803,#39804,#39805,#39806,#39807,#39808,#39809,#39810,#39811,
#39812,#39813,#39814,#39815,#39816,#39817,#39818,#39819,#39820,#39821,#39822,
#39823,#39824,#39825,#39826,#39827,#39828,#39829,#39830,#39831,#39832,#39833,
#39834,#39835,#39836,#39837,#39838,#39839,#39840,#39841,#39842,#39843,#39844,
#39845,#39846),.UNSPECIFIED.,.F.,.F.,(4,1,1,1,1,1,1,1,1,1,1,1,1,1,1,1,1,
1,1,1,1,1,1,1,1,1,1,1,1,1,1,1,1,1,1,1,1,1,1,1,1,1,1,1,1,1,1,1,1,1,1,1,1,
1,1,1,1,1,1,4),(7.04827039213818,7.25848395380519,7.74613327711798,8.23378260043077,
8.72143192374356,9.20908124705636,9.69673057036915,10.1843798936819,10.6720292169947,
11.1596785403075,11.6473278636203,12.1349771869331,12.6226265102459,13.1102758335587,
13.5979251568715,14.0855744801843,14.5732238034971,15.0608731268099,15.5485224501227,
16.0361717734355,16.5238210967483,17.011470420061,17.4991197433738,17.9867690666866,
18.4744183899994,18.9620677133122,19.449717036625,19.9373663599378,20.4250156832506,
20.9126650065634,21.4003143298762,21.887963653189,22.3756129765018,22.8632622998146,
23.3509116231274,23.8385609464401,24.3262102697529,24.8138595930657,25.3015089163785,
25.7891582396913,26.2768075630041,26.7644568863169,27.2521062096297,27.7397555329425,
28.2274048562553,28.7150541795681,29.2027035028809,29.6903528261937,30.1780021495065,
30.6656514728192,31.153300796132,31.6409501194448,32.1285994427576,32.6162487660704,
33.1038980893832,33.591547412696,34.0791967360088,34.5668460593216,35.0544953826344,
35.5421447059472),.UNSPECIFIED.);
#665=B_SPLINE_CURVE_WITH_KNOTS('',3,(#40100,#40101,#40102,#40103,#40104,
#40105,#40106,#40107,#40108,#40109,#40110,#40111,#40112,#40113,#40114,#40115,
#40116,#40117,#40118,#40119,#40120,#40121,#40122,#40123,#40124,#40125,#40126,
#40127,#40128,#40129,#40130,#40131,#40132,#40133,#40134,#40135,#40136,#40137,
#40138,#40139,#40140,#40141,#40142,#40143,#40144,#40145),.UNSPECIFIED.,
 .F.,.F.,(4,3,3,3,3,3,3,3,3,3,3,3,3,3,3,4),(0.,0.0942991010737542,0.193262215210111,
0.237548070776078,0.261597840086782,0.292225329346469,0.384931640470592,
0.454115017893606,0.485075070504274,0.504919783104731,0.600066451276272,
0.674462382718296,0.696928463272835,0.786359577028978,0.874195006668787,
0.897650177044366),.UNSPECIFIED.);
#666=B_SPLINE_CURVE_WITH_KNOTS('',3,(#40147,#40148,#40149,#40150,#40151,
#40152,#40153,#40154,#40155,#40156,#40157,#40158,#40159,#40160,#40161,#40162,
#40163,#40164,#40165,#40166,#40167,#40168,#40169,#40170,#40171,#40172,#40173,
#40174,#40175,#40176,#40177,#40178,#40179,#40180,#40181,#40182,#40183,#40184,
#40185,#40186,#40187,#40188,#40189,#40190,#40191,#40192,#40193,#40194,#40195),
 .UNSPECIFIED.,.F.,.F.,(4,3,3,3,3,3,3,3,3,3,3,3,3,3,3,3,4),(-0.897650177044365,
-0.809221996292059,-0.716620361820245,-0.696324645029017,-0.674917979597778,
-0.624018727348431,-0.547256284732747,-0.495744435273601,-0.47451926273118,
-0.381889608747681,-0.316968956885692,-0.2713446547458,-0.249438014013973,
-0.22789468603582,-0.134228551311836,-0.0401158448815296,0.),
 .UNSPECIFIED.);
#667=B_SPLINE_CURVE_WITH_KNOTS('',3,(#40196,#40197,#40198,#40199,#40200,
#40201,#40202,#40203,#40204,#40205,#40206,#40207,#40208,#40209,#40210,#40211,
#40212,#40213,#40214,#40215,#40216,#40217,#40218,#40219,#40220,#40221,#40222,
#40223,#40224,#40225,#40226,#40227,#40228,#40229,#40230,#40231,#40232,#40233,
#40234,#40235,#40236,#40237,#40238,#40239,#40240,#40241,#40242,#40243,#40244,
#40245,#40246,#40247,#40248,#40249,#40250,#40251,#40252,#40253,#40254,#40255,
#40256),.UNSPECIFIED.,.F.,.F.,(4,1,1,1,1,1,1,1,1,1,1,1,1,1,1,1,1,1,1,1,
1,1,1,1,1,1,1,1,1,1,1,1,1,1,1,1,1,1,1,1,1,1,1,1,1,1,1,1,1,1,1,1,1,1,1,1,
1,1,4),(8.50634549793098,8.54586786311827,9.04506702011163,9.54426617710499,
10.0434653340984,10.5426644910917,11.0418636480851,11.5410628050784,12.0402619620718,
12.5394611190652,13.0386602760585,13.5378594330519,14.0370585900453,14.5362577470386,
15.035456904032,15.5346560610254,16.0338552180187,16.5330543750121,17.0322535320054,
17.5314526889988,18.0306518459922,18.5298510029855,19.0290501599789,19.5282493169723,
20.0274484739656,20.526647630959,21.0258467879524,21.5250459449457,22.0242451019391,
22.5234442589325,23.0226434159258,23.5218425729192,24.0210417299125,24.5202408869059,
25.0194400438993,25.5186392008926,26.017838357886,26.5170375148794,27.0162366718727,
27.5154358288661,28.0146349858595,28.5138341428528,29.0130332998462,29.5122324568395,
30.0114316138329,30.5106307708263,31.0098299278196,31.509029084813,32.0082282418064,
32.5074273987997,33.0066265557931,33.5058257127865,34.0050248697798,34.5042240267732,
35.0034231837665,35.5026223407599,36.0018214977533,36.5010206547466,37.00021981174),
 .UNSPECIFIED.);
#668=B_SPLINE_CURVE_WITH_KNOTS('',3,(#40572,#40573,#40574,#40575,#40576,
#40577,#40578,#40579),.UNSPECIFIED.,.F.,.F.,(4,2,2,4),(0.,0.129325009251138,
0.19845452791459,0.272929378090483),.UNSPECIFIED.);
#669=B_SPLINE_CURVE_WITH_KNOTS('',3,(#40581,#40582,#40583,#40584,#40585,
#40586,#40587,#40588),.UNSPECIFIED.,.F.,.F.,(4,2,2,4),(-0.272903900599443,
-0.198454240786918,-0.129349013127501,0.),.UNSPECIFIED.);
#670=B_SPLINE_CURVE_WITH_KNOTS('',3,(#40589,#40590,#40591,#40592),
 .UNSPECIFIED.,.F.,.F.,(4,4),(9.27143058288956,9.42477796076937),
 .UNSPECIFIED.);
#671=B_SPLINE_CURVE_WITH_KNOTS('',3,(#40598,#40599,#40600,#40601,#40602,
#40603,#40604,#40605),.UNSPECIFIED.,.F.,.F.,(4,2,2,4),(-0.322073238962409,
-0.232715827739448,-0.150125558909819,0.),.UNSPECIFIED.);
#672=B_SPLINE_CURVE_WITH_KNOTS('',3,(#40607,#40608,#40609,#40610,#40611,
#40612,#40613,#40614,#40615,#40616,#40617,#40618,#40619,#40620,#40621,#40622,
#40623,#40624,#40625,#40626,#40627,#40628,#40629,#40630,#40631,#40632,#40633,
#40634,#40635,#40636,#40637,#40638,#40639,#40640,#40641,#40642,#40643,#40644,
#40645,#40646,#40647,#40648,#40649,#40650,#40651,#40652,#40653,#40654,#40655),
 .UNSPECIFIED.,.F.,.F.,(4,3,3,3,3,3,3,3,3,3,3,3,3,3,3,3,4),(-0.89585384003955,
-0.801561846631882,-0.702966153173172,-0.678976633753644,-0.657477299216225,
-0.604370459714462,-0.527568764985274,-0.481321993461353,-0.451377108901128,
-0.36059738503407,-0.297163680797711,-0.25214599148876,-0.230319865611295,
-0.210822177973724,-0.121429520577694,-0.0337496836487225,0.),
 .UNSPECIFIED.);
#673=B_SPLINE_CURVE_WITH_KNOTS('',3,(#40656,#40657,#40658,#40659,#40660,
#40661),.UNSPECIFIED.,.F.,.F.,(4,2,4),(-0.500559801427663,-0.225408038500461,
0.),.UNSPECIFIED.);
#674=B_SPLINE_CURVE_WITH_KNOTS('',3,(#40980,#40981,#40982,#40983,#40984,
#40985),.UNSPECIFIED.,.F.,.F.,(4,2,4),(0.,0.225412734088363,0.500557798157366),
 .UNSPECIFIED.);
#675=B_SPLINE_CURVE_WITH_KNOTS('',3,(#40986,#40987,#40988,#40989,#40990,
#40991,#40992,#40993,#40994,#40995,#40996,#40997,#40998,#40999,#41000,#41001,
#41002,#41003,#41004,#41005,#41006,#41007,#41008,#41009,#41010,#41011,#41012,
#41013,#41014,#41015,#41016,#41017,#41018,#41019,#41020,#41021,#41022,#41023,
#41024,#41025,#41026,#41027,#41028,#41029,#41030,#41031,#41032,#41033,#41034,
#41035,#41036,#41037,#41038,#41039,#41040,#41041,#41042,#41043,#41044,#41045,
#41046,#41047),.UNSPECIFIED.,.F.,.F.,(4,1,1,1,1,1,1,1,1,1,1,1,1,1,1,1,1,
1,1,1,1,1,1,1,1,1,1,1,1,1,1,1,1,1,1,1,1,1,1,1,1,1,1,1,1,1,1,1,1,1,1,1,1,
1,1,1,1,1,1,4),(10.3432104236078,10.5534239852748,11.0410733085876,11.5287226319004,
12.0163719552132,12.504021278526,12.9916706018388,13.4793199251516,13.9669692484644,
14.4546185717772,14.94226789509,15.4299172184027,15.9175665417155,16.4052158650283,
16.8928651883411,17.3805145116539,17.8681638349667,18.3558131582795,18.8434624815923,
19.3311118049051,19.8187611282179,20.3064104515307,20.7940597748435,21.2817090981563,
21.7693584214691,22.2570077447818,22.7446570680946,23.2323063914074,23.7199557147202,
24.207605038033,24.6952543613458,25.1829036846586,25.6705530079714,26.1582023312842,
26.645851654597,27.1335009779098,27.6211503012226,28.1087996245354,28.5964489478482,
29.0840982711609,29.5717475944737,30.0593969177865,30.5470462410993,31.0346955644121,
31.5223448877249,32.0099942110377,32.4976435343505,32.9852928576633,33.4729421809761,
33.9605915042889,34.4482408276017,34.9358901509145,35.4235394742273,35.91118879754,
36.3988381208528,36.8864874441656,37.3741367674784,37.8617860907912,38.349435414104,
38.8370847374168),.UNSPECIFIED.);
#676=B_SPLINE_CURVE_WITH_KNOTS('',3,(#41301,#41302,#41303,#41304,#41305,
#41306,#41307,#41308,#41309,#41310,#41311,#41312,#41313,#41314,#41315,#41316,
#41317,#41318,#41319,#41320,#41321,#41322,#41323,#41324,#41325,#41326,#41327,
#41328,#41329,#41330,#41331,#41332,#41333,#41334,#41335,#41336,#41337,#41338,
#41339,#41340,#41341,#41342,#41343,#41344,#41345,#41346,#41347,#41348,#41349),
 .UNSPECIFIED.,.F.,.F.,(4,3,3,3,3,3,3,3,3,3,3,3,3,3,3,3,4),(0.,0.0881387442926152,
0.180700997921297,0.22591832279636,0.243527785554388,0.27326325154998,0.36378372577003,
0.424829269926009,0.460795635173694,0.480982236187546,0.57372100351339,
0.579674857270561,0.658719602962808,0.681251247199192,0.774812612388552,
0.868884434159813,0.895853840039549),.UNSPECIFIED.);
#677=B_SPLINE_CURVE_WITH_KNOTS('',3,(#41350,#41351,#41352,#41353,#41354,
#41355,#41356,#41357,#41358,#41359,#41360,#41361,#41362,#41363,#41364,#41365,
#41366,#41367,#41368,#41369,#41370,#41371,#41372,#41373,#41374,#41375,#41376,
#41377,#41378,#41379,#41380,#41381,#41382,#41383,#41384,#41385,#41386,#41387,
#41388,#41389,#41390,#41391,#41392,#41393,#41394,#41395,#41396,#41397,#41398,
#41399,#41400,#41401,#41402,#41403,#41404,#41405,#41406,#41407,#41408,#41409,
#41410),.UNSPECIFIED.,.F.,.F.,(4,1,1,1,1,1,1,1,1,1,1,1,1,1,1,1,1,1,1,1,
1,1,1,1,1,1,1,1,1,1,1,1,1,1,1,1,1,1,1,1,1,1,1,1,1,1,1,1,1,1,1,1,1,1,1,1,
1,1,4),(11.8012855294006,11.8408078945879,12.3400070515813,12.8392062085746,
13.338405365568,13.8376045225613,14.3368036795547,14.8360028365481,15.3352019935414,
15.8344011505348,16.3336003075282,16.8327994645215,17.3319986215149,17.8311977785083,
18.3303969355016,18.829596092495,19.3287952494883,19.8279944064817,20.3271935634751,
20.8263927204684,21.3255918774618,21.8247910344552,22.3239901914485,22.8231893484419,
23.3223885054353,23.8215876624286,24.320786819422,24.8199859764153,25.3191851334087,
25.8183842904021,26.3175834473954,26.8167826043888,27.3159817613822,27.8151809183755,
28.3143800753689,28.8135792323623,29.3127783893556,29.811977546349,30.3111767033423,
30.8103758603357,31.3095750173291,31.8087741743224,32.3079733313158,32.8071724883092,
33.3063716453025,33.8055708022959,34.3047699592893,34.8039691162826,35.303168273276,
35.8023674302693,36.3015665872627,36.8007657442561,37.2999649012494,37.7991640582428,
38.2983632152362,38.7975623722295,39.2967615292229,39.7959606862163,40.2951598432096),
 .UNSPECIFIED.);
#678=B_SPLINE_CURVE_WITH_KNOTS('',3,(#41726,#41727,#41728,#41729,#41730,
#41731,#41732,#41733),.UNSPECIFIED.,.F.,.F.,(4,2,2,4),(0.,0.150083807667359,
0.232692116568135,0.322068030175859),.UNSPECIFIED.);
#679=B_SPLINE_CURVE_WITH_KNOTS('',3,(#41868,#41869,#41870,#41871,#41872,
#41873,#41874,#41875,#41876,#41877,#41878,#41879,#41880,#41881,#41882,#41883,
#41884,#41885),.UNSPECIFIED.,.F.,.F.,(4,2,2,2,2,2,2,2,4),(-0.909033920514541,
-0.795393296746547,-0.681752672978553,-0.568134816617911,-0.45451696025727,
-0.340899103896629,-0.227281247535988,-0.113640623767994,0.),
 .UNSPECIFIED.);
#680=B_SPLINE_CURVE_WITH_KNOTS('',3,(#41896,#41897,#41898,#41899,#41900,
#41901,#41902,#41903,#41904,#41905,#41906,#41907,#41908,#41909,#41910,#41911,
#41912,#41913),.UNSPECIFIED.,.F.,.F.,(4,2,2,2,2,2,2,2,4),(0.,0.113640623767995,
0.22728124753599,0.34089910389663,0.454516960257271,0.568134816617911,0.681752672978552,
0.795393296746547,0.909033920514541),.UNSPECIFIED.);
#681=B_SPLINE_CURVE_WITH_KNOTS('',3,(#41927,#41928,#41929,#41930,#41931,
#41932,#41933,#41934,#41935,#41936,#41937,#41938,#41939,#41940,#41941,#41942,
#41943,#41944),.UNSPECIFIED.,.F.,.F.,(4,2,2,2,2,2,2,2,4),(-1.21468374386295,
-1.06281862619298,-0.910953508522999,-0.759147690227238,-0.607341871931477,
-0.455536053635716,-0.303730235339955,-0.151865117669978,0.),
 .UNSPECIFIED.);
#682=B_SPLINE_CURVE_WITH_KNOTS('',3,(#41955,#41956,#41957,#41958,#41959,
#41960,#41961,#41962,#41963,#41964,#41965,#41966,#41967,#41968,#41969,#41970,
#41971,#41972),.UNSPECIFIED.,.F.,.F.,(4,2,2,2,2,2,2,2,4),(0.,0.151865117669977,
0.303730235339955,0.455536053635716,0.607341871931477,0.759147690227237,
0.910953508522998,1.06281862619298,1.21468374386295),.UNSPECIFIED.);
#683=B_SPLINE_CURVE_WITH_KNOTS('',3,(#42129,#42130,#42131,#42132,#42133,
#42134),.UNSPECIFIED.,.F.,.F.,(4,2,4),(1.68069680516896,1.71912851411125,
1.75756022305355),.UNSPECIFIED.);
#684=B_SPLINE_CURVE_WITH_KNOTS('',3,(#42145,#42146,#42147,#42148,#42149,
#42150),.UNSPECIFIED.,.F.,.F.,(4,2,4),(1.68069680516896,1.71912851411125,
1.75756022305355),.UNSPECIFIED.);
#685=B_SPLINE_CURVE_WITH_KNOTS('',3,(#42161,#42162,#42163,#42164,#42165,
#42166),.UNSPECIFIED.,.F.,.F.,(4,2,4),(1.68069680516896,1.71912851411125,
1.75756022305355),.UNSPECIFIED.);
#686=B_SPLINE_CURVE_WITH_KNOTS('',3,(#42177,#42178,#42179,#42180,#42181,
#42182),.UNSPECIFIED.,.F.,.F.,(4,2,4),(1.68069680516896,1.71912851411125,
1.75756022305355),.UNSPECIFIED.);
#687=B_SPLINE_CURVE_WITH_KNOTS('',3,(#42193,#42194,#42195,#42196,#42197,
#42198),.UNSPECIFIED.,.F.,.F.,(4,2,4),(1.68069680516897,1.71912851411125,
1.75756022305354),.UNSPECIFIED.);
#688=B_SPLINE_CURVE_WITH_KNOTS('',3,(#42209,#42210,#42211,#42212,#42213,
#42214),.UNSPECIFIED.,.F.,.F.,(4,2,4),(1.68069680516896,1.71912851411125,
1.75756022305355),.UNSPECIFIED.);
#689=B_SPLINE_CURVE_WITH_KNOTS('',3,(#42225,#42226,#42227,#42228,#42229,
#42230),.UNSPECIFIED.,.F.,.F.,(4,2,4),(1.68069680516896,1.71912851411125,
1.75756022305355),.UNSPECIFIED.);
#690=B_SPLINE_CURVE_WITH_KNOTS('',3,(#42241,#42242,#42243,#42244,#42245,
#42246),.UNSPECIFIED.,.F.,.F.,(4,2,4),(1.68069680516896,1.71912851411125,
1.75756022305355),.UNSPECIFIED.);
#691=B_SPLINE_CURVE_WITH_KNOTS('',3,(#42257,#42258,#42259,#42260,#42261,
#42262),.UNSPECIFIED.,.F.,.F.,(4,2,4),(1.68069680516896,1.71912851411125,
1.75756022305355),.UNSPECIFIED.);
#692=B_SPLINE_CURVE_WITH_KNOTS('',3,(#42442,#42443,#42444,#42445,#42446,
#42447,#42448,#42449,#42450,#42451,#42452,#42453,#42454,#42455,#42456,#42457),
 .UNSPECIFIED.,.F.,.F.,(4,2,2,2,2,2,2,4),(-0.827444006878981,-0.709137715093229,
-0.606258454477036,-0.552969769025734,-0.51054365769559,-0.463186805002842,
-0.385864633040324,-0.216479568668788),.UNSPECIFIED.);
#693=B_SPLINE_CURVE_WITH_KNOTS('',3,(#42466,#42467,#42468,#42469,#42470,
#42471,#42472,#42473,#42474,#42475),.UNSPECIFIED.,.F.,.F.,(4,2,2,2,4),(-0.52479568404363,
-0.512334893121172,-0.461457866065132,-0.380752711923638,-0.216468504749557),
 .UNSPECIFIED.);
#694=B_SPLINE_CURVE_WITH_KNOTS('',3,(#42479,#42480,#42481,#42482,#42483,
#42484,#42485,#42486,#42487,#42488,#42489,#42490,#42491,#42492,#42493,#42494),
 .UNSPECIFIED.,.F.,.F.,(4,2,2,2,2,2,2,4),(-0.827444006877975,-0.709137715092587,
-0.606258454476783,-0.552969769025578,-0.510543657695527,-0.463186805002854,
-0.385864633040295,-0.216479568668763),.UNSPECIFIED.);
#695=B_SPLINE_CURVE_WITH_KNOTS('',3,(#42498,#42499,#42500,#42501,#42502,
#42503,#42504,#42505,#42506,#42507,#42508,#42509,#42510,#42511,#42512,#42513),
 .UNSPECIFIED.,.F.,.F.,(4,2,2,2,2,2,2,4),(-0.827444006878145,-0.709137715092748,
-0.606258454476905,-0.552969769025703,-0.510543657695638,-0.463186805002939,
-0.385864633040348,-0.21647956866881),.UNSPECIFIED.);
#696=B_SPLINE_CURVE_WITH_KNOTS('',3,(#42517,#42518,#42519,#42520,#42521,
#42522,#42523,#42524,#42525,#42526),.UNSPECIFIED.,.F.,.F.,(4,2,2,2,4),(-0.828799355587065,
-0.7357048796955,-0.618324369294947,-0.558811967132771,-0.524795684044317),
 .UNSPECIFIED.);
#697=B_SPLINE_CURVE_WITH_KNOTS('',3,(#42528,#42529,#42530,#42531,#42532,
#42533,#42534,#42535,#42536,#42537),.UNSPECIFIED.,.F.,.F.,(4,2,2,2,4),(-0.524795684044317,
-0.512334893121834,-0.461457866065708,-0.380752711924124,-0.216468504749763),
 .UNSPECIFIED.);
#698=B_SPLINE_CURVE_WITH_KNOTS('',3,(#42542,#42543,#42544,#42545,#42546,
#42547,#42548,#42549,#42550,#42551,#42552,#42553,#42554,#42555,#42556,#42557),
 .UNSPECIFIED.,.F.,.F.,(4,2,2,2,2,2,2,4),(-0.827444006877793,-0.709137715092454,
-0.606258454476639,-0.552969769025454,-0.510543657695402,-0.463186805002724,
-0.385864633040191,-0.216479568668727),.UNSPECIFIED.);
#699=B_SPLINE_CURVE_WITH_KNOTS('',3,(#42560,#42561,#42562,#42563,#42564,
#42565,#42566,#42567,#42568,#42569),.UNSPECIFIED.,.F.,.F.,(4,2,2,2,4),(-0.828799355585381,
-0.735704879694107,-0.618324369293949,-0.558811967131987,-0.52479568404363),
 .UNSPECIFIED.);
#700=B_SPLINE_CURVE_WITH_KNOTS('',3,(#42606,#42607,#42608,#42609,#42610,
#42611,#42612,#42613,#42614,#42615),.UNSPECIFIED.,.F.,.F.,(4,2,2,2,4),(0.,
0.250118116648096,0.500236233296193,0.750349479868711,1.00046272644123),
 .UNSPECIFIED.);
#701=B_SPLINE_CURVE_WITH_KNOTS('',3,(#42616,#42617,#42618,#42619,#42620,
#42621,#42622,#42623,#42624,#42625,#42626,#42627,#42628,#42629,#42630,#42631,
#42632,#42633,#42634,#42635,#42636,#42637,#42638,#42639,#42640,#42641),
 .UNSPECIFIED.,.F.,.F.,(4,2,2,2,2,2,2,2,2,2,2,2,4),(1.00046272644123,1.25057597301375,
1.50068921958627,1.75080733623436,2.00092545288246,2.25104356953056,2.50116168617865,
2.75127493275117,3.00138817932369,3.25150142589621,3.50161467246873,3.75173278911682,
4.00185090576492),.UNSPECIFIED.);
#702=B_SPLINE_CURVE_WITH_KNOTS('',3,(#42653,#42654,#42655,#42656,#42657,
#42658,#42659,#42660,#42661,#42662,#42663,#42664,#42665,#42666,#42667,#42668,
#42669,#42670,#42671,#42672,#42673,#42674,#42675,#42676,#42677,#42678),
 .UNSPECIFIED.,.F.,.F.,(4,2,2,2,2,2,2,2,2,2,2,2,4),(0.,0.492179153056542,
0.984358306113084,1.47645655199157,1.96855479787006,2.46065304374855,2.95275128962704,
3.44493044268358,3.93710959574012,4.42928874879666,4.92146790185321,5.41356614773169,
5.90566439361018),.UNSPECIFIED.);
#703=B_SPLINE_CURVE_WITH_KNOTS('',3,(#42679,#42680,#42681,#42682,#42683,
#42684,#42685,#42686,#42687,#42688),.UNSPECIFIED.,.F.,.F.,(4,2,2,2,4),(5.90566439361018,
6.39776263948867,6.88986088536716,7.3820400384237,7.87421919148024),
 .UNSPECIFIED.);
#704=B_SPLINE_CURVE_WITH_KNOTS('',3,(#42904,#42905,#42906,#42907,#42908,
#42909,#42910,#42911,#42912,#42913,#42914,#42915,#42916,#42917,#42918,#42919,
#42920,#42921),.UNSPECIFIED.,.F.,.F.,(4,2,2,2,2,2,2,2,4),(0.,0.115474560264442,
0.230949120528883,0.346108891526704,0.461268662524524,0.576428433522344,
0.691588204520164,0.807062764784606,0.922537325049047),.UNSPECIFIED.);
#705=B_SPLINE_CURVE_WITH_KNOTS('',3,(#42922,#42923,#42924,#42925,#42926,
#42927,#42928,#42929,#42930,#42931,#42932,#42933,#42934,#42935,#42936,#42937,
#42938,#42939),.UNSPECIFIED.,.F.,.F.,(4,2,2,2,2,2,2,2,4),(0.922537325049047,
1.03801188531349,1.15348644557793,1.26864621657575,1.38380598757357,1.49896575857139,
1.61412552956921,1.72960008983365,1.84507465009809),.UNSPECIFIED.);
#706=B_SPLINE_CURVE_WITH_KNOTS('',3,(#43005,#43006,#43007,#43008,#43009,
#43010,#43011,#43012,#43013,#43014),.UNSPECIFIED.,.F.,.F.,(4,2,2,2,4),(0.196434861767707,
0.226700589297083,0.453401178594166,0.680088163565136,0.906775148536106),
 .UNSPECIFIED.);
#707=B_SPLINE_CURVE_WITH_KNOTS('',3,(#43021,#43022,#43023,#43024,#43025,
#43026,#43027,#43028,#43029,#43030),.UNSPECIFIED.,.F.,.F.,(4,2,2,2,4),(0.906775148536106,
1.13346213350708,1.36014911847805,1.58684970777513,1.61711543530451),
 .UNSPECIFIED.);
#708=B_SPLINE_CURVE_WITH_KNOTS('',3,(#43034,#43035,#43036,#43037,#43038,
#43039,#43040,#43041,#43042,#43043,#43044,#43045,#43046,#43047),
 .UNSPECIFIED.,.F.,.F.,(4,2,2,2,2,2,4),(2.20122847938268,2.27205851753461,
2.49923948385036,2.72642045016611,2.95360141648186,3.18078238279761,3.25161242094954),
 .UNSPECIFIED.);
#709=B_SPLINE_CURVE_WITH_KNOTS('',3,(#43054,#43055,#43056,#43057,#43058,
#43059),.UNSPECIFIED.,.F.,.F.,(4,2,4),(0.193270693145506,0.23055183180291,
0.366122014076097),.UNSPECIFIED.);
#710=B_SPLINE_CURVE_WITH_KNOTS('',3,(#43067,#43068,#43069,#43070,#43071,
#43072),.UNSPECIFIED.,.F.,.F.,(4,2,4),(1.5242057805381,1.65977596281129,
1.69705710146869),.UNSPECIFIED.);
#711=B_SPLINE_CURVE_WITH_KNOTS('',3,(#43096,#43097,#43098,#43099,#43100,
#43101,#43102,#43103,#43104,#43105),.UNSPECIFIED.,.F.,.F.,(4,2,2,2,4),(2.72032544560832,
2.94701243057929,3.17369941555026,3.40040000484734,3.43066573237672),
 .UNSPECIFIED.);
#712=B_SPLINE_CURVE_WITH_KNOTS('',3,(#43110,#43111,#43112,#43113,#43114,
#43115,#43116,#43117,#43118,#43119),.UNSPECIFIED.,.F.,.F.,(4,2,2,2,4),(2.00998515883992,
2.0402508863693,2.26695147566638,2.49363846063735,2.72032544560832),
 .UNSPECIFIED.);
#713=B_SPLINE_CURVE_WITH_KNOTS('',3,(#43126,#43127,#43128,#43129,#43130,
#43131,#43132,#43133,#43134,#43135,#43136,#43137,#43138,#43139),
 .UNSPECIFIED.,.F.,.F.,(4,2,2,2,2,2,4),(0.383614845938606,0.454444884090536,
0.681625850406286,0.908806816722037,1.13598778303779,1.36316874935354,1.43399878750547),
 .UNSPECIFIED.);
#714=B_SPLINE_CURVE_WITH_KNOTS('',3,(#43147,#43148,#43149,#43150,#43151,
#43152),.UNSPECIFIED.,.F.,.F.,(4,2,4),(2.08359848775971,2.12087962641711,
2.2564498086903),.UNSPECIFIED.);
#715=B_SPLINE_CURVE_WITH_KNOTS('',3,(#43160,#43161,#43162,#43163,#43164,
#43165),.UNSPECIFIED.,.F.,.F.,(4,2,4),(3.4145335751523,3.55010375742549,
3.5873848960829),.UNSPECIFIED.);
#716=B_SPLINE_CURVE_WITH_KNOTS('',2,(#43224,#43225,#43226),
 .UNSPECIFIED.,.F.,.F.,(3,3),(0.,1.),.UNSPECIFIED.);
#717=B_SPLINE_CURVE_WITH_KNOTS('',2,(#43230,#43231,#43232),
 .UNSPECIFIED.,.F.,.F.,(3,3),(0.,1.),.UNSPECIFIED.);
#718=B_SPLINE_CURVE_WITH_KNOTS('',2,(#43241,#43242,#43243),
 .UNSPECIFIED.,.F.,.F.,(3,3),(0.,1.),.UNSPECIFIED.);
#719=B_SPLINE_CURVE_WITH_KNOTS('',2,(#43246,#43247,#43248),
 .UNSPECIFIED.,.F.,.F.,(3,3),(0.,1.),.UNSPECIFIED.);
#720=B_SPLINE_CURVE_WITH_KNOTS('',2,(#43256,#43257,#43258),
 .UNSPECIFIED.,.F.,.F.,(3,3),(0.,1.),.UNSPECIFIED.);
#721=B_SPLINE_CURVE_WITH_KNOTS('',2,(#43261,#43262,#43263),
 .UNSPECIFIED.,.F.,.F.,(3,3),(0.,1.),.UNSPECIFIED.);
#722=B_SPLINE_CURVE_WITH_KNOTS('',2,(#43271,#43272,#43273),
 .UNSPECIFIED.,.F.,.F.,(3,3),(0.,1.),.UNSPECIFIED.);
#723=B_SPLINE_CURVE_WITH_KNOTS('',2,(#43276,#43277,#43278),
 .UNSPECIFIED.,.F.,.F.,(3,3),(0.,1.),.UNSPECIFIED.);
#724=B_SPLINE_CURVE_WITH_KNOTS('',2,(#43286,#43287,#43288),
 .UNSPECIFIED.,.F.,.F.,(3,3),(0.,1.),.UNSPECIFIED.);
#725=B_SPLINE_CURVE_WITH_KNOTS('',2,(#43291,#43292,#43293),
 .UNSPECIFIED.,.F.,.F.,(3,3),(0.,1.),.UNSPECIFIED.);
#726=B_SPLINE_CURVE_WITH_KNOTS('',2,(#43301,#43302,#43303),
 .UNSPECIFIED.,.F.,.F.,(3,3),(0.,1.),.UNSPECIFIED.);
#727=B_SPLINE_CURVE_WITH_KNOTS('',2,(#43306,#43307,#43308),
 .UNSPECIFIED.,.F.,.F.,(3,3),(0.,1.),.UNSPECIFIED.);
#728=B_SPLINE_CURVE_WITH_KNOTS('',2,(#43316,#43317,#43318),
 .UNSPECIFIED.,.F.,.F.,(3,3),(0.,1.),.UNSPECIFIED.);
#729=B_SPLINE_CURVE_WITH_KNOTS('',2,(#43321,#43322,#43323),
 .UNSPECIFIED.,.F.,.F.,(3,3),(0.,1.),.UNSPECIFIED.);
#730=B_SPLINE_CURVE_WITH_KNOTS('',2,(#43331,#43332,#43333),
 .UNSPECIFIED.,.F.,.F.,(3,3),(0.,1.),.UNSPECIFIED.);
#731=B_SPLINE_CURVE_WITH_KNOTS('',2,(#43336,#43337,#43338),
 .UNSPECIFIED.,.F.,.F.,(3,3),(0.,1.),.UNSPECIFIED.);
#732=B_SPLINE_CURVE_WITH_KNOTS('',2,(#43346,#43347,#43348),
 .UNSPECIFIED.,.F.,.F.,(3,3),(0.,1.),.UNSPECIFIED.);
#733=B_SPLINE_CURVE_WITH_KNOTS('',2,(#43351,#43352,#43353),
 .UNSPECIFIED.,.F.,.F.,(3,3),(0.,1.),.UNSPECIFIED.);
#734=B_SPLINE_CURVE_WITH_KNOTS('',2,(#43365,#43366,#43367),
 .UNSPECIFIED.,.F.,.F.,(3,3),(0.,1.),.UNSPECIFIED.);
#735=B_SPLINE_CURVE_WITH_KNOTS('',2,(#43371,#43372,#43373),
 .UNSPECIFIED.,.F.,.F.,(3,3),(0.,1.),.UNSPECIFIED.);
#736=B_SPLINE_CURVE_WITH_KNOTS('',2,(#43382,#43383,#43384),
 .UNSPECIFIED.,.F.,.F.,(3,3),(0.,1.),.UNSPECIFIED.);
#737=B_SPLINE_CURVE_WITH_KNOTS('',2,(#43387,#43388,#43389),
 .UNSPECIFIED.,.F.,.F.,(3,3),(0.,1.),.UNSPECIFIED.);
#738=B_SPLINE_CURVE_WITH_KNOTS('',2,(#43403,#43404,#43405),
 .UNSPECIFIED.,.F.,.F.,(3,3),(0.,1.),.UNSPECIFIED.);
#739=B_SPLINE_CURVE_WITH_KNOTS('',2,(#43408,#43409,#43410),
 .UNSPECIFIED.,.F.,.F.,(3,3),(0.,1.),.UNSPECIFIED.);
#740=B_SPLINE_CURVE_WITH_KNOTS('',2,(#43418,#43419,#43420),
 .UNSPECIFIED.,.F.,.F.,(3,3),(0.,1.),.UNSPECIFIED.);
#741=B_SPLINE_CURVE_WITH_KNOTS('',2,(#43423,#43424,#43425),
 .UNSPECIFIED.,.F.,.F.,(3,3),(0.,1.),.UNSPECIFIED.);
#742=B_SPLINE_CURVE_WITH_KNOTS('',2,(#43433,#43434,#43435),
 .UNSPECIFIED.,.F.,.F.,(3,3),(0.,1.),.UNSPECIFIED.);
#743=B_SPLINE_CURVE_WITH_KNOTS('',2,(#43438,#43439,#43440),
 .UNSPECIFIED.,.F.,.F.,(3,3),(0.,1.),.UNSPECIFIED.);
#744=B_SPLINE_CURVE_WITH_KNOTS('',2,(#43448,#43449,#43450),
 .UNSPECIFIED.,.F.,.F.,(3,3),(0.,1.),.UNSPECIFIED.);
#745=B_SPLINE_CURVE_WITH_KNOTS('',2,(#43453,#43454,#43455),
 .UNSPECIFIED.,.F.,.F.,(3,3),(0.,1.),.UNSPECIFIED.);
#746=B_SPLINE_CURVE_WITH_KNOTS('',2,(#43463,#43464,#43465),
 .UNSPECIFIED.,.F.,.F.,(3,3),(0.,1.),.UNSPECIFIED.);
#747=B_SPLINE_CURVE_WITH_KNOTS('',2,(#43468,#43469,#43470),
 .UNSPECIFIED.,.F.,.F.,(3,3),(0.,1.),.UNSPECIFIED.);
#748=B_SPLINE_CURVE_WITH_KNOTS('',2,(#43478,#43479,#43480),
 .UNSPECIFIED.,.F.,.F.,(3,3),(0.,1.),.UNSPECIFIED.);
#749=B_SPLINE_CURVE_WITH_KNOTS('',2,(#43483,#43484,#43485),
 .UNSPECIFIED.,.F.,.F.,(3,3),(0.,1.),.UNSPECIFIED.);
#750=B_SPLINE_CURVE_WITH_KNOTS('',2,(#43493,#43494,#43495),
 .UNSPECIFIED.,.F.,.F.,(3,3),(0.,1.),.UNSPECIFIED.);
#751=B_SPLINE_CURVE_WITH_KNOTS('',2,(#43498,#43499,#43500),
 .UNSPECIFIED.,.F.,.F.,(3,3),(0.,1.),.UNSPECIFIED.);
#752=B_SPLINE_CURVE_WITH_KNOTS('',2,(#43514,#43515,#43516),
 .UNSPECIFIED.,.F.,.F.,(3,3),(0.,1.),.UNSPECIFIED.);
#753=B_SPLINE_CURVE_WITH_KNOTS('',2,(#43519,#43520,#43521),
 .UNSPECIFIED.,.F.,.F.,(3,3),(0.,1.),.UNSPECIFIED.);
#754=B_SPLINE_CURVE_WITH_KNOTS('',2,(#43529,#43530,#43531),
 .UNSPECIFIED.,.F.,.F.,(3,3),(0.,1.),.UNSPECIFIED.);
#755=B_SPLINE_CURVE_WITH_KNOTS('',2,(#43534,#43535,#43536),
 .UNSPECIFIED.,.F.,.F.,(3,3),(0.,1.),.UNSPECIFIED.);
#756=B_SPLINE_CURVE_WITH_KNOTS('',2,(#43544,#43545,#43546),
 .UNSPECIFIED.,.F.,.F.,(3,3),(0.,1.),.UNSPECIFIED.);
#757=B_SPLINE_CURVE_WITH_KNOTS('',2,(#43549,#43550,#43551),
 .UNSPECIFIED.,.F.,.F.,(3,3),(0.,1.),.UNSPECIFIED.);
#758=B_SPLINE_CURVE_WITH_KNOTS('',2,(#43559,#43560,#43561),
 .UNSPECIFIED.,.F.,.F.,(3,3),(0.,1.),.UNSPECIFIED.);
#759=B_SPLINE_CURVE_WITH_KNOTS('',2,(#43564,#43565,#43566),
 .UNSPECIFIED.,.F.,.F.,(3,3),(0.,1.),.UNSPECIFIED.);
#760=B_SPLINE_CURVE_WITH_KNOTS('',2,(#43574,#43575,#43576),
 .UNSPECIFIED.,.F.,.F.,(3,3),(0.,1.),.UNSPECIFIED.);
#761=B_SPLINE_CURVE_WITH_KNOTS('',2,(#43579,#43580,#43581),
 .UNSPECIFIED.,.F.,.F.,(3,3),(0.,1.),.UNSPECIFIED.);
#762=B_SPLINE_CURVE_WITH_KNOTS('',2,(#43589,#43590,#43591),
 .UNSPECIFIED.,.F.,.F.,(3,3),(0.,1.),.UNSPECIFIED.);
#763=B_SPLINE_CURVE_WITH_KNOTS('',2,(#43594,#43595,#43596),
 .UNSPECIFIED.,.F.,.F.,(3,3),(0.,1.),.UNSPECIFIED.);
#764=B_SPLINE_CURVE_WITH_KNOTS('',2,(#43604,#43605,#43606),
 .UNSPECIFIED.,.F.,.F.,(3,3),(0.,1.),.UNSPECIFIED.);
#765=B_SPLINE_CURVE_WITH_KNOTS('',2,(#43609,#43610,#43611),
 .UNSPECIFIED.,.F.,.F.,(3,3),(0.,1.),.UNSPECIFIED.);
#766=B_SPLINE_CURVE_WITH_KNOTS('',2,(#43619,#43620,#43621),
 .UNSPECIFIED.,.F.,.F.,(3,3),(0.,1.),.UNSPECIFIED.);
#767=B_SPLINE_CURVE_WITH_KNOTS('',2,(#43624,#43625,#43626),
 .UNSPECIFIED.,.F.,.F.,(3,3),(0.,1.),.UNSPECIFIED.);
#768=B_SPLINE_CURVE_WITH_KNOTS('',2,(#43634,#43635,#43636),
 .UNSPECIFIED.,.F.,.F.,(3,3),(0.,1.),.UNSPECIFIED.);
#769=B_SPLINE_CURVE_WITH_KNOTS('',2,(#43639,#43640,#43641),
 .UNSPECIFIED.,.F.,.F.,(3,3),(0.,1.),.UNSPECIFIED.);
#770=B_SPLINE_CURVE_WITH_KNOTS('',2,(#43649,#43650,#43651),
 .UNSPECIFIED.,.F.,.F.,(3,3),(0.,1.),.UNSPECIFIED.);
#771=B_SPLINE_CURVE_WITH_KNOTS('',2,(#43654,#43655,#43656),
 .UNSPECIFIED.,.F.,.F.,(3,3),(0.,1.),.UNSPECIFIED.);
#772=B_SPLINE_CURVE_WITH_KNOTS('',2,(#43664,#43665,#43666),
 .UNSPECIFIED.,.F.,.F.,(3,3),(0.,1.),.UNSPECIFIED.);
#773=B_SPLINE_CURVE_WITH_KNOTS('',2,(#43669,#43670,#43671),
 .UNSPECIFIED.,.F.,.F.,(3,3),(0.,1.),.UNSPECIFIED.);
#774=B_SPLINE_CURVE_WITH_KNOTS('',2,(#43679,#43680,#43681),
 .UNSPECIFIED.,.F.,.F.,(3,3),(0.,1.),.UNSPECIFIED.);
#775=B_SPLINE_CURVE_WITH_KNOTS('',2,(#43684,#43685,#43686),
 .UNSPECIFIED.,.F.,.F.,(3,3),(0.,1.),.UNSPECIFIED.);
#776=B_SPLINE_CURVE_WITH_KNOTS('',2,(#43694,#43695,#43696),
 .UNSPECIFIED.,.F.,.F.,(3,3),(0.,1.),.UNSPECIFIED.);
#777=B_SPLINE_CURVE_WITH_KNOTS('',2,(#43699,#43700,#43701),
 .UNSPECIFIED.,.F.,.F.,(3,3),(0.,1.),.UNSPECIFIED.);
#778=B_SPLINE_CURVE_WITH_KNOTS('',2,(#43709,#43710,#43711),
 .UNSPECIFIED.,.F.,.F.,(3,3),(0.,1.),.UNSPECIFIED.);
#779=B_SPLINE_CURVE_WITH_KNOTS('',2,(#43714,#43715,#43716),
 .UNSPECIFIED.,.F.,.F.,(3,3),(0.,1.),.UNSPECIFIED.);
#780=B_SPLINE_CURVE_WITH_KNOTS('',2,(#43724,#43725,#43726),
 .UNSPECIFIED.,.F.,.F.,(3,3),(0.,1.),.UNSPECIFIED.);
#781=B_SPLINE_CURVE_WITH_KNOTS('',2,(#43729,#43730,#43731),
 .UNSPECIFIED.,.F.,.F.,(3,3),(0.,1.),.UNSPECIFIED.);
#782=B_SPLINE_CURVE_WITH_KNOTS('',2,(#43744,#43745,#43746),
 .UNSPECIFIED.,.F.,.F.,(3,3),(0.,1.),.UNSPECIFIED.);
#783=B_SPLINE_CURVE_WITH_KNOTS('',2,(#43750,#43751,#43752),
 .UNSPECIFIED.,.F.,.F.,(3,3),(0.,1.),.UNSPECIFIED.);
#784=B_SPLINE_CURVE_WITH_KNOTS('',2,(#43761,#43762,#43763),
 .UNSPECIFIED.,.F.,.F.,(3,3),(0.,1.),.UNSPECIFIED.);
#785=B_SPLINE_CURVE_WITH_KNOTS('',2,(#43766,#43767,#43768),
 .UNSPECIFIED.,.F.,.F.,(3,3),(0.,1.),.UNSPECIFIED.);
#786=B_SPLINE_CURVE_WITH_KNOTS('',2,(#43776,#43777,#43778),
 .UNSPECIFIED.,.F.,.F.,(3,3),(0.,1.),.UNSPECIFIED.);
#787=B_SPLINE_CURVE_WITH_KNOTS('',2,(#43781,#43782,#43783),
 .UNSPECIFIED.,.F.,.F.,(3,3),(0.,1.),.UNSPECIFIED.);
#788=B_SPLINE_CURVE_WITH_KNOTS('',2,(#43791,#43792,#43793),
 .UNSPECIFIED.,.F.,.F.,(3,3),(0.,1.),.UNSPECIFIED.);
#789=B_SPLINE_CURVE_WITH_KNOTS('',2,(#43796,#43797,#43798),
 .UNSPECIFIED.,.F.,.F.,(3,3),(0.,1.),.UNSPECIFIED.);
#790=B_SPLINE_CURVE_WITH_KNOTS('',2,(#43806,#43807,#43808),
 .UNSPECIFIED.,.F.,.F.,(3,3),(0.,1.),.UNSPECIFIED.);
#791=B_SPLINE_CURVE_WITH_KNOTS('',2,(#43811,#43812,#43813),
 .UNSPECIFIED.,.F.,.F.,(3,3),(0.,1.),.UNSPECIFIED.);
#792=B_SPLINE_CURVE_WITH_KNOTS('',2,(#43821,#43822,#43823),
 .UNSPECIFIED.,.F.,.F.,(3,3),(0.,1.),.UNSPECIFIED.);
#793=B_SPLINE_CURVE_WITH_KNOTS('',2,(#43826,#43827,#43828),
 .UNSPECIFIED.,.F.,.F.,(3,3),(0.,1.),.UNSPECIFIED.);
#794=B_SPLINE_CURVE_WITH_KNOTS('',2,(#43836,#43837,#43838),
 .UNSPECIFIED.,.F.,.F.,(3,3),(0.,1.),.UNSPECIFIED.);
#795=B_SPLINE_CURVE_WITH_KNOTS('',2,(#43841,#43842,#43843),
 .UNSPECIFIED.,.F.,.F.,(3,3),(0.,1.),.UNSPECIFIED.);
#796=B_SPLINE_CURVE_WITH_KNOTS('',2,(#43850,#43851,#43852),
 .UNSPECIFIED.,.F.,.F.,(3,3),(0.,1.),.UNSPECIFIED.);
#797=B_SPLINE_CURVE_WITH_KNOTS('',2,(#43853,#43854,#43855),
 .UNSPECIFIED.,.F.,.F.,(3,3),(0.,1.),.UNSPECIFIED.);
#798=B_SPLINE_CURVE_WITH_KNOTS('',2,(#43864,#43865,#43866),
 .UNSPECIFIED.,.F.,.F.,(3,3),(0.,1.),.UNSPECIFIED.);
#799=B_SPLINE_CURVE_WITH_KNOTS('',2,(#43870,#43871,#43872),
 .UNSPECIFIED.,.F.,.F.,(3,3),(0.,1.),.UNSPECIFIED.);
#800=B_SPLINE_CURVE_WITH_KNOTS('',2,(#43881,#43882,#43883),
 .UNSPECIFIED.,.F.,.F.,(3,3),(0.,1.),.UNSPECIFIED.);
#801=B_SPLINE_CURVE_WITH_KNOTS('',2,(#43886,#43887,#43888),
 .UNSPECIFIED.,.F.,.F.,(3,3),(0.,1.),.UNSPECIFIED.);
#802=B_SPLINE_CURVE_WITH_KNOTS('',2,(#43896,#43897,#43898),
 .UNSPECIFIED.,.F.,.F.,(3,3),(0.,1.),.UNSPECIFIED.);
#803=B_SPLINE_CURVE_WITH_KNOTS('',2,(#43901,#43902,#43903),
 .UNSPECIFIED.,.F.,.F.,(3,3),(0.,1.),.UNSPECIFIED.);
#804=B_SPLINE_CURVE_WITH_KNOTS('',2,(#43911,#43912,#43913),
 .UNSPECIFIED.,.F.,.F.,(3,3),(0.,1.),.UNSPECIFIED.);
#805=B_SPLINE_CURVE_WITH_KNOTS('',2,(#43916,#43917,#43918),
 .UNSPECIFIED.,.F.,.F.,(3,3),(0.,1.),.UNSPECIFIED.);
#806=B_SPLINE_CURVE_WITH_KNOTS('',2,(#43926,#43927,#43928),
 .UNSPECIFIED.,.F.,.F.,(3,3),(0.,1.),.UNSPECIFIED.);
#807=B_SPLINE_CURVE_WITH_KNOTS('',2,(#43931,#43932,#43933),
 .UNSPECIFIED.,.F.,.F.,(3,3),(0.,1.),.UNSPECIFIED.);
#808=B_SPLINE_CURVE_WITH_KNOTS('',2,(#43941,#43942,#43943),
 .UNSPECIFIED.,.F.,.F.,(3,3),(0.,1.),.UNSPECIFIED.);
#809=B_SPLINE_CURVE_WITH_KNOTS('',2,(#43946,#43947,#43948),
 .UNSPECIFIED.,.F.,.F.,(3,3),(0.,1.),.UNSPECIFIED.);
#810=B_SPLINE_CURVE_WITH_KNOTS('',2,(#43956,#43957,#43958),
 .UNSPECIFIED.,.F.,.F.,(3,3),(0.,1.),.UNSPECIFIED.);
#811=B_SPLINE_CURVE_WITH_KNOTS('',2,(#43961,#43962,#43963),
 .UNSPECIFIED.,.F.,.F.,(3,3),(0.,1.),.UNSPECIFIED.);
#812=B_SPLINE_CURVE_WITH_KNOTS('',2,(#43971,#43972,#43973),
 .UNSPECIFIED.,.F.,.F.,(3,3),(0.,1.),.UNSPECIFIED.);
#813=B_SPLINE_CURVE_WITH_KNOTS('',2,(#43976,#43977,#43978),
 .UNSPECIFIED.,.F.,.F.,(3,3),(0.,1.),.UNSPECIFIED.);
#814=B_SPLINE_CURVE_WITH_KNOTS('',2,(#43986,#43987,#43988),
 .UNSPECIFIED.,.F.,.F.,(3,3),(0.,1.),.UNSPECIFIED.);
#815=B_SPLINE_CURVE_WITH_KNOTS('',2,(#43991,#43992,#43993),
 .UNSPECIFIED.,.F.,.F.,(3,3),(0.,1.),.UNSPECIFIED.);
#816=B_SPLINE_CURVE_WITH_KNOTS('',2,(#44001,#44002,#44003),
 .UNSPECIFIED.,.F.,.F.,(3,3),(0.,1.),.UNSPECIFIED.);
#817=B_SPLINE_CURVE_WITH_KNOTS('',2,(#44006,#44007,#44008),
 .UNSPECIFIED.,.F.,.F.,(3,3),(0.,1.),.UNSPECIFIED.);
#818=B_SPLINE_CURVE_WITH_KNOTS('',2,(#44016,#44017,#44018),
 .UNSPECIFIED.,.F.,.F.,(3,3),(0.,1.),.UNSPECIFIED.);
#819=B_SPLINE_CURVE_WITH_KNOTS('',2,(#44021,#44022,#44023),
 .UNSPECIFIED.,.F.,.F.,(3,3),(0.,1.),.UNSPECIFIED.);
#820=B_SPLINE_CURVE_WITH_KNOTS('',2,(#44030,#44031,#44032),
 .UNSPECIFIED.,.F.,.F.,(3,3),(0.,1.),.UNSPECIFIED.);
#821=B_SPLINE_CURVE_WITH_KNOTS('',2,(#44033,#44034,#44035),
 .UNSPECIFIED.,.F.,.F.,(3,3),(0.,1.),.UNSPECIFIED.);
#822=B_SPLINE_CURVE_WITH_KNOTS('',2,(#44045,#44046,#44047),
 .UNSPECIFIED.,.F.,.F.,(3,3),(0.,1.),.UNSPECIFIED.);
#823=B_SPLINE_CURVE_WITH_KNOTS('',2,(#44051,#44052,#44053),
 .UNSPECIFIED.,.F.,.F.,(3,3),(0.,1.),.UNSPECIFIED.);
#824=B_SPLINE_CURVE_WITH_KNOTS('',2,(#44062,#44063,#44064),
 .UNSPECIFIED.,.F.,.F.,(3,3),(0.,1.),.UNSPECIFIED.);
#825=B_SPLINE_CURVE_WITH_KNOTS('',2,(#44067,#44068,#44069),
 .UNSPECIFIED.,.F.,.F.,(3,3),(0.,1.),.UNSPECIFIED.);
#826=B_SPLINE_CURVE_WITH_KNOTS('',2,(#44083,#44084,#44085),
 .UNSPECIFIED.,.F.,.F.,(3,3),(0.,1.),.UNSPECIFIED.);
#827=B_SPLINE_CURVE_WITH_KNOTS('',2,(#44088,#44089,#44090),
 .UNSPECIFIED.,.F.,.F.,(3,3),(0.,1.),.UNSPECIFIED.);
#828=B_SPLINE_CURVE_WITH_KNOTS('',2,(#44098,#44099,#44100),
 .UNSPECIFIED.,.F.,.F.,(3,3),(0.,1.),.UNSPECIFIED.);
#829=B_SPLINE_CURVE_WITH_KNOTS('',2,(#44103,#44104,#44105),
 .UNSPECIFIED.,.F.,.F.,(3,3),(0.,1.),.UNSPECIFIED.);
#830=B_SPLINE_CURVE_WITH_KNOTS('',2,(#44186,#44187,#44188),
 .UNSPECIFIED.,.F.,.F.,(3,3),(0.,1.),.UNSPECIFIED.);
#831=B_SPLINE_CURVE_WITH_KNOTS('',2,(#44191,#44192,#44193),
 .UNSPECIFIED.,.F.,.F.,(3,3),(0.,1.),.UNSPECIFIED.);
#832=B_SPLINE_CURVE_WITH_KNOTS('',2,(#44201,#44202,#44203),
 .UNSPECIFIED.,.F.,.F.,(3,3),(0.,1.),.UNSPECIFIED.);
#833=B_SPLINE_CURVE_WITH_KNOTS('',2,(#44206,#44207,#44208),
 .UNSPECIFIED.,.F.,.F.,(3,3),(0.,1.),.UNSPECIFIED.);
#834=B_SPLINE_CURVE_WITH_KNOTS('',2,(#44245,#44246,#44247),
 .UNSPECIFIED.,.F.,.F.,(3,3),(0.,1.),.UNSPECIFIED.);
#835=B_SPLINE_CURVE_WITH_KNOTS('',2,(#44251,#44252,#44253),
 .UNSPECIFIED.,.F.,.F.,(3,3),(0.,1.),.UNSPECIFIED.);
#836=B_SPLINE_CURVE_WITH_KNOTS('',2,(#44262,#44263,#44264),
 .UNSPECIFIED.,.F.,.F.,(3,3),(0.,1.),.UNSPECIFIED.);
#837=B_SPLINE_CURVE_WITH_KNOTS('',2,(#44267,#44268,#44269),
 .UNSPECIFIED.,.F.,.F.,(3,3),(0.,1.),.UNSPECIFIED.);
#838=B_SPLINE_CURVE_WITH_KNOTS('',2,(#44277,#44278,#44279),
 .UNSPECIFIED.,.F.,.F.,(3,3),(0.,1.),.UNSPECIFIED.);
#839=B_SPLINE_CURVE_WITH_KNOTS('',2,(#44282,#44283,#44284),
 .UNSPECIFIED.,.F.,.F.,(3,3),(0.,1.),.UNSPECIFIED.);
#840=B_SPLINE_CURVE_WITH_KNOTS('',2,(#44292,#44293,#44294),
 .UNSPECIFIED.,.F.,.F.,(3,3),(0.,1.),.UNSPECIFIED.);
#841=B_SPLINE_CURVE_WITH_KNOTS('',2,(#44297,#44298,#44299),
 .UNSPECIFIED.,.F.,.F.,(3,3),(0.,1.),.UNSPECIFIED.);
#842=B_SPLINE_CURVE_WITH_KNOTS('',2,(#44307,#44308,#44309),
 .UNSPECIFIED.,.F.,.F.,(3,3),(0.,1.),.UNSPECIFIED.);
#843=B_SPLINE_CURVE_WITH_KNOTS('',2,(#44312,#44313,#44314),
 .UNSPECIFIED.,.F.,.F.,(3,3),(0.,1.),.UNSPECIFIED.);
#844=B_SPLINE_CURVE_WITH_KNOTS('',2,(#44322,#44323,#44324),
 .UNSPECIFIED.,.F.,.F.,(3,3),(0.,1.),.UNSPECIFIED.);
#845=B_SPLINE_CURVE_WITH_KNOTS('',2,(#44327,#44328,#44329),
 .UNSPECIFIED.,.F.,.F.,(3,3),(0.,1.),.UNSPECIFIED.);
#846=B_SPLINE_CURVE_WITH_KNOTS('',2,(#44337,#44338,#44339),
 .UNSPECIFIED.,.F.,.F.,(3,3),(0.,1.),.UNSPECIFIED.);
#847=B_SPLINE_CURVE_WITH_KNOTS('',2,(#44342,#44343,#44344),
 .UNSPECIFIED.,.F.,.F.,(3,3),(0.,1.),.UNSPECIFIED.);
#848=B_SPLINE_CURVE_WITH_KNOTS('',2,(#44352,#44353,#44354),
 .UNSPECIFIED.,.F.,.F.,(3,3),(0.,1.),.UNSPECIFIED.);
#849=B_SPLINE_CURVE_WITH_KNOTS('',2,(#44357,#44358,#44359),
 .UNSPECIFIED.,.F.,.F.,(3,3),(0.,1.),.UNSPECIFIED.);
#850=B_SPLINE_CURVE_WITH_KNOTS('',2,(#44367,#44368,#44369),
 .UNSPECIFIED.,.F.,.F.,(3,3),(0.,1.),.UNSPECIFIED.);
#851=B_SPLINE_CURVE_WITH_KNOTS('',2,(#44372,#44373,#44374),
 .UNSPECIFIED.,.F.,.F.,(3,3),(0.,1.),.UNSPECIFIED.);
#852=B_SPLINE_CURVE_WITH_KNOTS('',2,(#44382,#44383,#44384),
 .UNSPECIFIED.,.F.,.F.,(3,3),(0.,1.),.UNSPECIFIED.);
#853=B_SPLINE_CURVE_WITH_KNOTS('',2,(#44387,#44388,#44389),
 .UNSPECIFIED.,.F.,.F.,(3,3),(0.,1.),.UNSPECIFIED.);
#854=B_SPLINE_CURVE_WITH_KNOTS('',2,(#44397,#44398,#44399),
 .UNSPECIFIED.,.F.,.F.,(3,3),(0.,1.),.UNSPECIFIED.);
#855=B_SPLINE_CURVE_WITH_KNOTS('',2,(#44402,#44403,#44404),
 .UNSPECIFIED.,.F.,.F.,(3,3),(0.,1.),.UNSPECIFIED.);
#856=B_SPLINE_CURVE_WITH_KNOTS('',2,(#44418,#44419,#44420),
 .UNSPECIFIED.,.F.,.F.,(3,3),(0.,1.),.UNSPECIFIED.);
#857=B_SPLINE_CURVE_WITH_KNOTS('',2,(#44423,#44424,#44425),
 .UNSPECIFIED.,.F.,.F.,(3,3),(0.,1.),.UNSPECIFIED.);
#858=B_SPLINE_CURVE_WITH_KNOTS('',2,(#44433,#44434,#44435),
 .UNSPECIFIED.,.F.,.F.,(3,3),(0.,1.),.UNSPECIFIED.);
#859=B_SPLINE_CURVE_WITH_KNOTS('',2,(#44438,#44439,#44440),
 .UNSPECIFIED.,.F.,.F.,(3,3),(0.,1.),.UNSPECIFIED.);
#860=B_SPLINE_CURVE_WITH_KNOTS('',2,(#44448,#44449,#44450),
 .UNSPECIFIED.,.F.,.F.,(3,3),(0.,1.),.UNSPECIFIED.);
#861=B_SPLINE_CURVE_WITH_KNOTS('',2,(#44453,#44454,#44455),
 .UNSPECIFIED.,.F.,.F.,(3,3),(0.,1.),.UNSPECIFIED.);
#862=B_SPLINE_CURVE_WITH_KNOTS('',2,(#44463,#44464,#44465),
 .UNSPECIFIED.,.F.,.F.,(3,3),(0.,1.),.UNSPECIFIED.);
#863=B_SPLINE_CURVE_WITH_KNOTS('',2,(#44468,#44469,#44470),
 .UNSPECIFIED.,.F.,.F.,(3,3),(0.,1.),.UNSPECIFIED.);
#864=B_SPLINE_CURVE_WITH_KNOTS('',2,(#44478,#44479,#44480),
 .UNSPECIFIED.,.F.,.F.,(3,3),(0.,1.),.UNSPECIFIED.);
#865=B_SPLINE_CURVE_WITH_KNOTS('',2,(#44483,#44484,#44485),
 .UNSPECIFIED.,.F.,.F.,(3,3),(0.,1.),.UNSPECIFIED.);
#866=B_SPLINE_CURVE_WITH_KNOTS('',2,(#44493,#44494,#44495),
 .UNSPECIFIED.,.F.,.F.,(3,3),(0.,1.),.UNSPECIFIED.);
#867=B_SPLINE_CURVE_WITH_KNOTS('',2,(#44498,#44499,#44500),
 .UNSPECIFIED.,.F.,.F.,(3,3),(0.,1.),.UNSPECIFIED.);
#868=B_SPLINE_CURVE_WITH_KNOTS('',2,(#44508,#44509,#44510),
 .UNSPECIFIED.,.F.,.F.,(3,3),(0.,1.),.UNSPECIFIED.);
#869=B_SPLINE_CURVE_WITH_KNOTS('',2,(#44513,#44514,#44515),
 .UNSPECIFIED.,.F.,.F.,(3,3),(0.,1.),.UNSPECIFIED.);
#870=B_SPLINE_CURVE_WITH_KNOTS('',2,(#44529,#44530,#44531),
 .UNSPECIFIED.,.F.,.F.,(3,3),(0.,1.),.UNSPECIFIED.);
#871=B_SPLINE_CURVE_WITH_KNOTS('',2,(#44534,#44535,#44536),
 .UNSPECIFIED.,.F.,.F.,(3,3),(0.,1.),.UNSPECIFIED.);
#872=B_SPLINE_CURVE_WITH_KNOTS('',2,(#44544,#44545,#44546),
 .UNSPECIFIED.,.F.,.F.,(3,3),(0.,1.),.UNSPECIFIED.);
#873=B_SPLINE_CURVE_WITH_KNOTS('',2,(#44549,#44550,#44551),
 .UNSPECIFIED.,.F.,.F.,(3,3),(0.,1.),.UNSPECIFIED.);
#874=B_SPLINE_CURVE_WITH_KNOTS('',2,(#44559,#44560,#44561),
 .UNSPECIFIED.,.F.,.F.,(3,3),(0.,1.),.UNSPECIFIED.);
#875=B_SPLINE_CURVE_WITH_KNOTS('',2,(#44564,#44565,#44566),
 .UNSPECIFIED.,.F.,.F.,(3,3),(0.,1.),.UNSPECIFIED.);
#876=B_SPLINE_CURVE_WITH_KNOTS('',2,(#44574,#44575,#44576),
 .UNSPECIFIED.,.F.,.F.,(3,3),(0.,1.),.UNSPECIFIED.);
#877=B_SPLINE_CURVE_WITH_KNOTS('',2,(#44579,#44580,#44581),
 .UNSPECIFIED.,.F.,.F.,(3,3),(0.,1.),.UNSPECIFIED.);
#878=B_SPLINE_CURVE_WITH_KNOTS('',2,(#44589,#44590,#44591),
 .UNSPECIFIED.,.F.,.F.,(3,3),(0.,1.),.UNSPECIFIED.);
#879=B_SPLINE_CURVE_WITH_KNOTS('',2,(#44594,#44595,#44596),
 .UNSPECIFIED.,.F.,.F.,(3,3),(0.,1.),.UNSPECIFIED.);
#880=B_SPLINE_CURVE_WITH_KNOTS('',2,(#44604,#44605,#44606),
 .UNSPECIFIED.,.F.,.F.,(3,3),(0.,1.),.UNSPECIFIED.);
#881=B_SPLINE_CURVE_WITH_KNOTS('',2,(#44609,#44610,#44611),
 .UNSPECIFIED.,.F.,.F.,(3,3),(0.,1.),.UNSPECIFIED.);
#882=B_SPLINE_CURVE_WITH_KNOTS('',2,(#44619,#44620,#44621),
 .UNSPECIFIED.,.F.,.F.,(3,3),(0.,1.),.UNSPECIFIED.);
#883=B_SPLINE_CURVE_WITH_KNOTS('',2,(#44624,#44625,#44626),
 .UNSPECIFIED.,.F.,.F.,(3,3),(0.,1.),.UNSPECIFIED.);
#884=B_SPLINE_CURVE_WITH_KNOTS('',2,(#44640,#44641,#44642),
 .UNSPECIFIED.,.F.,.F.,(3,3),(0.,1.),.UNSPECIFIED.);
#885=B_SPLINE_CURVE_WITH_KNOTS('',2,(#44645,#44646,#44647),
 .UNSPECIFIED.,.F.,.F.,(3,3),(0.,1.),.UNSPECIFIED.);
#886=B_SPLINE_CURVE_WITH_KNOTS('',2,(#44654,#44655,#44656),
 .UNSPECIFIED.,.F.,.F.,(3,3),(0.,1.),.UNSPECIFIED.);
#887=B_SPLINE_CURVE_WITH_KNOTS('',2,(#44657,#44658,#44659),
 .UNSPECIFIED.,.F.,.F.,(3,3),(0.,1.),.UNSPECIFIED.);
#888=B_SPLINE_CURVE_WITH_KNOTS('',2,(#44694,#44695,#44696),
 .UNSPECIFIED.,.F.,.F.,(3,3),(0.,1.),.UNSPECIFIED.);
#889=B_SPLINE_CURVE_WITH_KNOTS('',2,(#44700,#44701,#44702),
 .UNSPECIFIED.,.F.,.F.,(3,3),(0.,1.),.UNSPECIFIED.);
#890=B_SPLINE_CURVE_WITH_KNOTS('',2,(#44711,#44712,#44713),
 .UNSPECIFIED.,.F.,.F.,(3,3),(0.,1.),.UNSPECIFIED.);
#891=B_SPLINE_CURVE_WITH_KNOTS('',2,(#44716,#44717,#44718),
 .UNSPECIFIED.,.F.,.F.,(3,3),(0.,1.),.UNSPECIFIED.);
#892=B_SPLINE_CURVE_WITH_KNOTS('',2,(#44791,#44792,#44793),
 .UNSPECIFIED.,.F.,.F.,(3,3),(0.,1.),.UNSPECIFIED.);
#893=B_SPLINE_CURVE_WITH_KNOTS('',2,(#44797,#44798,#44799),
 .UNSPECIFIED.,.F.,.F.,(3,3),(0.,1.),.UNSPECIFIED.);
#894=B_SPLINE_CURVE_WITH_KNOTS('',2,(#44808,#44809,#44810),
 .UNSPECIFIED.,.F.,.F.,(3,3),(0.,1.),.UNSPECIFIED.);
#895=B_SPLINE_CURVE_WITH_KNOTS('',2,(#44813,#44814,#44815),
 .UNSPECIFIED.,.F.,.F.,(3,3),(0.,1.),.UNSPECIFIED.);
#896=B_SPLINE_CURVE_WITH_KNOTS('',2,(#44823,#44824,#44825),
 .UNSPECIFIED.,.F.,.F.,(3,3),(0.,1.),.UNSPECIFIED.);
#897=B_SPLINE_CURVE_WITH_KNOTS('',2,(#44828,#44829,#44830),
 .UNSPECIFIED.,.F.,.F.,(3,3),(0.,1.),.UNSPECIFIED.);
#898=B_SPLINE_CURVE_WITH_KNOTS('',2,(#44838,#44839,#44840),
 .UNSPECIFIED.,.F.,.F.,(3,3),(0.,1.),.UNSPECIFIED.);
#899=B_SPLINE_CURVE_WITH_KNOTS('',2,(#44843,#44844,#44845),
 .UNSPECIFIED.,.F.,.F.,(3,3),(0.,1.),.UNSPECIFIED.);
#900=B_SPLINE_CURVE_WITH_KNOTS('',2,(#44853,#44854,#44855),
 .UNSPECIFIED.,.F.,.F.,(3,3),(0.,1.),.UNSPECIFIED.);
#901=B_SPLINE_CURVE_WITH_KNOTS('',2,(#44858,#44859,#44860),
 .UNSPECIFIED.,.F.,.F.,(3,3),(0.,1.),.UNSPECIFIED.);
#902=B_SPLINE_CURVE_WITH_KNOTS('',2,(#44868,#44869,#44870),
 .UNSPECIFIED.,.F.,.F.,(3,3),(0.,1.),.UNSPECIFIED.);
#903=B_SPLINE_CURVE_WITH_KNOTS('',2,(#44873,#44874,#44875),
 .UNSPECIFIED.,.F.,.F.,(3,3),(0.,1.),.UNSPECIFIED.);
#904=B_SPLINE_CURVE_WITH_KNOTS('',2,(#44883,#44884,#44885),
 .UNSPECIFIED.,.F.,.F.,(3,3),(0.,1.),.UNSPECIFIED.);
#905=B_SPLINE_CURVE_WITH_KNOTS('',2,(#44888,#44889,#44890),
 .UNSPECIFIED.,.F.,.F.,(3,3),(0.,1.),.UNSPECIFIED.);
#906=B_SPLINE_CURVE_WITH_KNOTS('',2,(#44898,#44899,#44900),
 .UNSPECIFIED.,.F.,.F.,(3,3),(0.,1.),.UNSPECIFIED.);
#907=B_SPLINE_CURVE_WITH_KNOTS('',2,(#44903,#44904,#44905),
 .UNSPECIFIED.,.F.,.F.,(3,3),(0.,1.),.UNSPECIFIED.);
#908=B_SPLINE_CURVE_WITH_KNOTS('',2,(#44913,#44914,#44915),
 .UNSPECIFIED.,.F.,.F.,(3,3),(0.,1.),.UNSPECIFIED.);
#909=B_SPLINE_CURVE_WITH_KNOTS('',2,(#44918,#44919,#44920),
 .UNSPECIFIED.,.F.,.F.,(3,3),(0.,1.),.UNSPECIFIED.);
#910=B_SPLINE_CURVE_WITH_KNOTS('',2,(#44928,#44929,#44930),
 .UNSPECIFIED.,.F.,.F.,(3,3),(0.,1.),.UNSPECIFIED.);
#911=B_SPLINE_CURVE_WITH_KNOTS('',2,(#44933,#44934,#44935),
 .UNSPECIFIED.,.F.,.F.,(3,3),(0.,1.),.UNSPECIFIED.);
#912=B_SPLINE_CURVE_WITH_KNOTS('',2,(#44943,#44944,#44945),
 .UNSPECIFIED.,.F.,.F.,(3,3),(0.,1.),.UNSPECIFIED.);
#913=B_SPLINE_CURVE_WITH_KNOTS('',2,(#44948,#44949,#44950),
 .UNSPECIFIED.,.F.,.F.,(3,3),(0.,1.),.UNSPECIFIED.);
#914=B_SPLINE_CURVE_WITH_KNOTS('',2,(#44958,#44959,#44960),
 .UNSPECIFIED.,.F.,.F.,(3,3),(0.,1.),.UNSPECIFIED.);
#915=B_SPLINE_CURVE_WITH_KNOTS('',2,(#44963,#44964,#44965),
 .UNSPECIFIED.,.F.,.F.,(3,3),(0.,1.),.UNSPECIFIED.);
#916=B_SPLINE_CURVE_WITH_KNOTS('',2,(#44973,#44974,#44975),
 .UNSPECIFIED.,.F.,.F.,(3,3),(0.,1.),.UNSPECIFIED.);
#917=B_SPLINE_CURVE_WITH_KNOTS('',2,(#44978,#44979,#44980),
 .UNSPECIFIED.,.F.,.F.,(3,3),(0.,1.),.UNSPECIFIED.);
#918=B_SPLINE_CURVE_WITH_KNOTS('',2,(#44994,#44995,#44996),
 .UNSPECIFIED.,.F.,.F.,(3,3),(0.,1.),.UNSPECIFIED.);
#919=B_SPLINE_CURVE_WITH_KNOTS('',2,(#44999,#45000,#45001),
 .UNSPECIFIED.,.F.,.F.,(3,3),(0.,1.),.UNSPECIFIED.);
#920=B_SPLINE_CURVE_WITH_KNOTS('',2,(#45009,#45010,#45011),
 .UNSPECIFIED.,.F.,.F.,(3,3),(0.,1.),.UNSPECIFIED.);
#921=B_SPLINE_CURVE_WITH_KNOTS('',2,(#45014,#45015,#45016),
 .UNSPECIFIED.,.F.,.F.,(3,3),(0.,1.),.UNSPECIFIED.);
#922=B_SPLINE_CURVE_WITH_KNOTS('',2,(#45024,#45025,#45026),
 .UNSPECIFIED.,.F.,.F.,(3,3),(0.,1.),.UNSPECIFIED.);
#923=B_SPLINE_CURVE_WITH_KNOTS('',2,(#45029,#45030,#45031),
 .UNSPECIFIED.,.F.,.F.,(3,3),(0.,1.),.UNSPECIFIED.);
#924=B_SPLINE_CURVE_WITH_KNOTS('',2,(#45039,#45040,#45041),
 .UNSPECIFIED.,.F.,.F.,(3,3),(0.,1.),.UNSPECIFIED.);
#925=B_SPLINE_CURVE_WITH_KNOTS('',2,(#45044,#45045,#45046),
 .UNSPECIFIED.,.F.,.F.,(3,3),(0.,1.),.UNSPECIFIED.);
#926=B_SPLINE_CURVE_WITH_KNOTS('',2,(#45054,#45055,#45056),
 .UNSPECIFIED.,.F.,.F.,(3,3),(0.,1.),.UNSPECIFIED.);
#927=B_SPLINE_CURVE_WITH_KNOTS('',2,(#45059,#45060,#45061),
 .UNSPECIFIED.,.F.,.F.,(3,3),(0.,1.),.UNSPECIFIED.);
#928=B_SPLINE_CURVE_WITH_KNOTS('',2,(#45069,#45070,#45071),
 .UNSPECIFIED.,.F.,.F.,(3,3),(0.,1.),.UNSPECIFIED.);
#929=B_SPLINE_CURVE_WITH_KNOTS('',2,(#45074,#45075,#45076),
 .UNSPECIFIED.,.F.,.F.,(3,3),(0.,1.),.UNSPECIFIED.);
#930=B_SPLINE_CURVE_WITH_KNOTS('',2,(#45084,#45085,#45086),
 .UNSPECIFIED.,.F.,.F.,(3,3),(0.,1.),.UNSPECIFIED.);
#931=B_SPLINE_CURVE_WITH_KNOTS('',2,(#45089,#45090,#45091),
 .UNSPECIFIED.,.F.,.F.,(3,3),(0.,1.),.UNSPECIFIED.);
#932=B_SPLINE_CURVE_WITH_KNOTS('',2,(#45099,#45100,#45101),
 .UNSPECIFIED.,.F.,.F.,(3,3),(0.,1.),.UNSPECIFIED.);
#933=B_SPLINE_CURVE_WITH_KNOTS('',2,(#45104,#45105,#45106),
 .UNSPECIFIED.,.F.,.F.,(3,3),(0.,1.),.UNSPECIFIED.);
#934=B_SPLINE_CURVE_WITH_KNOTS('',2,(#45114,#45115,#45116),
 .UNSPECIFIED.,.F.,.F.,(3,3),(0.,1.),.UNSPECIFIED.);
#935=B_SPLINE_CURVE_WITH_KNOTS('',2,(#45119,#45120,#45121),
 .UNSPECIFIED.,.F.,.F.,(3,3),(0.,1.),.UNSPECIFIED.);
#936=B_SPLINE_CURVE_WITH_KNOTS('',2,(#45129,#45130,#45131),
 .UNSPECIFIED.,.F.,.F.,(3,3),(0.,1.),.UNSPECIFIED.);
#937=B_SPLINE_CURVE_WITH_KNOTS('',2,(#45134,#45135,#45136),
 .UNSPECIFIED.,.F.,.F.,(3,3),(0.,1.),.UNSPECIFIED.);
#938=B_SPLINE_CURVE_WITH_KNOTS('',2,(#45144,#45145,#45146),
 .UNSPECIFIED.,.F.,.F.,(3,3),(0.,1.),.UNSPECIFIED.);
#939=B_SPLINE_CURVE_WITH_KNOTS('',2,(#45149,#45150,#45151),
 .UNSPECIFIED.,.F.,.F.,(3,3),(0.,1.),.UNSPECIFIED.);
#940=B_SPLINE_CURVE_WITH_KNOTS('',2,(#45159,#45160,#45161),
 .UNSPECIFIED.,.F.,.F.,(3,3),(0.,1.),.UNSPECIFIED.);
#941=B_SPLINE_CURVE_WITH_KNOTS('',2,(#45164,#45165,#45166),
 .UNSPECIFIED.,.F.,.F.,(3,3),(0.,1.),.UNSPECIFIED.);
#942=B_SPLINE_CURVE_WITH_KNOTS('',2,(#45174,#45175,#45176),
 .UNSPECIFIED.,.F.,.F.,(3,3),(0.,1.),.UNSPECIFIED.);
#943=B_SPLINE_CURVE_WITH_KNOTS('',2,(#45179,#45180,#45181),
 .UNSPECIFIED.,.F.,.F.,(3,3),(0.,1.),.UNSPECIFIED.);
#944=B_SPLINE_CURVE_WITH_KNOTS('',2,(#45189,#45190,#45191),
 .UNSPECIFIED.,.F.,.F.,(3,3),(0.,1.),.UNSPECIFIED.);
#945=B_SPLINE_CURVE_WITH_KNOTS('',2,(#45194,#45195,#45196),
 .UNSPECIFIED.,.F.,.F.,(3,3),(0.,1.),.UNSPECIFIED.);
#946=B_SPLINE_CURVE_WITH_KNOTS('',2,(#45204,#45205,#45206),
 .UNSPECIFIED.,.F.,.F.,(3,3),(0.,1.),.UNSPECIFIED.);
#947=B_SPLINE_CURVE_WITH_KNOTS('',2,(#45209,#45210,#45211),
 .UNSPECIFIED.,.F.,.F.,(3,3),(0.,1.),.UNSPECIFIED.);
#948=B_SPLINE_CURVE_WITH_KNOTS('',2,(#45219,#45220,#45221),
 .UNSPECIFIED.,.F.,.F.,(3,3),(0.,1.),.UNSPECIFIED.);
#949=B_SPLINE_CURVE_WITH_KNOTS('',2,(#45224,#45225,#45226),
 .UNSPECIFIED.,.F.,.F.,(3,3),(0.,1.),.UNSPECIFIED.);
#950=B_SPLINE_CURVE_WITH_KNOTS('',2,(#45234,#45235,#45236),
 .UNSPECIFIED.,.F.,.F.,(3,3),(0.,1.),.UNSPECIFIED.);
#951=B_SPLINE_CURVE_WITH_KNOTS('',2,(#45239,#45240,#45241),
 .UNSPECIFIED.,.F.,.F.,(3,3),(0.,1.),.UNSPECIFIED.);
#952=B_SPLINE_CURVE_WITH_KNOTS('',2,(#45249,#45250,#45251),
 .UNSPECIFIED.,.F.,.F.,(3,3),(0.,1.),.UNSPECIFIED.);
#953=B_SPLINE_CURVE_WITH_KNOTS('',2,(#45254,#45255,#45256),
 .UNSPECIFIED.,.F.,.F.,(3,3),(0.,1.),.UNSPECIFIED.);
#954=B_SPLINE_CURVE_WITH_KNOTS('',2,(#45270,#45271,#45272),
 .UNSPECIFIED.,.F.,.F.,(3,3),(0.,1.),.UNSPECIFIED.);
#955=B_SPLINE_CURVE_WITH_KNOTS('',2,(#45275,#45276,#45277),
 .UNSPECIFIED.,.F.,.F.,(3,3),(0.,1.),.UNSPECIFIED.);
#956=B_SPLINE_CURVE_WITH_KNOTS('',2,(#45284,#45285,#45286),
 .UNSPECIFIED.,.F.,.F.,(3,3),(0.,1.),.UNSPECIFIED.);
#957=B_SPLINE_CURVE_WITH_KNOTS('',2,(#45287,#45288,#45289),
 .UNSPECIFIED.,.F.,.F.,(3,3),(0.,1.),.UNSPECIFIED.);
#958=B_SPLINE_CURVE_WITH_KNOTS('',2,(#45299,#45300,#45301),
 .UNSPECIFIED.,.F.,.F.,(3,3),(0.,1.),.UNSPECIFIED.);
#959=B_SPLINE_CURVE_WITH_KNOTS('',2,(#45305,#45306,#45307),
 .UNSPECIFIED.,.F.,.F.,(3,3),(0.,1.),.UNSPECIFIED.);
#960=B_SPLINE_CURVE_WITH_KNOTS('',2,(#45316,#45317,#45318),
 .UNSPECIFIED.,.F.,.F.,(3,3),(0.,1.),.UNSPECIFIED.);
#961=B_SPLINE_CURVE_WITH_KNOTS('',2,(#45321,#45322,#45323),
 .UNSPECIFIED.,.F.,.F.,(3,3),(0.,1.),.UNSPECIFIED.);
#962=B_SPLINE_CURVE_WITH_KNOTS('',2,(#45331,#45332,#45333),
 .UNSPECIFIED.,.F.,.F.,(3,3),(0.,1.),.UNSPECIFIED.);
#963=B_SPLINE_CURVE_WITH_KNOTS('',2,(#45336,#45337,#45338),
 .UNSPECIFIED.,.F.,.F.,(3,3),(0.,1.),.UNSPECIFIED.);
#964=B_SPLINE_CURVE_WITH_KNOTS('',2,(#45346,#45347,#45348),
 .UNSPECIFIED.,.F.,.F.,(3,3),(0.,1.),.UNSPECIFIED.);
#965=B_SPLINE_CURVE_WITH_KNOTS('',2,(#45351,#45352,#45353),
 .UNSPECIFIED.,.F.,.F.,(3,3),(0.,1.),.UNSPECIFIED.);
#966=B_SPLINE_CURVE_WITH_KNOTS('',2,(#45361,#45362,#45363),
 .UNSPECIFIED.,.F.,.F.,(3,3),(0.,1.),.UNSPECIFIED.);
#967=B_SPLINE_CURVE_WITH_KNOTS('',2,(#45366,#45367,#45368),
 .UNSPECIFIED.,.F.,.F.,(3,3),(0.,1.),.UNSPECIFIED.);
#968=B_SPLINE_CURVE_WITH_KNOTS('',2,(#45376,#45377,#45378),
 .UNSPECIFIED.,.F.,.F.,(3,3),(0.,1.),.UNSPECIFIED.);
#969=B_SPLINE_CURVE_WITH_KNOTS('',2,(#45381,#45382,#45383),
 .UNSPECIFIED.,.F.,.F.,(3,3),(0.,1.),.UNSPECIFIED.);
#970=B_SPLINE_CURVE_WITH_KNOTS('',2,(#45391,#45392,#45393),
 .UNSPECIFIED.,.F.,.F.,(3,3),(0.,1.),.UNSPECIFIED.);
#971=B_SPLINE_CURVE_WITH_KNOTS('',2,(#45396,#45397,#45398),
 .UNSPECIFIED.,.F.,.F.,(3,3),(0.,1.),.UNSPECIFIED.);
#972=B_SPLINE_CURVE_WITH_KNOTS('',2,(#45406,#45407,#45408),
 .UNSPECIFIED.,.F.,.F.,(3,3),(0.,1.),.UNSPECIFIED.);
#973=B_SPLINE_CURVE_WITH_KNOTS('',2,(#45411,#45412,#45413),
 .UNSPECIFIED.,.F.,.F.,(3,3),(0.,1.),.UNSPECIFIED.);
#974=B_SPLINE_CURVE_WITH_KNOTS('',2,(#45421,#45422,#45423),
 .UNSPECIFIED.,.F.,.F.,(3,3),(0.,1.),.UNSPECIFIED.);
#975=B_SPLINE_CURVE_WITH_KNOTS('',2,(#45426,#45427,#45428),
 .UNSPECIFIED.,.F.,.F.,(3,3),(0.,1.),.UNSPECIFIED.);
#976=B_SPLINE_CURVE_WITH_KNOTS('',2,(#45436,#45437,#45438),
 .UNSPECIFIED.,.F.,.F.,(3,3),(0.,1.),.UNSPECIFIED.);
#977=B_SPLINE_CURVE_WITH_KNOTS('',2,(#45441,#45442,#45443),
 .UNSPECIFIED.,.F.,.F.,(3,3),(0.,1.),.UNSPECIFIED.);
#978=B_SPLINE_CURVE_WITH_KNOTS('',2,(#45451,#45452,#45453),
 .UNSPECIFIED.,.F.,.F.,(3,3),(0.,1.),.UNSPECIFIED.);
#979=B_SPLINE_CURVE_WITH_KNOTS('',2,(#45456,#45457,#45458),
 .UNSPECIFIED.,.F.,.F.,(3,3),(0.,1.),.UNSPECIFIED.);
#980=B_SPLINE_CURVE_WITH_KNOTS('',2,(#45472,#45473,#45474),
 .UNSPECIFIED.,.F.,.F.,(3,3),(0.,1.),.UNSPECIFIED.);
#981=B_SPLINE_CURVE_WITH_KNOTS('',2,(#45477,#45478,#45479),
 .UNSPECIFIED.,.F.,.F.,(3,3),(0.,1.),.UNSPECIFIED.);
#982=B_SPLINE_CURVE_WITH_KNOTS('',2,(#45487,#45488,#45489),
 .UNSPECIFIED.,.F.,.F.,(3,3),(0.,1.),.UNSPECIFIED.);
#983=B_SPLINE_CURVE_WITH_KNOTS('',2,(#45492,#45493,#45494),
 .UNSPECIFIED.,.F.,.F.,(3,3),(0.,1.),.UNSPECIFIED.);
#984=B_SPLINE_CURVE_WITH_KNOTS('',2,(#45502,#45503,#45504),
 .UNSPECIFIED.,.F.,.F.,(3,3),(0.,1.),.UNSPECIFIED.);
#985=B_SPLINE_CURVE_WITH_KNOTS('',2,(#45507,#45508,#45509),
 .UNSPECIFIED.,.F.,.F.,(3,3),(0.,1.),.UNSPECIFIED.);
#986=B_SPLINE_CURVE_WITH_KNOTS('',2,(#45517,#45518,#45519),
 .UNSPECIFIED.,.F.,.F.,(3,3),(0.,1.),.UNSPECIFIED.);
#987=B_SPLINE_CURVE_WITH_KNOTS('',2,(#45522,#45523,#45524),
 .UNSPECIFIED.,.F.,.F.,(3,3),(0.,1.),.UNSPECIFIED.);
#988=B_SPLINE_CURVE_WITH_KNOTS('',2,(#45532,#45533,#45534),
 .UNSPECIFIED.,.F.,.F.,(3,3),(0.,1.),.UNSPECIFIED.);
#989=B_SPLINE_CURVE_WITH_KNOTS('',2,(#45537,#45538,#45539),
 .UNSPECIFIED.,.F.,.F.,(3,3),(0.,1.),.UNSPECIFIED.);
#990=B_SPLINE_CURVE_WITH_KNOTS('',2,(#45547,#45548,#45549),
 .UNSPECIFIED.,.F.,.F.,(3,3),(0.,1.),.UNSPECIFIED.);
#991=B_SPLINE_CURVE_WITH_KNOTS('',2,(#45552,#45553,#45554),
 .UNSPECIFIED.,.F.,.F.,(3,3),(0.,1.),.UNSPECIFIED.);
#992=B_SPLINE_CURVE_WITH_KNOTS('',2,(#45562,#45563,#45564),
 .UNSPECIFIED.,.F.,.F.,(3,3),(0.,1.),.UNSPECIFIED.);
#993=B_SPLINE_CURVE_WITH_KNOTS('',2,(#45567,#45568,#45569),
 .UNSPECIFIED.,.F.,.F.,(3,3),(0.,1.),.UNSPECIFIED.);
#994=B_SPLINE_CURVE_WITH_KNOTS('',2,(#45583,#45584,#45585),
 .UNSPECIFIED.,.F.,.F.,(3,3),(0.,1.),.UNSPECIFIED.);
#995=B_SPLINE_CURVE_WITH_KNOTS('',2,(#45588,#45589,#45590),
 .UNSPECIFIED.,.F.,.F.,(3,3),(0.,1.),.UNSPECIFIED.);
#996=B_SPLINE_CURVE_WITH_KNOTS('',2,(#45598,#45599,#45600),
 .UNSPECIFIED.,.F.,.F.,(3,3),(0.,1.),.UNSPECIFIED.);
#997=B_SPLINE_CURVE_WITH_KNOTS('',2,(#45603,#45604,#45605),
 .UNSPECIFIED.,.F.,.F.,(3,3),(0.,1.),.UNSPECIFIED.);
#998=B_SPLINE_CURVE_WITH_KNOTS('',2,(#45613,#45614,#45615),
 .UNSPECIFIED.,.F.,.F.,(3,3),(0.,1.),.UNSPECIFIED.);
#999=B_SPLINE_CURVE_WITH_KNOTS('',2,(#45618,#45619,#45620),
 .UNSPECIFIED.,.F.,.F.,(3,3),(0.,1.),.UNSPECIFIED.);
#1000=B_SPLINE_CURVE_WITH_KNOTS('',2,(#45628,#45629,#45630),
 .UNSPECIFIED.,.F.,.F.,(3,3),(0.,1.),.UNSPECIFIED.);
#1001=B_SPLINE_CURVE_WITH_KNOTS('',2,(#45633,#45634,#45635),
 .UNSPECIFIED.,.F.,.F.,(3,3),(0.,1.),.UNSPECIFIED.);
#1002=B_SPLINE_CURVE_WITH_KNOTS('',2,(#45643,#45644,#45645),
 .UNSPECIFIED.,.F.,.F.,(3,3),(0.,1.),.UNSPECIFIED.);
#1003=B_SPLINE_CURVE_WITH_KNOTS('',2,(#45648,#45649,#45650),
 .UNSPECIFIED.,.F.,.F.,(3,3),(0.,1.),.UNSPECIFIED.);
#1004=B_SPLINE_CURVE_WITH_KNOTS('',2,(#45658,#45659,#45660),
 .UNSPECIFIED.,.F.,.F.,(3,3),(0.,1.),.UNSPECIFIED.);
#1005=B_SPLINE_CURVE_WITH_KNOTS('',2,(#45663,#45664,#45665),
 .UNSPECIFIED.,.F.,.F.,(3,3),(0.,1.),.UNSPECIFIED.);
#1006=B_SPLINE_CURVE_WITH_KNOTS('',2,(#45673,#45674,#45675),
 .UNSPECIFIED.,.F.,.F.,(3,3),(0.,1.),.UNSPECIFIED.);
#1007=B_SPLINE_CURVE_WITH_KNOTS('',2,(#45678,#45679,#45680),
 .UNSPECIFIED.,.F.,.F.,(3,3),(0.,1.),.UNSPECIFIED.);
#1008=B_SPLINE_CURVE_WITH_KNOTS('',2,(#45694,#45695,#45696),
 .UNSPECIFIED.,.F.,.F.,(3,3),(0.,1.),.UNSPECIFIED.);
#1009=B_SPLINE_CURVE_WITH_KNOTS('',2,(#45699,#45700,#45701),
 .UNSPECIFIED.,.F.,.F.,(3,3),(0.,1.),.UNSPECIFIED.);
#1010=B_SPLINE_CURVE_WITH_KNOTS('',2,(#45708,#45709,#45710),
 .UNSPECIFIED.,.F.,.F.,(3,3),(0.,1.),.UNSPECIFIED.);
#1011=B_SPLINE_CURVE_WITH_KNOTS('',2,(#45711,#45712,#45713),
 .UNSPECIFIED.,.F.,.F.,(3,3),(0.,1.),.UNSPECIFIED.);
#1012=B_SPLINE_CURVE_WITH_KNOTS('',2,(#45723,#45724,#45725),
 .UNSPECIFIED.,.F.,.F.,(3,3),(0.,1.),.UNSPECIFIED.);
#1013=B_SPLINE_CURVE_WITH_KNOTS('',2,(#45729,#45730,#45731),
 .UNSPECIFIED.,.F.,.F.,(3,3),(0.,1.),.UNSPECIFIED.);
#1014=B_SPLINE_CURVE_WITH_KNOTS('',2,(#45740,#45741,#45742),
 .UNSPECIFIED.,.F.,.F.,(3,3),(0.,1.),.UNSPECIFIED.);
#1015=B_SPLINE_CURVE_WITH_KNOTS('',2,(#45745,#45746,#45747),
 .UNSPECIFIED.,.F.,.F.,(3,3),(0.,1.),.UNSPECIFIED.);
#1016=B_SPLINE_CURVE_WITH_KNOTS('',2,(#45755,#45756,#45757),
 .UNSPECIFIED.,.F.,.F.,(3,3),(0.,1.),.UNSPECIFIED.);
#1017=B_SPLINE_CURVE_WITH_KNOTS('',2,(#45760,#45761,#45762),
 .UNSPECIFIED.,.F.,.F.,(3,3),(0.,1.),.UNSPECIFIED.);
#1018=B_SPLINE_CURVE_WITH_KNOTS('',2,(#45770,#45771,#45772),
 .UNSPECIFIED.,.F.,.F.,(3,3),(0.,1.),.UNSPECIFIED.);
#1019=B_SPLINE_CURVE_WITH_KNOTS('',2,(#45775,#45776,#45777),
 .UNSPECIFIED.,.F.,.F.,(3,3),(0.,1.),.UNSPECIFIED.);
#1020=B_SPLINE_CURVE_WITH_KNOTS('',2,(#45785,#45786,#45787),
 .UNSPECIFIED.,.F.,.F.,(3,3),(0.,1.),.UNSPECIFIED.);
#1021=B_SPLINE_CURVE_WITH_KNOTS('',2,(#45790,#45791,#45792),
 .UNSPECIFIED.,.F.,.F.,(3,3),(0.,1.),.UNSPECIFIED.);
#1022=B_SPLINE_CURVE_WITH_KNOTS('',2,(#45800,#45801,#45802),
 .UNSPECIFIED.,.F.,.F.,(3,3),(0.,1.),.UNSPECIFIED.);
#1023=B_SPLINE_CURVE_WITH_KNOTS('',2,(#45805,#45806,#45807),
 .UNSPECIFIED.,.F.,.F.,(3,3),(0.,1.),.UNSPECIFIED.);
#1024=B_SPLINE_CURVE_WITH_KNOTS('',2,(#45815,#45816,#45817),
 .UNSPECIFIED.,.F.,.F.,(3,3),(0.,1.),.UNSPECIFIED.);
#1025=B_SPLINE_CURVE_WITH_KNOTS('',2,(#45820,#45821,#45822),
 .UNSPECIFIED.,.F.,.F.,(3,3),(0.,1.),.UNSPECIFIED.);
#1026=B_SPLINE_CURVE_WITH_KNOTS('',2,(#45830,#45831,#45832),
 .UNSPECIFIED.,.F.,.F.,(3,3),(0.,1.),.UNSPECIFIED.);
#1027=B_SPLINE_CURVE_WITH_KNOTS('',2,(#45835,#45836,#45837),
 .UNSPECIFIED.,.F.,.F.,(3,3),(0.,1.),.UNSPECIFIED.);
#1028=B_SPLINE_CURVE_WITH_KNOTS('',2,(#45851,#45852,#45853),
 .UNSPECIFIED.,.F.,.F.,(3,3),(0.,1.),.UNSPECIFIED.);
#1029=B_SPLINE_CURVE_WITH_KNOTS('',2,(#45856,#45857,#45858),
 .UNSPECIFIED.,.F.,.F.,(3,3),(0.,1.),.UNSPECIFIED.);
#1030=B_SPLINE_CURVE_WITH_KNOTS('',2,(#45866,#45867,#45868),
 .UNSPECIFIED.,.F.,.F.,(3,3),(0.,1.),.UNSPECIFIED.);
#1031=B_SPLINE_CURVE_WITH_KNOTS('',2,(#45871,#45872,#45873),
 .UNSPECIFIED.,.F.,.F.,(3,3),(0.,1.),.UNSPECIFIED.);
#1032=B_SPLINE_CURVE_WITH_KNOTS('',2,(#45881,#45882,#45883),
 .UNSPECIFIED.,.F.,.F.,(3,3),(0.,1.),.UNSPECIFIED.);
#1033=B_SPLINE_CURVE_WITH_KNOTS('',2,(#45886,#45887,#45888),
 .UNSPECIFIED.,.F.,.F.,(3,3),(0.,1.),.UNSPECIFIED.);
#1034=B_SPLINE_CURVE_WITH_KNOTS('',2,(#45896,#45897,#45898),
 .UNSPECIFIED.,.F.,.F.,(3,3),(0.,1.),.UNSPECIFIED.);
#1035=B_SPLINE_CURVE_WITH_KNOTS('',2,(#45901,#45902,#45903),
 .UNSPECIFIED.,.F.,.F.,(3,3),(0.,1.),.UNSPECIFIED.);
#1036=B_SPLINE_CURVE_WITH_KNOTS('',2,(#45911,#45912,#45913),
 .UNSPECIFIED.,.F.,.F.,(3,3),(0.,1.),.UNSPECIFIED.);
#1037=B_SPLINE_CURVE_WITH_KNOTS('',2,(#45916,#45917,#45918),
 .UNSPECIFIED.,.F.,.F.,(3,3),(0.,1.),.UNSPECIFIED.);
#1038=B_SPLINE_CURVE_WITH_KNOTS('',2,(#45926,#45927,#45928),
 .UNSPECIFIED.,.F.,.F.,(3,3),(0.,1.),.UNSPECIFIED.);
#1039=B_SPLINE_CURVE_WITH_KNOTS('',2,(#45931,#45932,#45933),
 .UNSPECIFIED.,.F.,.F.,(3,3),(0.,1.),.UNSPECIFIED.);
#1040=B_SPLINE_CURVE_WITH_KNOTS('',2,(#45941,#45942,#45943),
 .UNSPECIFIED.,.F.,.F.,(3,3),(0.,1.),.UNSPECIFIED.);
#1041=B_SPLINE_CURVE_WITH_KNOTS('',2,(#45946,#45947,#45948),
 .UNSPECIFIED.,.F.,.F.,(3,3),(0.,1.),.UNSPECIFIED.);
#1042=B_SPLINE_CURVE_WITH_KNOTS('',2,(#45956,#45957,#45958),
 .UNSPECIFIED.,.F.,.F.,(3,3),(0.,1.),.UNSPECIFIED.);
#1043=B_SPLINE_CURVE_WITH_KNOTS('',2,(#45961,#45962,#45963),
 .UNSPECIFIED.,.F.,.F.,(3,3),(0.,1.),.UNSPECIFIED.);
#1044=B_SPLINE_CURVE_WITH_KNOTS('',2,(#45971,#45972,#45973),
 .UNSPECIFIED.,.F.,.F.,(3,3),(0.,1.),.UNSPECIFIED.);
#1045=B_SPLINE_CURVE_WITH_KNOTS('',2,(#45976,#45977,#45978),
 .UNSPECIFIED.,.F.,.F.,(3,3),(0.,1.),.UNSPECIFIED.);
#1046=B_SPLINE_CURVE_WITH_KNOTS('',2,(#46003,#46004,#46005),
 .UNSPECIFIED.,.F.,.F.,(3,3),(0.,1.),.UNSPECIFIED.);
#1047=B_SPLINE_CURVE_WITH_KNOTS('',2,(#46006,#46007,#46008),
 .UNSPECIFIED.,.F.,.F.,(3,3),(0.,1.),.UNSPECIFIED.);
#1048=B_SPLINE_CURVE_WITH_KNOTS('',2,(#46026,#46027,#46028),
 .UNSPECIFIED.,.F.,.F.,(3,3),(0.,1.),.UNSPECIFIED.);
#1049=B_SPLINE_CURVE_WITH_KNOTS('',2,(#46031,#46032,#46033),
 .UNSPECIFIED.,.F.,.F.,(3,3),(0.,1.),.UNSPECIFIED.);
#1050=B_SPLINE_CURVE_WITH_KNOTS('',2,(#46041,#46042,#46043),
 .UNSPECIFIED.,.F.,.F.,(3,3),(0.,1.),.UNSPECIFIED.);
#1051=B_SPLINE_CURVE_WITH_KNOTS('',2,(#46046,#46047,#46048),
 .UNSPECIFIED.,.F.,.F.,(3,3),(0.,1.),.UNSPECIFIED.);
#1052=B_SPLINE_CURVE_WITH_KNOTS('',2,(#46056,#46057,#46058),
 .UNSPECIFIED.,.F.,.F.,(3,3),(0.,1.),.UNSPECIFIED.);
#1053=B_SPLINE_CURVE_WITH_KNOTS('',2,(#46061,#46062,#46063),
 .UNSPECIFIED.,.F.,.F.,(3,3),(0.,1.),.UNSPECIFIED.);
#1054=B_SPLINE_CURVE_WITH_KNOTS('',2,(#46071,#46072,#46073),
 .UNSPECIFIED.,.F.,.F.,(3,3),(0.,1.),.UNSPECIFIED.);
#1055=B_SPLINE_CURVE_WITH_KNOTS('',2,(#46076,#46077,#46078),
 .UNSPECIFIED.,.F.,.F.,(3,3),(0.,1.),.UNSPECIFIED.);
#1056=B_SPLINE_CURVE_WITH_KNOTS('',2,(#46086,#46087,#46088),
 .UNSPECIFIED.,.F.,.F.,(3,3),(0.,1.),.UNSPECIFIED.);
#1057=B_SPLINE_CURVE_WITH_KNOTS('',2,(#46091,#46092,#46093),
 .UNSPECIFIED.,.F.,.F.,(3,3),(0.,1.),.UNSPECIFIED.);
#1058=B_SPLINE_CURVE_WITH_KNOTS('',2,(#46119,#46120,#46121),
 .UNSPECIFIED.,.F.,.F.,(3,3),(0.,1.),.UNSPECIFIED.);
#1059=B_SPLINE_CURVE_WITH_KNOTS('',2,(#46124,#46125,#46126),
 .UNSPECIFIED.,.F.,.F.,(3,3),(0.,1.),.UNSPECIFIED.);
#1060=B_SPLINE_CURVE_WITH_KNOTS('',2,(#46134,#46135,#46136),
 .UNSPECIFIED.,.F.,.F.,(3,3),(0.,1.),.UNSPECIFIED.);
#1061=B_SPLINE_CURVE_WITH_KNOTS('',2,(#46139,#46140,#46141),
 .UNSPECIFIED.,.F.,.F.,(3,3),(0.,1.),.UNSPECIFIED.);
#1062=B_SPLINE_CURVE_WITH_KNOTS('',2,(#46149,#46150,#46151),
 .UNSPECIFIED.,.F.,.F.,(3,3),(0.,1.),.UNSPECIFIED.);
#1063=B_SPLINE_CURVE_WITH_KNOTS('',2,(#46154,#46155,#46156),
 .UNSPECIFIED.,.F.,.F.,(3,3),(0.,1.),.UNSPECIFIED.);
#1064=B_SPLINE_CURVE_WITH_KNOTS('',2,(#46164,#46165,#46166),
 .UNSPECIFIED.,.F.,.F.,(3,3),(0.,1.),.UNSPECIFIED.);
#1065=B_SPLINE_CURVE_WITH_KNOTS('',2,(#46169,#46170,#46171),
 .UNSPECIFIED.,.F.,.F.,(3,3),(0.,1.),.UNSPECIFIED.);
#1066=B_SPLINE_CURVE_WITH_KNOTS('',2,(#46179,#46180,#46181),
 .UNSPECIFIED.,.F.,.F.,(3,3),(0.,1.),.UNSPECIFIED.);
#1067=B_SPLINE_CURVE_WITH_KNOTS('',2,(#46184,#46185,#46186),
 .UNSPECIFIED.,.F.,.F.,(3,3),(0.,1.),.UNSPECIFIED.);
#1068=B_SPLINE_CURVE_WITH_KNOTS('',2,(#46194,#46195,#46196),
 .UNSPECIFIED.,.F.,.F.,(3,3),(0.,1.),.UNSPECIFIED.);
#1069=B_SPLINE_CURVE_WITH_KNOTS('',2,(#46199,#46200,#46201),
 .UNSPECIFIED.,.F.,.F.,(3,3),(0.,1.),.UNSPECIFIED.);
#1070=B_SPLINE_CURVE_WITH_KNOTS('',2,(#46232,#46233,#46234),
 .UNSPECIFIED.,.F.,.F.,(3,3),(0.,1.),.UNSPECIFIED.);
#1071=B_SPLINE_CURVE_WITH_KNOTS('',2,(#46238,#46239,#46240),
 .UNSPECIFIED.,.F.,.F.,(3,3),(0.,1.),.UNSPECIFIED.);
#1072=B_SPLINE_CURVE_WITH_KNOTS('',2,(#46249,#46250,#46251),
 .UNSPECIFIED.,.F.,.F.,(3,3),(0.,1.),.UNSPECIFIED.);
#1073=B_SPLINE_CURVE_WITH_KNOTS('',2,(#46254,#46255,#46256),
 .UNSPECIFIED.,.F.,.F.,(3,3),(0.,1.),.UNSPECIFIED.);
#1074=B_SPLINE_CURVE_WITH_KNOTS('',2,(#46264,#46265,#46266),
 .UNSPECIFIED.,.F.,.F.,(3,3),(0.,1.),.UNSPECIFIED.);
#1075=B_SPLINE_CURVE_WITH_KNOTS('',2,(#46269,#46270,#46271),
 .UNSPECIFIED.,.F.,.F.,(3,3),(0.,1.),.UNSPECIFIED.);
#1076=B_SPLINE_CURVE_WITH_KNOTS('',2,(#46279,#46280,#46281),
 .UNSPECIFIED.,.F.,.F.,(3,3),(0.,1.),.UNSPECIFIED.);
#1077=B_SPLINE_CURVE_WITH_KNOTS('',2,(#46284,#46285,#46286),
 .UNSPECIFIED.,.F.,.F.,(3,3),(0.,1.),.UNSPECIFIED.);
#1078=B_SPLINE_CURVE_WITH_KNOTS('',2,(#46294,#46295,#46296),
 .UNSPECIFIED.,.F.,.F.,(3,3),(0.,1.),.UNSPECIFIED.);
#1079=B_SPLINE_CURVE_WITH_KNOTS('',2,(#46299,#46300,#46301),
 .UNSPECIFIED.,.F.,.F.,(3,3),(0.,1.),.UNSPECIFIED.);
#1080=B_SPLINE_CURVE_WITH_KNOTS('',2,(#46309,#46310,#46311),
 .UNSPECIFIED.,.F.,.F.,(3,3),(0.,1.),.UNSPECIFIED.);
#1081=B_SPLINE_CURVE_WITH_KNOTS('',2,(#46314,#46315,#46316),
 .UNSPECIFIED.,.F.,.F.,(3,3),(0.,1.),.UNSPECIFIED.);
#1082=B_SPLINE_CURVE_WITH_KNOTS('',2,(#46324,#46325,#46326),
 .UNSPECIFIED.,.F.,.F.,(3,3),(0.,1.),.UNSPECIFIED.);
#1083=B_SPLINE_CURVE_WITH_KNOTS('',2,(#46329,#46330,#46331),
 .UNSPECIFIED.,.F.,.F.,(3,3),(0.,1.),.UNSPECIFIED.);
#1084=B_SPLINE_CURVE_WITH_KNOTS('',2,(#46339,#46340,#46341),
 .UNSPECIFIED.,.F.,.F.,(3,3),(0.,1.),.UNSPECIFIED.);
#1085=B_SPLINE_CURVE_WITH_KNOTS('',2,(#46344,#46345,#46346),
 .UNSPECIFIED.,.F.,.F.,(3,3),(0.,1.),.UNSPECIFIED.);
#1086=B_SPLINE_CURVE_WITH_KNOTS('',2,(#46353,#46354,#46355),
 .UNSPECIFIED.,.F.,.F.,(3,3),(0.,1.),.UNSPECIFIED.);
#1087=B_SPLINE_CURVE_WITH_KNOTS('',2,(#46356,#46357,#46358),
 .UNSPECIFIED.,.F.,.F.,(3,3),(0.,1.),.UNSPECIFIED.);
#1088=B_SPLINE_CURVE_WITH_KNOTS('',2,(#46367,#46368,#46369),
 .UNSPECIFIED.,.F.,.F.,(3,3),(0.,1.),.UNSPECIFIED.);
#1089=B_SPLINE_CURVE_WITH_KNOTS('',2,(#46373,#46374,#46375),
 .UNSPECIFIED.,.F.,.F.,(3,3),(0.,1.),.UNSPECIFIED.);
#1090=B_SPLINE_CURVE_WITH_KNOTS('',2,(#46384,#46385,#46386),
 .UNSPECIFIED.,.F.,.F.,(3,3),(0.,1.),.UNSPECIFIED.);
#1091=B_SPLINE_CURVE_WITH_KNOTS('',2,(#46389,#46390,#46391),
 .UNSPECIFIED.,.F.,.F.,(3,3),(0.,1.),.UNSPECIFIED.);
#1092=B_SPLINE_CURVE_WITH_KNOTS('',2,(#46399,#46400,#46401),
 .UNSPECIFIED.,.F.,.F.,(3,3),(0.,1.),.UNSPECIFIED.);
#1093=B_SPLINE_CURVE_WITH_KNOTS('',2,(#46404,#46405,#46406),
 .UNSPECIFIED.,.F.,.F.,(3,3),(0.,1.),.UNSPECIFIED.);
#1094=B_SPLINE_CURVE_WITH_KNOTS('',2,(#46414,#46415,#46416),
 .UNSPECIFIED.,.F.,.F.,(3,3),(0.,1.),.UNSPECIFIED.);
#1095=B_SPLINE_CURVE_WITH_KNOTS('',2,(#46419,#46420,#46421),
 .UNSPECIFIED.,.F.,.F.,(3,3),(0.,1.),.UNSPECIFIED.);
#1096=B_SPLINE_CURVE_WITH_KNOTS('',2,(#46429,#46430,#46431),
 .UNSPECIFIED.,.F.,.F.,(3,3),(0.,1.),.UNSPECIFIED.);
#1097=B_SPLINE_CURVE_WITH_KNOTS('',2,(#46434,#46435,#46436),
 .UNSPECIFIED.,.F.,.F.,(3,3),(0.,1.),.UNSPECIFIED.);
#1098=B_SPLINE_CURVE_WITH_KNOTS('',2,(#46444,#46445,#46446),
 .UNSPECIFIED.,.F.,.F.,(3,3),(0.,1.),.UNSPECIFIED.);
#1099=B_SPLINE_CURVE_WITH_KNOTS('',2,(#46449,#46450,#46451),
 .UNSPECIFIED.,.F.,.F.,(3,3),(0.,1.),.UNSPECIFIED.);
#1100=B_SPLINE_CURVE_WITH_KNOTS('',2,(#46459,#46460,#46461),
 .UNSPECIFIED.,.F.,.F.,(3,3),(0.,1.),.UNSPECIFIED.);
#1101=B_SPLINE_CURVE_WITH_KNOTS('',2,(#46464,#46465,#46466),
 .UNSPECIFIED.,.F.,.F.,(3,3),(0.,1.),.UNSPECIFIED.);
#1102=B_SPLINE_CURVE_WITH_KNOTS('',2,(#46474,#46475,#46476),
 .UNSPECIFIED.,.F.,.F.,(3,3),(0.,1.),.UNSPECIFIED.);
#1103=B_SPLINE_CURVE_WITH_KNOTS('',2,(#46479,#46480,#46481),
 .UNSPECIFIED.,.F.,.F.,(3,3),(0.,1.),.UNSPECIFIED.);
#1104=B_SPLINE_CURVE_WITH_KNOTS('',2,(#46489,#46490,#46491),
 .UNSPECIFIED.,.F.,.F.,(3,3),(0.,1.),.UNSPECIFIED.);
#1105=B_SPLINE_CURVE_WITH_KNOTS('',2,(#46494,#46495,#46496),
 .UNSPECIFIED.,.F.,.F.,(3,3),(0.,1.),.UNSPECIFIED.);
#1106=B_SPLINE_CURVE_WITH_KNOTS('',2,(#46504,#46505,#46506),
 .UNSPECIFIED.,.F.,.F.,(3,3),(0.,1.),.UNSPECIFIED.);
#1107=B_SPLINE_CURVE_WITH_KNOTS('',2,(#46509,#46510,#46511),
 .UNSPECIFIED.,.F.,.F.,(3,3),(0.,1.),.UNSPECIFIED.);
#1108=B_SPLINE_CURVE_WITH_KNOTS('',2,(#46519,#46520,#46521),
 .UNSPECIFIED.,.F.,.F.,(3,3),(0.,1.),.UNSPECIFIED.);
#1109=B_SPLINE_CURVE_WITH_KNOTS('',2,(#46524,#46525,#46526),
 .UNSPECIFIED.,.F.,.F.,(3,3),(0.,1.),.UNSPECIFIED.);
#1110=B_SPLINE_CURVE_WITH_KNOTS('',2,(#46534,#46535,#46536),
 .UNSPECIFIED.,.F.,.F.,(3,3),(0.,1.),.UNSPECIFIED.);
#1111=B_SPLINE_CURVE_WITH_KNOTS('',2,(#46539,#46540,#46541),
 .UNSPECIFIED.,.F.,.F.,(3,3),(0.,1.),.UNSPECIFIED.);
#1112=B_SPLINE_CURVE_WITH_KNOTS('',2,(#46549,#46550,#46551),
 .UNSPECIFIED.,.F.,.F.,(3,3),(0.,1.),.UNSPECIFIED.);
#1113=B_SPLINE_CURVE_WITH_KNOTS('',2,(#46554,#46555,#46556),
 .UNSPECIFIED.,.F.,.F.,(3,3),(0.,1.),.UNSPECIFIED.);
#1114=B_SPLINE_CURVE_WITH_KNOTS('',2,(#46564,#46565,#46566),
 .UNSPECIFIED.,.F.,.F.,(3,3),(0.,1.),.UNSPECIFIED.);
#1115=B_SPLINE_CURVE_WITH_KNOTS('',2,(#46569,#46570,#46571),
 .UNSPECIFIED.,.F.,.F.,(3,3),(0.,1.),.UNSPECIFIED.);
#1116=B_SPLINE_CURVE_WITH_KNOTS('',2,(#46579,#46580,#46581),
 .UNSPECIFIED.,.F.,.F.,(3,3),(0.,1.),.UNSPECIFIED.);
#1117=B_SPLINE_CURVE_WITH_KNOTS('',2,(#46584,#46585,#46586),
 .UNSPECIFIED.,.F.,.F.,(3,3),(0.,1.),.UNSPECIFIED.);
#1118=B_SPLINE_CURVE_WITH_KNOTS('',2,(#46594,#46595,#46596),
 .UNSPECIFIED.,.F.,.F.,(3,3),(0.,1.),.UNSPECIFIED.);
#1119=B_SPLINE_CURVE_WITH_KNOTS('',2,(#46599,#46600,#46601),
 .UNSPECIFIED.,.F.,.F.,(3,3),(0.,1.),.UNSPECIFIED.);
#1120=B_SPLINE_CURVE_WITH_KNOTS('',2,(#46615,#46616,#46617),
 .UNSPECIFIED.,.F.,.F.,(3,3),(0.,1.),.UNSPECIFIED.);
#1121=B_SPLINE_CURVE_WITH_KNOTS('',2,(#46620,#46621,#46622),
 .UNSPECIFIED.,.F.,.F.,(3,3),(0.,1.),.UNSPECIFIED.);
#1122=B_SPLINE_CURVE_WITH_KNOTS('',2,(#46629,#46630,#46631),
 .UNSPECIFIED.,.F.,.F.,(3,3),(0.,1.),.UNSPECIFIED.);
#1123=B_SPLINE_CURVE_WITH_KNOTS('',2,(#46632,#46633,#46634),
 .UNSPECIFIED.,.F.,.F.,(3,3),(0.,1.),.UNSPECIFIED.);
#1124=B_SPLINE_CURVE_WITH_KNOTS('',2,(#46644,#46645,#46646),
 .UNSPECIFIED.,.F.,.F.,(3,3),(0.,1.),.UNSPECIFIED.);
#1125=B_SPLINE_CURVE_WITH_KNOTS('',2,(#46650,#46651,#46652),
 .UNSPECIFIED.,.F.,.F.,(3,3),(0.,1.),.UNSPECIFIED.);
#1126=B_SPLINE_CURVE_WITH_KNOTS('',2,(#46661,#46662,#46663),
 .UNSPECIFIED.,.F.,.F.,(3,3),(0.,1.),.UNSPECIFIED.);
#1127=B_SPLINE_CURVE_WITH_KNOTS('',2,(#46666,#46667,#46668),
 .UNSPECIFIED.,.F.,.F.,(3,3),(0.,1.),.UNSPECIFIED.);
#1128=B_SPLINE_CURVE_WITH_KNOTS('',2,(#46676,#46677,#46678),
 .UNSPECIFIED.,.F.,.F.,(3,3),(0.,1.),.UNSPECIFIED.);
#1129=B_SPLINE_CURVE_WITH_KNOTS('',2,(#46681,#46682,#46683),
 .UNSPECIFIED.,.F.,.F.,(3,3),(0.,1.),.UNSPECIFIED.);
#1130=B_SPLINE_CURVE_WITH_KNOTS('',2,(#46691,#46692,#46693),
 .UNSPECIFIED.,.F.,.F.,(3,3),(0.,1.),.UNSPECIFIED.);
#1131=B_SPLINE_CURVE_WITH_KNOTS('',2,(#46696,#46697,#46698),
 .UNSPECIFIED.,.F.,.F.,(3,3),(0.,1.),.UNSPECIFIED.);
#1132=B_SPLINE_CURVE_WITH_KNOTS('',2,(#46706,#46707,#46708),
 .UNSPECIFIED.,.F.,.F.,(3,3),(0.,1.),.UNSPECIFIED.);
#1133=B_SPLINE_CURVE_WITH_KNOTS('',2,(#46711,#46712,#46713),
 .UNSPECIFIED.,.F.,.F.,(3,3),(0.,1.),.UNSPECIFIED.);
#1134=B_SPLINE_CURVE_WITH_KNOTS('',2,(#46721,#46722,#46723),
 .UNSPECIFIED.,.F.,.F.,(3,3),(0.,1.),.UNSPECIFIED.);
#1135=B_SPLINE_CURVE_WITH_KNOTS('',2,(#46726,#46727,#46728),
 .UNSPECIFIED.,.F.,.F.,(3,3),(0.,1.),.UNSPECIFIED.);
#1136=B_SPLINE_CURVE_WITH_KNOTS('',2,(#46736,#46737,#46738),
 .UNSPECIFIED.,.F.,.F.,(3,3),(0.,1.),.UNSPECIFIED.);
#1137=B_SPLINE_CURVE_WITH_KNOTS('',2,(#46741,#46742,#46743),
 .UNSPECIFIED.,.F.,.F.,(3,3),(0.,1.),.UNSPECIFIED.);
#1138=B_SPLINE_CURVE_WITH_KNOTS('',2,(#46750,#46751,#46752),
 .UNSPECIFIED.,.F.,.F.,(3,3),(0.,1.),.UNSPECIFIED.);
#1139=B_SPLINE_CURVE_WITH_KNOTS('',2,(#46753,#46754,#46755),
 .UNSPECIFIED.,.F.,.F.,(3,3),(0.,1.),.UNSPECIFIED.);
#1140=B_SPLINE_CURVE_WITH_KNOTS('',2,(#46764,#46765,#46766),
 .UNSPECIFIED.,.F.,.F.,(3,3),(0.,1.),.UNSPECIFIED.);
#1141=B_SPLINE_CURVE_WITH_KNOTS('',2,(#46770,#46771,#46772),
 .UNSPECIFIED.,.F.,.F.,(3,3),(0.,1.),.UNSPECIFIED.);
#1142=B_SPLINE_CURVE_WITH_KNOTS('',2,(#46781,#46782,#46783),
 .UNSPECIFIED.,.F.,.F.,(3,3),(0.,1.),.UNSPECIFIED.);
#1143=B_SPLINE_CURVE_WITH_KNOTS('',2,(#46786,#46787,#46788),
 .UNSPECIFIED.,.F.,.F.,(3,3),(0.,1.),.UNSPECIFIED.);
#1144=B_SPLINE_CURVE_WITH_KNOTS('',2,(#46796,#46797,#46798),
 .UNSPECIFIED.,.F.,.F.,(3,3),(0.,1.),.UNSPECIFIED.);
#1145=B_SPLINE_CURVE_WITH_KNOTS('',2,(#46801,#46802,#46803),
 .UNSPECIFIED.,.F.,.F.,(3,3),(0.,1.),.UNSPECIFIED.);
#1146=B_SPLINE_CURVE_WITH_KNOTS('',2,(#46811,#46812,#46813),
 .UNSPECIFIED.,.F.,.F.,(3,3),(0.,1.),.UNSPECIFIED.);
#1147=B_SPLINE_CURVE_WITH_KNOTS('',2,(#46816,#46817,#46818),
 .UNSPECIFIED.,.F.,.F.,(3,3),(0.,1.),.UNSPECIFIED.);
#1148=B_SPLINE_CURVE_WITH_KNOTS('',2,(#46826,#46827,#46828),
 .UNSPECIFIED.,.F.,.F.,(3,3),(0.,1.),.UNSPECIFIED.);
#1149=B_SPLINE_CURVE_WITH_KNOTS('',2,(#46831,#46832,#46833),
 .UNSPECIFIED.,.F.,.F.,(3,3),(0.,1.),.UNSPECIFIED.);
#1150=B_SPLINE_CURVE_WITH_KNOTS('',2,(#46841,#46842,#46843),
 .UNSPECIFIED.,.F.,.F.,(3,3),(0.,1.),.UNSPECIFIED.);
#1151=B_SPLINE_CURVE_WITH_KNOTS('',2,(#46846,#46847,#46848),
 .UNSPECIFIED.,.F.,.F.,(3,3),(0.,1.),.UNSPECIFIED.);
#1152=B_SPLINE_CURVE_WITH_KNOTS('',2,(#46856,#46857,#46858),
 .UNSPECIFIED.,.F.,.F.,(3,3),(0.,1.),.UNSPECIFIED.);
#1153=B_SPLINE_CURVE_WITH_KNOTS('',2,(#46861,#46862,#46863),
 .UNSPECIFIED.,.F.,.F.,(3,3),(0.,1.),.UNSPECIFIED.);
#1154=B_SPLINE_CURVE_WITH_KNOTS('',2,(#46900,#46901,#46902),
 .UNSPECIFIED.,.F.,.F.,(3,3),(0.,1.),.UNSPECIFIED.);
#1155=B_SPLINE_CURVE_WITH_KNOTS('',2,(#46903,#46904,#46905),
 .UNSPECIFIED.,.F.,.F.,(3,3),(0.,1.),.UNSPECIFIED.);
#1156=B_SPLINE_CURVE_WITH_KNOTS('',2,(#46915,#46916,#46917),
 .UNSPECIFIED.,.F.,.F.,(3,3),(0.,1.),.UNSPECIFIED.);
#1157=B_SPLINE_CURVE_WITH_KNOTS('',2,(#46921,#46922,#46923),
 .UNSPECIFIED.,.F.,.F.,(3,3),(0.,1.),.UNSPECIFIED.);
#1158=B_SPLINE_CURVE_WITH_KNOTS('',2,(#46932,#46933,#46934),
 .UNSPECIFIED.,.F.,.F.,(3,3),(0.,1.),.UNSPECIFIED.);
#1159=B_SPLINE_CURVE_WITH_KNOTS('',2,(#46937,#46938,#46939),
 .UNSPECIFIED.,.F.,.F.,(3,3),(0.,1.),.UNSPECIFIED.);
#1160=B_SPLINE_CURVE_WITH_KNOTS('',2,(#46947,#46948,#46949),
 .UNSPECIFIED.,.F.,.F.,(3,3),(0.,1.),.UNSPECIFIED.);
#1161=B_SPLINE_CURVE_WITH_KNOTS('',2,(#46952,#46953,#46954),
 .UNSPECIFIED.,.F.,.F.,(3,3),(0.,1.),.UNSPECIFIED.);
#1162=B_SPLINE_CURVE_WITH_KNOTS('',2,(#46962,#46963,#46964),
 .UNSPECIFIED.,.F.,.F.,(3,3),(0.,1.),.UNSPECIFIED.);
#1163=B_SPLINE_CURVE_WITH_KNOTS('',2,(#46967,#46968,#46969),
 .UNSPECIFIED.,.F.,.F.,(3,3),(0.,1.),.UNSPECIFIED.);
#1164=B_SPLINE_CURVE_WITH_KNOTS('',2,(#46983,#46984,#46985),
 .UNSPECIFIED.,.F.,.F.,(3,3),(0.,1.),.UNSPECIFIED.);
#1165=B_SPLINE_CURVE_WITH_KNOTS('',2,(#46988,#46989,#46990),
 .UNSPECIFIED.,.F.,.F.,(3,3),(0.,1.),.UNSPECIFIED.);
#1166=B_SPLINE_CURVE_WITH_KNOTS('',2,(#46998,#46999,#47000),
 .UNSPECIFIED.,.F.,.F.,(3,3),(0.,1.),.UNSPECIFIED.);
#1167=B_SPLINE_CURVE_WITH_KNOTS('',2,(#47003,#47004,#47005),
 .UNSPECIFIED.,.F.,.F.,(3,3),(0.,1.),.UNSPECIFIED.);
#1168=B_SPLINE_CURVE_WITH_KNOTS('',2,(#47013,#47014,#47015),
 .UNSPECIFIED.,.F.,.F.,(3,3),(0.,1.),.UNSPECIFIED.);
#1169=B_SPLINE_CURVE_WITH_KNOTS('',2,(#47018,#47019,#47020),
 .UNSPECIFIED.,.F.,.F.,(3,3),(0.,1.),.UNSPECIFIED.);
#1170=B_SPLINE_CURVE_WITH_KNOTS('',3,(#47061,#47062,#47063,#47064,#47065,
#47066,#47067,#47068,#47069,#47070),.UNSPECIFIED.,.F.,.F.,(4,2,2,2,4),(0.466330361623161,
0.582535633002934,0.698740904382707,0.815700813814515,0.932660723246322),
 .UNSPECIFIED.);
#1171=B_SPLINE_CURVE_WITH_KNOTS('',3,(#47072,#47073,#47074,#47075,#47076,
#47077,#47078,#47079,#47080,#47081),.UNSPECIFIED.,.F.,.F.,(4,2,2,2,4),(0.,
0.116959909431808,0.233919818863615,0.350125090243388,0.466330361623161),
 .UNSPECIFIED.);
#1172=B_SPLINE_CURVE_WITH_KNOTS('',3,(#47083,#47084,#47085,#47086,#47087,
#47088,#47089,#47090,#47091,#47092),.UNSPECIFIED.,.F.,.F.,(4,2,2,2,4),(1.39899108486948,
1.51519635624926,1.63140162762903,1.74836153706084,1.86532144649264),
 .UNSPECIFIED.);
#1173=B_SPLINE_CURVE_WITH_KNOTS('',3,(#47093,#47094,#47095,#47096,#47097,
#47098,#47099,#47100,#47101,#47102),.UNSPECIFIED.,.F.,.F.,(4,2,2,2,4),(0.932660723246322,
1.04962063267813,1.16658054210994,1.28278581348971,1.39899108486948),
 .UNSPECIFIED.);
#1174=B_SPLINE_CURVE_WITH_KNOTS('',3,(#47118,#47119,#47120,#47121,#47122,
#47123,#47124,#47125,#47126,#47127,#47128,#47129,#47130,#47131,#47132,#47133,
#47134,#47135,#47136,#47137,#47138,#47139,#47140,#47141,#47142,#47143),
 .UNSPECIFIED.,.F.,.F.,(4,2,2,2,2,2,2,2,2,2,2,2,4),(1.72309603002439,1.81125279412847,
1.94756976198853,2.21280480266174,2.5211516170085,2.82949843135526,3.44619206004878,
4.06288568874231,4.37123250308907,4.67957931743583,4.94481435810904,5.0811313259691,
5.16928809007318),.UNSPECIFIED.);
#1175=B_SPLINE_CURVE_WITH_KNOTS('',3,(#47413,#47414,#47415,#47416),
 .UNSPECIFIED.,.F.,.F.,(4,4),(1.05088688293601,2.10047487645352),
 .UNSPECIFIED.);
#1176=B_SPLINE_CURVE_WITH_KNOTS('',3,(#47419,#47420,#47421,#47422),
 .UNSPECIFIED.,.F.,.F.,(4,4),(1.06882494380393,2.11841293732144),
 .UNSPECIFIED.);
#1177=B_SPLINE_CURVE_WITH_KNOTS('',3,(#47427,#47428,#47429,#47430),
 .UNSPECIFIED.,.F.,.F.,(4,4),(1.098090767842,2.14756146588325),
 .UNSPECIFIED.);
#1178=B_SPLINE_CURVE_WITH_KNOTS('',3,(#47433,#47434,#47435,#47436),
 .UNSPECIFIED.,.F.,.F.,(4,4),(1.07645732586084,2.12592802390209),
 .UNSPECIFIED.);
#1179=B_SPLINE_CURVE_WITH_KNOTS('',3,(#47441,#47442,#47443,#47444),
 .UNSPECIFIED.,.F.,.F.,(4,4),(1.06876863774445,2.11830775146031),
 .UNSPECIFIED.);
#1180=B_SPLINE_CURVE_WITH_KNOTS('',3,(#47447,#47448,#47449,#47450),
 .UNSPECIFIED.,.F.,.F.,(4,4),(1.07183362023116,2.12137273394702),
 .UNSPECIFIED.);
#1181=B_SPLINE_CURVE_WITH_KNOTS('',3,(#47455,#47456,#47457,#47458),
 .UNSPECIFIED.,.F.,.F.,(4,4),(1.00966173528769,2.0593901610072),
 .UNSPECIFIED.);
#1182=B_SPLINE_CURVE_WITH_KNOTS('',3,(#47461,#47462,#47463,#47464),
 .UNSPECIFIED.,.F.,.F.,(4,4),(1.05659594524126,2.10632437096077),
 .UNSPECIFIED.);
#1183=B_SPLINE_CURVE_WITH_KNOTS('',3,(#47469,#47470,#47471,#47472),
 .UNSPECIFIED.,.F.,.F.,(4,4),(1.03463183846597,2.08427034714712),
 .UNSPECIFIED.);
#1184=B_SPLINE_CURVE_WITH_KNOTS('',3,(#47475,#47476,#47477,#47478),
 .UNSPECIFIED.,.F.,.F.,(4,4),(1.06519471367074,2.1148332223519),
 .UNSPECIFIED.);
#1185=B_SPLINE_CURVE_WITH_KNOTS('',3,(#47483,#47484,#47485,#47486),
 .UNSPECIFIED.,.F.,.F.,(4,4),(1.09726472627115,2.14673867240921),
 .UNSPECIFIED.);
#1186=B_SPLINE_CURVE_WITH_KNOTS('',3,(#47489,#47490,#47491,#47492),
 .UNSPECIFIED.,.F.,.F.,(4,4),(1.07572637127808,2.12520031741614),
 .UNSPECIFIED.);
#1187=B_SPLINE_CURVE_WITH_KNOTS('',3,(#47497,#47498,#47499,#47500),
 .UNSPECIFIED.,.F.,.F.,(4,4),(1.08743350871975,2.13692892862863),
 .UNSPECIFIED.);
#1188=B_SPLINE_CURVE_WITH_KNOTS('',3,(#47503,#47504,#47505,#47506),
 .UNSPECIFIED.,.F.,.F.,(4,4),(1.07417908634448,2.12367450625336),
 .UNSPECIFIED.);
#1189=B_SPLINE_CURVE_WITH_KNOTS('',3,(#47511,#47512,#47513,#47514),
 .UNSPECIFIED.,.F.,.F.,(4,4),(1.02070861103776,2.07039533198825),
 .UNSPECIFIED.);
#1190=B_SPLINE_CURVE_WITH_KNOTS('',3,(#47517,#47518,#47519,#47520),
 .UNSPECIFIED.,.F.,.F.,(4,4),(1.06098917218957,2.11067589314006),
 .UNSPECIFIED.);
#1191=B_SPLINE_CURVE_WITH_KNOTS('',3,(#47525,#47526,#47527,#47528),
 .UNSPECIFIED.,.F.,.F.,(4,4),(1.02070861103776,2.07039533198825),
 .UNSPECIFIED.);
#1192=B_SPLINE_CURVE_WITH_KNOTS('',3,(#47531,#47532,#47533,#47534),
 .UNSPECIFIED.,.F.,.F.,(4,4),(1.06098917218957,2.11067589314006),
 .UNSPECIFIED.);
#1193=B_SPLINE_CURVE_WITH_KNOTS('',3,(#47539,#47540,#47541,#47542),
 .UNSPECIFIED.,.F.,.F.,(4,4),(1.08743350871974,2.13692892862862),
 .UNSPECIFIED.);
#1194=B_SPLINE_CURVE_WITH_KNOTS('',3,(#47545,#47546,#47547,#47548),
 .UNSPECIFIED.,.F.,.F.,(4,4),(1.07417908634448,2.12367450625336),
 .UNSPECIFIED.);
#1195=B_SPLINE_CURVE_WITH_KNOTS('',3,(#47553,#47554,#47555,#47556),
 .UNSPECIFIED.,.F.,.F.,(4,4),(1.09726472627116,2.14673867240921),
 .UNSPECIFIED.);
#1196=B_SPLINE_CURVE_WITH_KNOTS('',3,(#47559,#47560,#47561,#47562),
 .UNSPECIFIED.,.F.,.F.,(4,4),(1.07572637127808,2.12520031741614),
 .UNSPECIFIED.);
#1197=B_SPLINE_CURVE_WITH_KNOTS('',3,(#47567,#47568,#47569,#47570),
 .UNSPECIFIED.,.F.,.F.,(4,4),(1.03463183846599,2.08427034714714),
 .UNSPECIFIED.);
#1198=B_SPLINE_CURVE_WITH_KNOTS('',3,(#47573,#47574,#47575,#47576),
 .UNSPECIFIED.,.F.,.F.,(4,4),(1.06519471367074,2.1148332223519),
 .UNSPECIFIED.);
#1199=B_SPLINE_CURVE_WITH_KNOTS('',3,(#47581,#47582,#47583,#47584),
 .UNSPECIFIED.,.F.,.F.,(4,4),(1.00966173528769,2.0593901610072),
 .UNSPECIFIED.);
#1200=B_SPLINE_CURVE_WITH_KNOTS('',3,(#47587,#47588,#47589,#47590),
 .UNSPECIFIED.,.F.,.F.,(4,4),(1.05659594524126,2.10632437096077),
 .UNSPECIFIED.);
#1201=B_SPLINE_CURVE_WITH_KNOTS('',3,(#47595,#47596,#47597,#47598),
 .UNSPECIFIED.,.F.,.F.,(4,4),(1.06876863774445,2.11830775146031),
 .UNSPECIFIED.);
#1202=B_SPLINE_CURVE_WITH_KNOTS('',3,(#47601,#47602,#47603,#47604),
 .UNSPECIFIED.,.F.,.F.,(4,4),(1.07183362023116,2.12137273394701),
 .UNSPECIFIED.);
#1203=B_SPLINE_CURVE_WITH_KNOTS('',3,(#47609,#47610,#47611,#47612),
 .UNSPECIFIED.,.F.,.F.,(4,4),(1.09809076783139,2.14756146587266),
 .UNSPECIFIED.);
#1204=B_SPLINE_CURVE_WITH_KNOTS('',3,(#47615,#47616,#47617,#47618),
 .UNSPECIFIED.,.F.,.F.,(4,4),(1.07645732586072,2.12592802390199),
 .UNSPECIFIED.);
#1205=B_SPLINE_CURVE_WITH_KNOTS('',3,(#47623,#47624,#47625,#47626),
 .UNSPECIFIED.,.F.,.F.,(4,4),(1.05088688291748,2.10047487643504),
 .UNSPECIFIED.);
#1206=B_SPLINE_CURVE_WITH_KNOTS('',3,(#47629,#47630,#47631,#47632),
 .UNSPECIFIED.,.F.,.F.,(4,4),(1.06882494380372,2.11841293732128),
 .UNSPECIFIED.);
#1207=B_SPLINE_CURVE_WITH_KNOTS('',3,(#47635,#47636,#47637,#47638),
 .UNSPECIFIED.,.F.,.F.,(4,4),(1.00183351673943,2.05159618842433),
 .UNSPECIFIED.);
#1208=B_SPLINE_CURVE_WITH_KNOTS('',3,(#47642,#47643,#47644,#47645),
 .UNSPECIFIED.,.F.,.F.,(4,4),(1.05075063815515,2.10051330984005),
 .UNSPECIFIED.);
#1209=B_SPLINE_CURVE_WITH_KNOTS('',3,(#47657,#47658,#47659,#47660),
 .UNSPECIFIED.,.F.,.F.,(4,4),(1.0651631905772,2.1146873922484),
 .UNSPECIFIED.);
#1210=B_SPLINE_CURVE_WITH_KNOTS('',3,(#47663,#47664,#47665,#47666),
 .UNSPECIFIED.,.F.,.F.,(4,4),(1.08410770108472,2.13363190275592),
 .UNSPECIFIED.);
#1211=B_SPLINE_CURVE_WITH_KNOTS('',3,(#47671,#47672,#47673,#47674),
 .UNSPECIFIED.,.F.,.F.,(4,4),(1.09826811480986,2.14770347966715),
 .UNSPECIFIED.);
#1212=B_SPLINE_CURVE_WITH_KNOTS('',3,(#47677,#47678,#47679,#47680),
 .UNSPECIFIED.,.F.,.F.,(4,4),(1.0915792594565,2.14101462431379),
 .UNSPECIFIED.);
#1213=B_SPLINE_CURVE_WITH_KNOTS('',3,(#47685,#47686,#47687,#47688),
 .UNSPECIFIED.,.F.,.F.,(4,4),(1.08247899997509,2.13195661716112),
 .UNSPECIFIED.);
#1214=B_SPLINE_CURVE_WITH_KNOTS('',3,(#47691,#47692,#47693,#47694),
 .UNSPECIFIED.,.F.,.F.,(4,4),(1.08711062908542,2.13658824627145),
 .UNSPECIFIED.);
#1215=B_SPLINE_CURVE_WITH_KNOTS('',3,(#47699,#47700,#47701,#47702),
 .UNSPECIFIED.,.F.,.F.,(4,4),(1.02489973343678,2.07455809562116),
 .UNSPECIFIED.);
#1216=B_SPLINE_CURVE_WITH_KNOTS('',3,(#47705,#47706,#47707,#47708),
 .UNSPECIFIED.,.F.,.F.,(4,4),(1.07188875891378,2.12154712109815),
 .UNSPECIFIED.);
#1217=B_SPLINE_CURVE_WITH_KNOTS('',3,(#47713,#47714,#47715,#47716),
 .UNSPECIFIED.,.F.,.F.,(4,4),(1.04935390711823,2.09892626486964),
 .UNSPECIFIED.);
#1218=B_SPLINE_CURVE_WITH_KNOTS('',3,(#47719,#47720,#47721,#47722),
 .UNSPECIFIED.,.F.,.F.,(4,4),(1.08048205057026,2.13005440832166),
 .UNSPECIFIED.);
#1219=B_SPLINE_CURVE_WITH_KNOTS('',3,(#47727,#47728,#47729,#47730),
 .UNSPECIFIED.,.F.,.F.,(4,4),(1.09744201858002,2.14688060738206),
 .UNSPECIFIED.);
#1220=B_SPLINE_CURVE_WITH_KNOTS('',3,(#47733,#47734,#47735,#47736),
 .UNSPECIFIED.,.F.,.F.,(4,4),(1.0908483826499,2.14028697145194),
 .UNSPECIFIED.);
#1221=B_SPLINE_CURVE_WITH_KNOTS('',3,(#47741,#47742,#47743,#47744),
 .UNSPECIFIED.,.F.,.F.,(4,4),(1.09579976662743,2.14524477934728),
 .UNSPECIFIED.);
#1222=B_SPLINE_CURVE_WITH_KNOTS('',3,(#47747,#47748,#47749,#47750),
 .UNSPECIFIED.,.F.,.F.,(4,4),(1.08939524602275,2.1388402587426),
 .UNSPECIFIED.);
#1223=B_SPLINE_CURVE_WITH_KNOTS('',3,(#47755,#47756,#47757,#47758),
 .UNSPECIFIED.,.F.,.F.,(4,4),(1.03575222205974,2.08537061780256),
 .UNSPECIFIED.);
#1224=B_SPLINE_CURVE_WITH_KNOTS('',3,(#47761,#47762,#47763,#47764),
 .UNSPECIFIED.,.F.,.F.,(4,4),(1.07627988374361,2.12589827948644),
 .UNSPECIFIED.);
#1225=B_SPLINE_CURVE_WITH_KNOTS('',3,(#47769,#47770,#47771,#47772),
 .UNSPECIFIED.,.F.,.F.,(4,4),(1.03575222205973,2.08537061780256),
 .UNSPECIFIED.);
#1226=B_SPLINE_CURVE_WITH_KNOTS('',3,(#47775,#47776,#47777,#47778),
 .UNSPECIFIED.,.F.,.F.,(4,4),(1.07627988374361,2.12589827948644),
 .UNSPECIFIED.);
#1227=B_SPLINE_CURVE_WITH_KNOTS('',3,(#47783,#47784,#47785,#47786),
 .UNSPECIFIED.,.F.,.F.,(4,4),(1.09579976662742,2.14524477934727),
 .UNSPECIFIED.);
#1228=B_SPLINE_CURVE_WITH_KNOTS('',3,(#47789,#47790,#47791,#47792),
 .UNSPECIFIED.,.F.,.F.,(4,4),(1.08939524602275,2.1388402587426),
 .UNSPECIFIED.);
#1229=B_SPLINE_CURVE_WITH_KNOTS('',3,(#47797,#47798,#47799,#47800),
 .UNSPECIFIED.,.F.,.F.,(4,4),(1.09744201858002,2.14688060738207),
 .UNSPECIFIED.);
#1230=B_SPLINE_CURVE_WITH_KNOTS('',3,(#47803,#47804,#47805,#47806),
 .UNSPECIFIED.,.F.,.F.,(4,4),(1.0908483826499,2.14028697145194),
 .UNSPECIFIED.);
#1231=B_SPLINE_CURVE_WITH_KNOTS('',3,(#47811,#47812,#47813,#47814),
 .UNSPECIFIED.,.F.,.F.,(4,4),(1.04935390711825,2.09892626486965),
 .UNSPECIFIED.);
#1232=B_SPLINE_CURVE_WITH_KNOTS('',3,(#47817,#47818,#47819,#47820),
 .UNSPECIFIED.,.F.,.F.,(4,4),(1.08048205057026,2.13005440832167),
 .UNSPECIFIED.);
#1233=B_SPLINE_CURVE_WITH_KNOTS('',3,(#47825,#47826,#47827,#47828),
 .UNSPECIFIED.,.F.,.F.,(4,4),(1.02489973343678,2.07455809562116),
 .UNSPECIFIED.);
#1234=B_SPLINE_CURVE_WITH_KNOTS('',3,(#47831,#47832,#47833,#47834),
 .UNSPECIFIED.,.F.,.F.,(4,4),(1.07188875891378,2.12154712109815),
 .UNSPECIFIED.);
#1235=B_SPLINE_CURVE_WITH_KNOTS('',3,(#47839,#47840,#47841,#47842),
 .UNSPECIFIED.,.F.,.F.,(4,4),(1.0824789999751,2.13195661716112),
 .UNSPECIFIED.);
#1236=B_SPLINE_CURVE_WITH_KNOTS('',3,(#47845,#47846,#47847,#47848),
 .UNSPECIFIED.,.F.,.F.,(4,4),(1.08711062908542,2.13658824627145),
 .UNSPECIFIED.);
#1237=B_SPLINE_CURVE_WITH_KNOTS('',3,(#47853,#47854,#47855,#47856),
 .UNSPECIFIED.,.F.,.F.,(4,4),(1.09826811479926,2.14770347965657),
 .UNSPECIFIED.);
#1238=B_SPLINE_CURVE_WITH_KNOTS('',3,(#47859,#47860,#47861,#47862),
 .UNSPECIFIED.,.F.,.F.,(4,4),(1.09157925945638,2.14101462431369),
 .UNSPECIFIED.);
#1239=B_SPLINE_CURVE_WITH_KNOTS('',3,(#47867,#47868,#47869,#47870),
 .UNSPECIFIED.,.F.,.F.,(4,4),(1.06516319055868,2.11468739222992),
 .UNSPECIFIED.);
#1240=B_SPLINE_CURVE_WITH_KNOTS('',3,(#47873,#47874,#47875,#47876),
 .UNSPECIFIED.,.F.,.F.,(4,4),(1.08410770108451,2.13363190275575),
 .UNSPECIFIED.);
#1241=B_SPLINE_CURVE_WITH_KNOTS('',3,(#47879,#47880,#47881,#47882),
 .UNSPECIFIED.,.F.,.F.,(4,4),(1.06604442753704,2.11573584316717),
 .UNSPECIFIED.);
#1242=B_SPLINE_CURVE_WITH_KNOTS('',3,(#47886,#47887,#47888,#47889),
 .UNSPECIFIED.,.F.,.F.,(4,4),(1.01713682798446,2.0668282436146),
 .UNSPECIFIED.);
#1243=B_SPLINE_CURVE_WITH_KNOTS('',3,(#47910,#47911,#47912,#47913),
 .UNSPECIFIED.,.F.,.F.,(4,4),(0.988228581953082,2.02619732383854),
 .UNSPECIFIED.);
#1244=B_SPLINE_CURVE_WITH_KNOTS('',3,(#47930,#47931,#47932,#47933),
 .UNSPECIFIED.,.F.,.F.,(4,4),(0.996245219772127,2.03408046027085),
 .UNSPECIFIED.);
#1245=B_SPLINE_CURVE_WITH_KNOTS('',3,(#47950,#47951,#47952,#47953),
 .UNSPECIFIED.,.F.,.F.,(4,4),(0.991257065987786,2.02917865590825),
 .UNSPECIFIED.);
#1246=B_SPLINE_CURVE_WITH_KNOTS('',3,(#47970,#47971,#47972,#47973),
 .UNSPECIFIED.,.F.,.F.,(4,4),(0.975946465952181,2.01405910333835),
 .UNSPECIFIED.);
#1247=B_SPLINE_CURVE_WITH_KNOTS('',3,(#47990,#47991,#47992,#47993),
 .UNSPECIFIED.,.F.,.F.,(4,4),(0.984583139670925,2.02260243625185),
 .UNSPECIFIED.);
#1248=B_SPLINE_CURVE_WITH_KNOTS('',3,(#48010,#48011,#48012,#48013),
 .UNSPECIFIED.,.F.,.F.,(4,4),(0.995299247716725,2.03315199866672),
 .UNSPECIFIED.);
#1249=B_SPLINE_CURVE_WITH_KNOTS('',3,(#48030,#48031,#48032,#48033),
 .UNSPECIFIED.,.F.,.F.,(4,4),(0.99362573826485,2.03150775762006),
 .UNSPECIFIED.);
#1250=B_SPLINE_CURVE_WITH_KNOTS('',3,(#48050,#48051,#48052,#48053),
 .UNSPECIFIED.,.F.,.F.,(4,4),(0.980365846111703,2.01843481385154),
 .UNSPECIFIED.);
#1251=B_SPLINE_CURVE_WITH_KNOTS('',3,(#48070,#48071,#48072,#48073),
 .UNSPECIFIED.,.F.,.F.,(4,4),(0.980365846111703,2.01843481385154),
 .UNSPECIFIED.);
#1252=B_SPLINE_CURVE_WITH_KNOTS('',3,(#48090,#48091,#48092,#48093),
 .UNSPECIFIED.,.F.,.F.,(4,4),(0.993625738264851,2.03150775762006),
 .UNSPECIFIED.);
#1253=B_SPLINE_CURVE_WITH_KNOTS('',3,(#48110,#48111,#48112,#48113),
 .UNSPECIFIED.,.F.,.F.,(4,4),(0.995299247716725,2.03315199866672),
 .UNSPECIFIED.);
#1254=B_SPLINE_CURVE_WITH_KNOTS('',3,(#48130,#48131,#48132,#48133),
 .UNSPECIFIED.,.F.,.F.,(4,4),(0.984583139670924,2.02260243625185),
 .UNSPECIFIED.);
#1255=B_SPLINE_CURVE_WITH_KNOTS('',3,(#48150,#48151,#48152,#48153),
 .UNSPECIFIED.,.F.,.F.,(4,4),(0.975946465952182,2.01405910333835),
 .UNSPECIFIED.);
#1256=B_SPLINE_CURVE_WITH_KNOTS('',3,(#48170,#48171,#48172,#48173),
 .UNSPECIFIED.,.F.,.F.,(4,4),(0.991257065987786,2.02917865590825),
 .UNSPECIFIED.);
#1257=B_SPLINE_CURVE_WITH_KNOTS('',3,(#48190,#48191,#48192,#48193),
 .UNSPECIFIED.,.F.,.F.,(4,4),(0.99624520912574,2.03408045013743),
 .UNSPECIFIED.);
#1258=B_SPLINE_CURVE_WITH_KNOTS('',3,(#48210,#48211,#48212,#48213),
 .UNSPECIFIED.,.F.,.F.,(4,4),(0.988228562594649,2.02619730816861),
 .UNSPECIFIED.);
#1259=B_SPLINE_CURVE_WITH_KNOTS('',3,(#48231,#48232,#48233,#48234),
 .UNSPECIFIED.,.F.,.F.,(4,4),(0.97041538436032,2.0085649015089),
 .UNSPECIFIED.);
#1260=B_SPLINE_CURVE_WITH_KNOTS('',3,(#48241,#48242,#48243,#48244),
 .UNSPECIFIED.,.F.,.F.,(4,4),(1.00572796764383,2.04369670952928),
 .UNSPECIFIED.);
#1261=B_SPLINE_CURVE_WITH_KNOTS('',3,(#48253,#48254,#48255,#48256),
 .UNSPECIFIED.,.F.,.F.,(4,4),(0.972542826498871,2.01061179423871),
 .UNSPECIFIED.);
#1262=B_SPLINE_CURVE_WITH_KNOTS('',3,(#48259,#48260,#48261,#48262),
 .UNSPECIFIED.,.F.,.F.,(4,4),(1.04725787168466,2.08513989103987),
 .UNSPECIFIED.);
#1263=B_SPLINE_CURVE_WITH_KNOTS('',3,(#48265,#48266,#48267,#48268),
 .UNSPECIFIED.,.F.,.F.,(4,4),(1.06889245483208,2.10674520578207),
 .UNSPECIFIED.);
#1264=B_SPLINE_CURVE_WITH_KNOTS('',3,(#48271,#48272,#48273,#48274),
 .UNSPECIFIED.,.F.,.F.,(4,4),(0.987740311273852,2.02575960785478),
 .UNSPECIFIED.);
#1265=B_SPLINE_CURVE_WITH_KNOTS('',3,(#48277,#48278,#48279,#48280),
 .UNSPECIFIED.,.F.,.F.,(4,4),(0.960726337881709,1.99883897526788),
 .UNSPECIFIED.);
#1266=B_SPLINE_CURVE_WITH_KNOTS('',3,(#48283,#48284,#48285,#48286),
 .UNSPECIFIED.,.F.,.F.,(4,4),(1.02588990754098,2.06381149746145),
 .UNSPECIFIED.);
#1267=B_SPLINE_CURVE_WITH_KNOTS('',3,(#48289,#48290,#48291,#48292),
 .UNSPECIFIED.,.F.,.F.,(4,4),(1.0893949973477,2.12723023784643),
 .UNSPECIFIED.);
#1268=B_SPLINE_CURVE_WITH_KNOTS('',3,(#48296,#48297,#48298,#48299),
 .UNSPECIFIED.,.F.,.F.,(4,4),(0.952533772491406,1.99068328963999),
 .UNSPECIFIED.);
#1269=B_SPLINE_CURVE_WITH_KNOTS('',3,(#48302,#48303,#48304,#48305),
 .UNSPECIFIED.,.F.,.F.,(4,4),(1.00572623032852,2.04369497590248),
 .UNSPECIFIED.);
#1270=B_SPLINE_CURVE_WITH_KNOTS('',3,(#48308,#48309,#48310,#48311),
 .UNSPECIFIED.,.F.,.F.,(4,4),(1.08939401792972,2.12722925894141),
 .UNSPECIFIED.);
#1271=B_SPLINE_CURVE_WITH_KNOTS('',3,(#48314,#48315,#48316,#48317),
 .UNSPECIFIED.,.F.,.F.,(4,4),(1.02588990754098,2.06381149746145),
 .UNSPECIFIED.);
#1272=B_SPLINE_CURVE_WITH_KNOTS('',3,(#48320,#48321,#48322,#48323),
 .UNSPECIFIED.,.F.,.F.,(4,4),(0.960726337881709,1.99883897526788),
 .UNSPECIFIED.);
#1273=B_SPLINE_CURVE_WITH_KNOTS('',3,(#48326,#48327,#48328,#48329),
 .UNSPECIFIED.,.F.,.F.,(4,4),(0.987740311273852,2.02575960785478),
 .UNSPECIFIED.);
#1274=B_SPLINE_CURVE_WITH_KNOTS('',3,(#48332,#48333,#48334,#48335),
 .UNSPECIFIED.,.F.,.F.,(4,4),(1.06889245483208,2.10674520578207),
 .UNSPECIFIED.);
#1275=B_SPLINE_CURVE_WITH_KNOTS('',3,(#48338,#48339,#48340,#48341),
 .UNSPECIFIED.,.F.,.F.,(4,4),(1.04725787168466,2.08513989103987),
 .UNSPECIFIED.);
#1276=B_SPLINE_CURVE_WITH_KNOTS('',3,(#48344,#48345,#48346,#48347),
 .UNSPECIFIED.,.F.,.F.,(4,4),(0.972542826498871,2.01061179423871),
 .UNSPECIFIED.);
#1277=B_SPLINE_CURVE_WITH_KNOTS('',3,(#48579,#48580,#48581,#48582,#48583,
#48584,#48585,#48586,#48587,#48588,#48589,#48590,#48591),.UNSPECIFIED.,
 .F.,.F.,(4,3,3,3,4),(-5.01260736916534,-4.99316617057127,-3.99453293645702,
-2.99589970234276,-2.06120159751579),.UNSPECIFIED.);
#1278=B_SPLINE_CURVE_WITH_KNOTS('',3,(#48599,#48600,#48601,#48602,#48603,
#48604,#48605,#48606,#48607,#48608),.UNSPECIFIED.,.F.,.F.,(4,3,3,4),(0.,
0.998633234114252,1.99726646822851,2.02990353988235),.UNSPECIFIED.);
#1279=B_SPLINE_CURVE_WITH_KNOTS('',3,(#48613,#48614,#48615,#48616,#48617,
#48618,#48619,#48620,#48621,#48622,#48623,#48624,#48625,#48626,#48627,#48628,
#48629,#48630,#48631,#48632,#48633,#48634),.UNSPECIFIED.,.F.,.F.,(4,3,3,
3,3,3,3,4),(-11.2957926763449,-10.9849655752568,-9.98633234114256,-8.9876991070283,
-7.98906587291404,-6.99043263879979,-5.99179940468553,-5.01260736916534),
 .UNSPECIFIED.);
#1280=B_SPLINE_CURVE_WITH_KNOTS('',3,(#48635,#48636,#48637,#48638,#48639,
#48640,#48641,#48642,#48643,#48644,#48645,#48646,#48647,#48648,#48649,#48650,
#48651,#48652,#48653,#48654,#48655,#48656),.UNSPECIFIED.,.F.,.F.,(4,3,3,
3,3,3,3,4),(2.02990353988235,2.99589970234276,3.99453293645702,4.99316617057127,
5.99179940468553,6.99043263879979,7.98906587291404,8.31308884706194),
 .UNSPECIFIED.);
#1281=B_SPLINE_CURVE_WITH_KNOTS('',3,(#48661,#48662,#48663,#48664,#48665,
#48666,#48667,#48668,#48669,#48670,#48671,#48672,#48673,#48674,#48675,#48676,
#48677,#48678,#48679,#48680,#48681,#48682),.UNSPECIFIED.,.F.,.F.,(4,3,3,
3,3,3,3,4),(-17.5789779835245,-16.9767649799423,-15.9781317458281,-14.9794985117138,
-13.9808652775996,-12.9822320434853,-11.9835988093711,-11.2957926763449),
 .UNSPECIFIED.);
#1282=B_SPLINE_CURVE_WITH_KNOTS('',3,(#48683,#48684,#48685,#48686,#48687,
#48688,#48689,#48690,#48691,#48692,#48693,#48694,#48695,#48696,#48697,#48698,
#48699,#48700,#48701,#48702,#48703,#48704),.UNSPECIFIED.,.F.,.F.,(4,3,3,
3,3,3,3,4),(8.31308884706194,8.9876991070283,9.98633234114255,10.9849655752568,
11.9835988093711,12.9822320434853,13.9808652775996,14.5962741542415),
 .UNSPECIFIED.);
#1283=B_SPLINE_CURVE_WITH_KNOTS('',3,(#48709,#48710,#48711,#48712,#48713,
#48714,#48715,#48716,#48717,#48718,#48719,#48720,#48721,#48722,#48723,#48724,
#48725,#48726,#48727,#48728,#48729,#48730),.UNSPECIFIED.,.F.,.F.,(4,3,3,
3,3,3,3,4),(-23.8621632907041,-22.9685643846279,-21.9699311505136,-20.9712979163994,
-19.9726646822851,-18.9740314481709,-17.9753982140566,-17.5789779835245),
 .UNSPECIFIED.);
#1284=B_SPLINE_CURVE_WITH_KNOTS('',3,(#48731,#48732,#48733,#48734,#48735,
#48736,#48737,#48738,#48739,#48740,#48741,#48742,#48743,#48744,#48745,#48746,
#48747,#48748,#48749,#48750,#48751,#48752),.UNSPECIFIED.,.F.,.F.,(4,3,3,
3,3,3,3,4),(14.5962741542415,14.9794985117138,15.9781317458281,16.9767649799423,
17.9753982140566,18.9740314481709,19.9726646822851,20.8794594614211),
 .UNSPECIFIED.);
#1285=B_SPLINE_CURVE_WITH_KNOTS('',3,(#48757,#48758,#48759,#48760,#48761,
#48762,#48763,#48764,#48765,#48766,#48767,#48768,#48769,#48770,#48771,#48772,
#48773,#48774,#48775,#48776,#48777,#48778,#48779,#48780,#48781),
 .UNSPECIFIED.,.F.,.F.,(4,3,3,3,3,3,3,3,4),(-30.1453485978837,-29.9589970234277,
-28.9603637893134,-27.9617305551992,-26.9630973210849,-25.9644640869706,
-24.9658308528564,-23.9671976187421,-23.8621632907041),.UNSPECIFIED.);
#1286=B_SPLINE_CURVE_WITH_KNOTS('',3,(#48782,#48783,#48784,#48785,#48786,
#48787,#48788,#48789,#48790,#48791,#48792,#48793,#48794,#48795,#48796,#48797,
#48798,#48799,#48800,#48801,#48802,#48803,#48804,#48805,#48806),
 .UNSPECIFIED.,.F.,.F.,(4,3,3,3,3,3,3,3,4),(20.8794594614211,20.9712979163994,
21.9699311505136,22.9685643846279,23.9671976187421,24.9658308528564,25.9644640869706,
26.9630973210849,27.1626447686007),.UNSPECIFIED.);
#1287=B_SPLINE_CURVE_WITH_KNOTS('',3,(#48811,#48812,#48813,#48814,#48815,
#48816,#48817,#48818,#48819,#48820,#48821,#48822,#48823,#48824,#48825,#48826,
#48827,#48828,#48829,#48830,#48831,#48832),.UNSPECIFIED.,.F.,.F.,(4,3,3,
3,3,3,3,4),(-36.4285339050633,-35.9507964281132,-34.9521631939989,-33.9535299598847,
-32.9548967257704,-31.9562634916562,-30.9576302575419,-30.1453485978837),
 .UNSPECIFIED.);
#1288=B_SPLINE_CURVE_WITH_KNOTS('',3,(#48833,#48834,#48835,#48836,#48837,
#48838,#48839,#48840,#48841,#48842,#48843,#48844,#48845,#48846,#48847,#48848,
#48849,#48850,#48851,#48852,#48853,#48854),.UNSPECIFIED.,.F.,.F.,(4,3,3,
3,3,3,3,4),(27.1626447686007,27.9617305551991,28.9603637893134,29.9589970234277,
30.9576302575419,31.9562634916562,32.9548967257704,33.4458300757803),
 .UNSPECIFIED.);
#1289=B_SPLINE_CURVE_WITH_KNOTS('',3,(#48859,#48860,#48861,#48862,#48863,
#48864,#48865,#48866,#48867,#48868,#48869,#48870,#48871,#48872,#48873,#48874,
#48875,#48876,#48877,#48878,#48879,#48880),.UNSPECIFIED.,.F.,.F.,(4,3,3,
3,3,3,3,4),(-42.7117192122429,-41.9425958327987,-40.9439625986845,-39.9453293645702,
-38.946696130456,-37.9480628963417,-36.9494296622274,-36.4285339050633),
 .UNSPECIFIED.);
#1290=B_SPLINE_CURVE_WITH_KNOTS('',3,(#48881,#48882,#48883,#48884,#48885,
#48886,#48887,#48888,#48889,#48890,#48891,#48892,#48893,#48894,#48895,#48896,
#48897,#48898,#48899,#48900,#48901,#48902),.UNSPECIFIED.,.F.,.F.,(4,3,3,
3,3,3,3,4),(33.4458300757803,33.9535299598847,34.9521631939989,35.9507964281132,
36.9494296622274,37.9480628963417,38.946696130456,39.7290153829599),
 .UNSPECIFIED.);
#1291=B_SPLINE_CURVE_WITH_KNOTS('',3,(#48907,#48908,#48909,#48910,#48911,
#48912,#48913,#48914,#48915,#48916,#48917,#48918,#48919,#48920,#48921,#48922,
#48923,#48924,#48925,#48926,#48927,#48928,#48929,#48930,#48931),
 .UNSPECIFIED.,.F.,.F.,(4,3,3,3,3,3,3,3,4),(-48.9949045194225,-48.9330284715985,
-47.9343952374843,-46.93576200337,-45.9371287692558,-44.9384955351415,-43.9398623010272,
-42.941229066913,-42.7117192122429),.UNSPECIFIED.);
#1292=B_SPLINE_CURVE_WITH_KNOTS('',3,(#48932,#48933,#48934,#48935,#48936,
#48937,#48938,#48939,#48940,#48941,#48942,#48943,#48944,#48945,#48946,#48947,
#48948,#48949,#48950,#48951,#48952,#48953,#48954,#48955,#48956),
 .UNSPECIFIED.,.F.,.F.,(4,3,3,3,3,3,3,3,4),(39.7290153829599,39.9453293645702,
40.9439625986845,41.9425958327987,42.941229066913,43.9398623010272,44.9384955351415,
45.9371287692557,46.0122006901395),.UNSPECIFIED.);
#1293=B_SPLINE_CURVE_WITH_KNOTS('',3,(#48961,#48962,#48963,#48964,#48965,
#48966,#48967,#48968,#48969,#48970,#48971,#48972,#48973,#48974,#48975,#48976,
#48977,#48978,#48979,#48980,#48981,#48982),.UNSPECIFIED.,.F.,.F.,(4,3,3,
3,3,3,3,4),(-55.278089826602,-54.924827876284,-53.9261946421698,-52.9275614080555,
-51.9289281739413,-50.930294939827,-49.9316617057128,-48.9949045194225),
 .UNSPECIFIED.);
#1294=B_SPLINE_CURVE_WITH_KNOTS('',3,(#48983,#48984,#48985,#48986,#48987,
#48988,#48989,#48990,#48991,#48992,#48993,#48994,#48995,#48996,#48997,#48998,
#48999,#49000,#49001,#49002,#49003,#49004),.UNSPECIFIED.,.F.,.F.,(4,3,3,
3,3,3,3,4),(46.0122006901395,46.93576200337,47.9343952374843,48.9330284715985,
49.9316617057128,50.930294939827,51.9289281739413,52.2953859973191),
 .UNSPECIFIED.);
#1295=B_SPLINE_CURVE_WITH_KNOTS('',3,(#49009,#49010,#49011,#49012,#49013,
#49014,#49015,#49016,#49017,#49018,#49019,#49020,#49021,#49022,#49023,#49024,
#49025,#49026,#49027,#49028,#49029,#49030),.UNSPECIFIED.,.F.,.F.,(4,3,3,
3,3,3,3,4),(-61.5612751337816,-60.9166272809696,-59.9179940468553,-58.9193608127411,
-57.9207275786268,-56.9220943445126,-55.9234611103983,-55.278089826602),
 .UNSPECIFIED.);
#1296=B_SPLINE_CURVE_WITH_KNOTS('',3,(#49031,#49032,#49033,#49034,#49035,
#49036,#49037,#49038,#49039,#49040,#49041,#49042,#49043,#49044,#49045,#49046,
#49047,#49048,#49049,#49050,#49051,#49052),.UNSPECIFIED.,.F.,.F.,(4,3,3,
3,3,3,3,4),(52.2953859973191,52.9275614080555,53.9261946421698,54.9248278762841,
55.9234611103983,56.9220943445126,57.9207275786268,58.5785713044986),
 .UNSPECIFIED.);
#1297=B_SPLINE_CURVE_WITH_KNOTS('',3,(#49057,#49058,#49059,#49060,#49061,
#49062,#49063,#49064,#49065,#49066,#49067,#49068,#49069,#49070,#49071,#49072,
#49073,#49074,#49075,#49076,#49077,#49078),.UNSPECIFIED.,.F.,.F.,(4,3,3,
3,3,3,3,4),(-67.8444604409612,-66.9084266856551,-65.9097934515409,-64.9111602174266,
-63.9125269833123,-62.9138937491981,-61.9152605150838,-61.5612751337816),
 .UNSPECIFIED.);
#1298=B_SPLINE_CURVE_WITH_KNOTS('',3,(#49079,#49080,#49081,#49082,#49083,
#49084,#49085,#49086,#49087,#49088,#49089,#49090,#49091,#49092,#49093,#49094,
#49095,#49096,#49097,#49098,#49099,#49100),.UNSPECIFIED.,.F.,.F.,(4,3,3,
3,3,3,3,4),(58.5785713044986,58.9193608127411,59.9179940468553,60.9166272809696,
61.9152605150838,62.9138937491981,63.9125269833123,64.8617566116782),
 .UNSPECIFIED.);
#1299=B_SPLINE_CURVE_WITH_KNOTS('',3,(#49105,#49106,#49107,#49108,#49109,
#49110,#49111,#49112,#49113,#49114,#49115,#49116,#49117,#49118,#49119,#49120,
#49121,#49122,#49123,#49124,#49125,#49126,#49127,#49128,#49129),
 .UNSPECIFIED.,.F.,.F.,(4,3,3,3,3,3,3,3,4),(-74.1276457481408,-73.8988593244549,
-72.9002260903406,-71.9015928562264,-70.9029596221121,-69.9043263879979,
-68.9056931538836,-67.9070599197694,-67.8444604409612),.UNSPECIFIED.);
#1300=B_SPLINE_CURVE_WITH_KNOTS('',3,(#49130,#49131,#49132,#49133,#49134,
#49135,#49136,#49137,#49138,#49139,#49140,#49141,#49142,#49143,#49144,#49145,
#49146,#49147,#49148,#49149,#49150,#49151,#49152,#49153,#49154),
 .UNSPECIFIED.,.F.,.F.,(4,3,3,3,3,3,3,3,4),(64.8617566116782,64.9111602174266,
65.9097934515408,66.9084266856551,67.9070599197694,68.9056931538836,69.9043263879979,
70.9029596221121,71.1449419188578),.UNSPECIFIED.);
#1301=B_SPLINE_CURVE_WITH_KNOTS('',3,(#49159,#49160,#49161,#49162,#49163,
#49164,#49165,#49166,#49167,#49168,#49169,#49170,#49171,#49172,#49173,#49174,
#49175,#49176,#49177,#49178,#49179,#49180),.UNSPECIFIED.,.F.,.F.,(4,3,3,
3,3,3,3,4),(-80.4108310553204,-79.8906587291404,-78.8920254950262,-77.8933922609119,
-76.8947590267977,-75.8961257926834,-74.8974925585692,-74.1276457481408),
 .UNSPECIFIED.);
#1302=B_SPLINE_CURVE_WITH_KNOTS('',3,(#49181,#49182,#49183,#49184,#49185,
#49186,#49187,#49188,#49189,#49190,#49191,#49192,#49193,#49194,#49195,#49196,
#49197,#49198,#49199,#49200,#49201,#49202),.UNSPECIFIED.,.F.,.F.,(4,3,3,
3,3,3,3,4),(71.1449419188578,71.9015928562264,72.9002260903406,73.8988593244549,
74.8974925585692,75.8961257926834,76.8947590267977,77.4281272260374),
 .UNSPECIFIED.);
#1303=B_SPLINE_CURVE_WITH_KNOTS('',3,(#49207,#49208,#49209,#49210,#49211,
#49212,#49213,#49214,#49215,#49216,#49217,#49218,#49219,#49220,#49221,#49222,
#49223,#49224,#49225,#49226,#49227,#49228),.UNSPECIFIED.,.F.,.F.,(4,3,3,
3,3,3,3,4),(-86.6940163625,-85.882458133826,-84.8838248997117,-83.8851916655974,
-82.8865584314832,-81.8879251973689,-80.8892919632547,-80.4108310553204),
 .UNSPECIFIED.);
#1304=B_SPLINE_CURVE_WITH_KNOTS('',3,(#49229,#49230,#49231,#49232,#49233,
#49234,#49235,#49236,#49237,#49238,#49239,#49240,#49241,#49242,#49243,#49244,
#49245,#49246,#49247,#49248,#49249,#49250),.UNSPECIFIED.,.F.,.F.,(4,3,3,
3,3,3,3,4),(77.4281272260374,77.8933922609119,78.8920254950262,79.8906587291404,
80.8892919632547,81.887925197369,82.8865584314832,83.711312533217),
 .UNSPECIFIED.);
#1305=B_SPLINE_CURVE_WITH_KNOTS('',3,(#49255,#49256,#49257,#49258,#49259,
#49260,#49261,#49262,#49263,#49264,#49265,#49266,#49267,#49268,#49269,#49270,
#49271,#49272,#49273,#49274,#49275,#49276,#49277,#49278,#49279),
 .UNSPECIFIED.,.F.,.F.,(4,3,3,3,3,3,3,3,4),(-92.9772016696796,-92.8728907726257,
-91.8742575385115,-90.8756243043972,-89.876991070283,-88.8783578361687,
-87.8797246020545,-86.8810913679402,-86.6940163625),.UNSPECIFIED.);
#1306=B_SPLINE_CURVE_WITH_KNOTS('',3,(#49280,#49281,#49282,#49283,#49284,
#49285,#49286,#49287,#49288,#49289,#49290,#49291,#49292,#49293,#49294,#49295,
#49296,#49297,#49298,#49299,#49300,#49301,#49302,#49303,#49304),
 .UNSPECIFIED.,.F.,.F.,(4,3,3,3,3,3,3,3,4),(83.711312533217,83.8851916655975,
84.8838248997117,85.882458133826,86.8810913679402,87.8797246020545,88.8783578361687,
89.876991070283,89.9944978403966),.UNSPECIFIED.);
#1307=B_SPLINE_CURVE_WITH_KNOTS('',3,(#49309,#49310,#49311,#49312,#49313,
#49314,#49315,#49316,#49317,#49318,#49319,#49320,#49321,#49322,#49323,#49324,
#49325,#49326,#49327,#49328,#49329,#49330),.UNSPECIFIED.,.F.,.F.,(4,3,3,
3,3,3,3,4),(-99.2603869768592,-98.8646901773113,-97.866056943197,-96.8674237090828,
-95.8687904749685,-94.8701572408543,-93.87152400674,-92.9772016696796),
 .UNSPECIFIED.);
#1308=B_SPLINE_CURVE_WITH_KNOTS('',3,(#49331,#49332,#49333,#49334,#49335,
#49336,#49337,#49338,#49339,#49340,#49341,#49342,#49343,#49344,#49345,#49346,
#49347,#49348,#49349,#49350,#49351,#49352),.UNSPECIFIED.,.F.,.F.,(4,3,3,
3,3,3,3,4),(89.9944978403966,90.8756243043972,91.8742575385115,92.8728907726258,
93.87152400674,94.8701572408542,95.8687904749685,96.2776831475762),
 .UNSPECIFIED.);
#1309=B_SPLINE_CURVE_WITH_KNOTS('',3,(#49357,#49358,#49359,#49360,#49361,
#49362,#49363,#49364,#49365,#49366,#49367,#49368,#49369,#49370,#49371,#49372,
#49373,#49374,#49375,#49376,#49377,#49378),.UNSPECIFIED.,.F.,.F.,(4,3,3,
3,3,3,3,4),(-105.543572284039,-104.856489581997,-103.857856347883,-102.859223113768,
-101.860589879654,-100.86195664554,-99.8633234114255,-99.2603869768592),
 .UNSPECIFIED.);
#1310=B_SPLINE_CURVE_WITH_KNOTS('',3,(#49379,#49380,#49381,#49382,#49383,
#49384,#49385,#49386,#49387,#49388,#49389,#49390,#49391,#49392,#49393,#49394,
#49395,#49396,#49397,#49398,#49399,#49400),.UNSPECIFIED.,.F.,.F.,(4,3,3,
3,3,3,3,4),(96.2776831475762,96.8674237090828,97.866056943197,98.8646901773113,
99.8633234114255,100.86195664554,101.860589879654,102.560868454756),
 .UNSPECIFIED.);
#1311=B_SPLINE_CURVE_WITH_KNOTS('',3,(#49405,#49406,#49407,#49408,#49409,
#49410,#49411,#49412,#49413,#49414,#49415,#49416,#49417,#49418,#49419,#49420,
#49421,#49422,#49423,#49424,#49425,#49426),.UNSPECIFIED.,.F.,.F.,(4,3,3,
3,3,3,3,4),(-111.826757591218,-110.848288986682,-109.849655752568,-108.851022518454,
-107.85238928434,-106.853756050225,-105.855122816111,-105.543572284039),
 .UNSPECIFIED.);
#1312=B_SPLINE_CURVE_WITH_KNOTS('',3,(#49427,#49428,#49429,#49430,#49431,
#49432,#49433,#49434,#49435,#49436,#49437,#49438,#49439,#49440,#49441,#49442,
#49443,#49444,#49445,#49446,#49447,#49448),.UNSPECIFIED.,.F.,.F.,(4,3,3,
3,3,3,3,4),(102.560868454756,102.859223113768,103.857856347883,104.856489581997,
105.855122816111,106.853756050225,107.85238928434,108.844053761935),
 .UNSPECIFIED.);
#1313=B_SPLINE_CURVE_WITH_KNOTS('',3,(#49453,#49454,#49455,#49456,#49457,
#49458,#49459,#49460,#49461,#49462,#49463,#49464,#49465,#49466,#49467,#49468,
#49469,#49470,#49471,#49472,#49473,#49474,#49475,#49476,#49477),
 .UNSPECIFIED.,.F.,.F.,(4,3,3,3,3,3,3,3,4),(-118.109942898398,-117.838721625482,
-116.840088391368,-115.841455157254,-114.842821923139,-113.844188689025,
-112.845555454911,-111.846922220797,-111.826757591218),.UNSPECIFIED.);
#1314=B_SPLINE_CURVE_WITH_KNOTS('',3,(#49478,#49479,#49480,#49481,#49482,
#49483,#49484,#49485,#49486,#49487,#49488,#49489,#49490,#49491,#49492,#49493,
#49494,#49495,#49496,#49497,#49498,#49499,#49500,#49501,#49502),
 .UNSPECIFIED.,.F.,.F.,(4,3,3,3,3,3,3,3,4),(108.844053761935,108.851022518454,
109.849655752568,110.848288986682,111.846922220797,112.845555454911,113.844188689025,
114.842821923139,115.127239069115),.UNSPECIFIED.);
#1315=B_SPLINE_CURVE_WITH_KNOTS('',3,(#49507,#49508,#49509,#49510,#49511,
#49512,#49513,#49514,#49515,#49516,#49517,#49518,#49519,#49520,#49521,#49522,
#49523,#49524,#49525,#49526,#49527,#49528),.UNSPECIFIED.,.F.,.F.,(4,3,3,
3,3,3,3,4),(-124.393128205578,-123.830521030168,-122.831887796053,-121.833254561939,
-120.834621327825,-119.835988093711,-118.837354859596,-118.109942898398),
 .UNSPECIFIED.);
#1316=B_SPLINE_CURVE_WITH_KNOTS('',3,(#49529,#49530,#49531,#49532,#49533,
#49534,#49535,#49536,#49537,#49538,#49539,#49540,#49541,#49542,#49543,#49544,
#49545,#49546,#49547,#49548,#49549,#49550),.UNSPECIFIED.,.F.,.F.,(4,3,3,
3,3,3,3,4),(115.127239069115,115.841455157254,116.840088391368,117.838721625482,
118.837354859596,119.835988093711,120.834621327825,121.410424376295),
 .UNSPECIFIED.);
#1317=B_SPLINE_CURVE_WITH_KNOTS('',3,(#49555,#49556,#49557,#49558,#49559,
#49560,#49561,#49562,#49563,#49564,#49565,#49566,#49567,#49568,#49569,#49570,
#49571,#49572,#49573,#49574,#49575,#49576),.UNSPECIFIED.,.F.,.F.,(4,3,3,
3,3,3,3,4),(-130.676313512757,-129.822320434853,-128.823687200739,-127.825053966625,
-126.82642073251,-125.827787498396,-124.829154264282,-124.393128205578),
 .UNSPECIFIED.);
#1318=B_SPLINE_CURVE_WITH_KNOTS('',3,(#49577,#49578,#49579,#49580,#49581,
#49582,#49583,#49584,#49585,#49586,#49587,#49588,#49589,#49590,#49591,#49592,
#49593,#49594,#49595,#49596,#49597,#49598),.UNSPECIFIED.,.F.,.F.,(4,3,3,
3,3,3,3,4),(121.410424376295,121.833254561939,122.831887796053,123.830521030168,
124.829154264282,125.827787498396,126.82642073251,127.693609683474),
 .UNSPECIFIED.);
#1319=B_SPLINE_CURVE_WITH_KNOTS('',3,(#49603,#49604,#49605,#49606,#49607,
#49608,#49609,#49610,#49611,#49612,#49613,#49614,#49615,#49616,#49617,#49618,
#49619,#49620,#49621,#49622,#49623,#49624,#49625,#49626,#49627),
 .UNSPECIFIED.,.F.,.F.,(4,3,3,3,3,3,3,3,4),(-136.959498819937,-136.812753073653,
-135.814119839539,-134.815486605424,-133.81685337131,-132.818220137196,
-131.819586903082,-130.820953668967,-130.676313512757),.UNSPECIFIED.);
#1320=B_SPLINE_CURVE_WITH_KNOTS('',3,(#49628,#49629,#49630,#49631,#49632,
#49633,#49634,#49635,#49636,#49637,#49638,#49639,#49640,#49641,#49642,#49643,
#49644,#49645,#49646,#49647,#49648,#49649,#49650,#49651,#49652),
 .UNSPECIFIED.,.F.,.F.,(4,3,3,3,3,3,3,3,4),(127.693609683474,127.825053966625,
128.823687200739,129.822320434853,130.820953668967,131.819586903082,132.818220137196,
133.81685337131,133.976794990654),.UNSPECIFIED.);
#1321=B_SPLINE_CURVE_WITH_KNOTS('',3,(#49659,#49660,#49661,#49662,#49663,
#49664,#49665,#49666,#49667,#49668,#49669,#49670,#49671,#49672,#49673,#49674,
#49675,#49676,#49677),.UNSPECIFIED.,.F.,.F.,(4,3,3,3,3,3,4),(-142.804552478339,
-141.805919244224,-140.80728601011,-139.808652775996,-138.810019541882,
-137.811386307767,-136.959498819937),.UNSPECIFIED.);
#1322=B_SPLINE_CURVE_WITH_KNOTS('',3,(#49678,#49679,#49680,#49681,#49682,
#49683,#49684,#49685,#49686,#49687,#49688,#49689,#49690,#49691,#49692,#49693,
#49694,#49695,#49696,#49697,#49698,#49699),.UNSPECIFIED.,.F.,.F.,(4,3,3,
3,3,3,3,4),(133.976794990654,134.815486605425,135.814119839539,136.812753073653,
137.811386307767,138.810019541882,139.808652775996,140.259980297833),
 .UNSPECIFIED.);
#1323=B_SPLINE_CURVE_WITH_KNOTS('',3,(#49705,#49706,#49707,#49708,#49709,
#49710,#49711),.UNSPECIFIED.,.F.,.F.,(4,1,1,1,4),(153.9380400259,154.78992751373,
155.788560747845,156.787193981959,157.721892086786),.UNSPECIFIED.);
#1324=B_SPLINE_CURVE_WITH_KNOTS('',3,(#49714,#49715,#49716,#49717,#49718,
#49719),.UNSPECIFIED.,.F.,.F.,(4,1,1,4),(153.9380400259,154.485345738177,
155.483978972291,156.482612206405),.UNSPECIFIED.);
#1325=B_SPLINE_CURVE_WITH_KNOTS('',3,(#49724,#49725,#49726,#49727,#49728,
#49729,#49730,#49731,#49732,#49733,#49734),.UNSPECIFIED.,.F.,.F.,(4,1,1,
1,1,1,1,1,4),(147.65485471872,147.799494874931,148.798128109045,149.796761343159,
150.795394577273,151.794027811388,152.792661045502,153.791294279616,153.9380400259),
 .UNSPECIFIED.);
#1326=B_SPLINE_CURVE_WITH_KNOTS('',3,(#49735,#49736,#49737,#49738,#49739,
#49740,#49741,#49742,#49743,#49744),.UNSPECIFIED.,.F.,.F.,(4,1,1,1,1,1,
1,4),(147.65485471872,148.493546333491,149.492179567605,150.490812801719,
151.489446035834,152.488079269948,153.486712504062,153.9380400259),
 .UNSPECIFIED.);
#1327=B_SPLINE_CURVE_WITH_KNOTS('',3,(#49749,#49750,#49751,#49752,#49753,
#49754,#49755,#49756,#49757,#49758),.UNSPECIFIED.,.F.,.F.,(4,1,1,1,1,1,
1,4),(141.371669411541,141.807695470245,142.806328704359,143.804961938474,
144.803595172588,145.802228406702,146.800861640816,147.65485471872),
 .UNSPECIFIED.);
#1328=B_SPLINE_CURVE_WITH_KNOTS('',3,(#49759,#49760,#49761,#49762,#49763,
#49764,#49765,#49766,#49767,#49768,#49769),.UNSPECIFIED.,.F.,.F.,(4,1,1,
1,1,1,1,1,4),(141.371669411541,141.503113694691,142.501746928805,143.50038016292,
144.499013397034,145.497646631148,146.496279865262,147.494913099377,147.65485471872),
 .UNSPECIFIED.);
#1329=B_SPLINE_CURVE_WITH_KNOTS('',3,(#49774,#49775,#49776,#49777,#49778,
#49779,#49780,#49781,#49782,#49783),.UNSPECIFIED.,.F.,.F.,(4,1,1,1,1,1,
1,4),(135.088484104361,135.81589606556,136.814529299674,137.813162533788,
138.811795767902,139.810429002017,140.809062236131,141.371669411541),
 .UNSPECIFIED.);
#1330=B_SPLINE_CURVE_WITH_KNOTS('',3,(#49784,#49785,#49786,#49787,#49788,
#49789,#49790,#49791,#49792,#49793),.UNSPECIFIED.,.F.,.F.,(4,1,1,1,1,1,
1,4),(135.088484104361,135.511314290006,136.50994752412,137.508580758234,
138.507213992348,139.505847226463,140.504480460577,141.371669411541),
 .UNSPECIFIED.);
#1331=B_SPLINE_CURVE_WITH_KNOTS('',3,(#49798,#49799,#49800,#49801,#49802,
#49803,#49804,#49805,#49806,#49807,#49808),.UNSPECIFIED.,.F.,.F.,(4,1,1,
1,1,1,1,1,4),(128.805298797182,128.82546342676,129.824096660874,130.822729894988,
131.821363129103,132.819996363217,133.818629597331,134.817262831445,135.088484104361),
 .UNSPECIFIED.);
#1332=B_SPLINE_CURVE_WITH_KNOTS('',3,(#49809,#49810,#49811,#49812,#49813,
#49814,#49815,#49816,#49817,#49818),.UNSPECIFIED.,.F.,.F.,(4,1,1,1,1,1,
1,4),(128.805298797182,129.51951488532,130.518148119434,131.516781353549,
132.515414587663,133.514047821777,134.512681055891,135.088484104361),
 .UNSPECIFIED.);
#1333=B_SPLINE_CURVE_WITH_KNOTS('',3,(#49823,#49824,#49825,#49826,#49827,
#49828,#49829,#49830,#49831,#49832),.UNSPECIFIED.,.F.,.F.,(4,1,1,1,1,1,
1,4),(122.522113490002,122.833664022074,123.832297256189,124.830930490303,
125.829563724417,126.828196958531,127.826830192646,128.805298797182),
 .UNSPECIFIED.);
#1334=B_SPLINE_CURVE_WITH_KNOTS('',3,(#49833,#49834,#49835,#49836,#49837,
#49838,#49839,#49840,#49841,#49842,#49843),.UNSPECIFIED.,.F.,.F.,(4,1,1,
1,1,1,1,1,4),(122.522113490002,122.52908224652,123.527715480635,124.526348714749,
125.524981948863,126.523615182977,127.522248417092,128.520881651206,128.805298797182),
 .UNSPECIFIED.);
#1335=B_SPLINE_CURVE_WITH_KNOTS('',3,(#49848,#49849,#49850,#49851,#49852,
#49853,#49854,#49855,#49856,#49857),.UNSPECIFIED.,.F.,.F.,(4,1,1,1,1,1,
1,4),(116.238928182822,116.841864617389,117.840497851503,118.839131085617,
119.837764319731,120.836397553846,121.83503078796,122.522113490002),
 .UNSPECIFIED.);
#1336=B_SPLINE_CURVE_WITH_KNOTS('',3,(#49858,#49859,#49860,#49861,#49862,
#49863,#49864,#49865,#49866,#49867),.UNSPECIFIED.,.F.,.F.,(4,1,1,1,1,1,
1,4),(116.238928182822,116.537282841835,117.535916075949,118.534549310063,
119.533182544178,120.531815778292,121.530449012406,122.522113490002),
 .UNSPECIFIED.);
#1337=B_SPLINE_CURVE_WITH_KNOTS('',3,(#49872,#49873,#49874,#49875,#49876,
#49877,#49878,#49879,#49880,#49881),.UNSPECIFIED.,.F.,.F.,(4,1,1,1,1,1,
1,4),(109.955742875643,110.850065212703,111.848698446817,112.847331680932,
113.845964915046,114.84459814916,115.843231383274,116.238928182822),
 .UNSPECIFIED.);
#1338=B_SPLINE_CURVE_WITH_KNOTS('',3,(#49882,#49883,#49884,#49885,#49886,
#49887,#49888,#49889,#49890,#49891),.UNSPECIFIED.,.F.,.F.,(4,1,1,1,1,1,
1,4),(109.955742875643,110.545483437149,111.544116671264,112.542749905378,
113.541383139492,114.540016373606,115.538649607721,116.238928182822),
 .UNSPECIFIED.);
#1339=B_SPLINE_CURVE_WITH_KNOTS('',3,(#49896,#49897,#49898,#49899,#49900,
#49901,#49902,#49903,#49904,#49905,#49906),.UNSPECIFIED.,.F.,.F.,(4,1,1,
1,1,1,1,1,4),(103.672557568463,103.859632573903,104.858265808018,105.856899042132,
106.855532276246,107.85416551036,108.852798744475,109.851431978589,109.955742875643),
 .UNSPECIFIED.);
#1340=B_SPLINE_CURVE_WITH_KNOTS('',3,(#49907,#49908,#49909,#49910,#49911,
#49912,#49913,#49914,#49915,#49916),.UNSPECIFIED.,.F.,.F.,(4,1,1,1,1,1,
1,4),(103.672557568463,104.553684032464,105.552317266578,106.550950500692,
107.549583734807,108.548216968921,109.546850203035,109.955742875643),
 .UNSPECIFIED.);
#1341=B_SPLINE_CURVE_WITH_KNOTS('',3,(#49921,#49922,#49923,#49924,#49925,
#49926,#49927,#49928,#49929,#49930),.UNSPECIFIED.,.F.,.F.,(4,1,1,1,1,1,
1,4),(97.3893722612837,97.8678331692179,98.8664664033321,99.8650996374464,
100.863732871561,101.862366105675,102.860999339789,103.672557568463),
 .UNSPECIFIED.);
#1342=B_SPLINE_CURVE_WITH_KNOTS('',3,(#49931,#49932,#49933,#49934,#49935,
#49936,#49937,#49938,#49939,#49940,#49941),.UNSPECIFIED.,.F.,.F.,(4,1,1,
1,1,1,1,1,4),(97.3893722612836,97.563251393664,98.5618846277782,99.5605178618925,
100.559151096007,101.557784330121,102.556417564235,103.555050798349,103.672557568463),
 .UNSPECIFIED.);
#1343=B_SPLINE_CURVE_WITH_KNOTS('',3,(#49946,#49947,#49948,#49949,#49950,
#49951,#49952,#49953,#49954,#49955),.UNSPECIFIED.,.F.,.F.,(4,1,1,1,1,1,
1,4),(91.1061869541041,91.8760337645324,92.8746669986466,93.8733002327609,
94.8719334668751,95.8705667009894,96.8691999351036,97.3893722612837),
 .UNSPECIFIED.);
#1344=B_SPLINE_CURVE_WITH_KNOTS('',3,(#49956,#49957,#49958,#49959,#49960,
#49961,#49962,#49963,#49964,#49965),.UNSPECIFIED.,.F.,.F.,(4,1,1,1,1,1,
1,4),(91.106186954104,91.5714519889784,92.5700852230927,93.568718457207,
94.5673516913212,95.5659849254355,96.5646181595497,97.3893722612836),
 .UNSPECIFIED.);
#1345=B_SPLINE_CURVE_WITH_KNOTS('',3,(#49970,#49971,#49972,#49973,#49974,
#49975,#49976,#49977,#49978,#49979,#49980),.UNSPECIFIED.,.F.,.F.,(4,1,1,
1,1,1,1,1,4),(84.8230016469245,84.8856011257326,85.8842343598468,86.8828675939611,
87.8815008280753,88.8801340621896,89.8787672963038,90.8774005304181,91.1061869541041),
 .UNSPECIFIED.);
#1346=B_SPLINE_CURVE_WITH_KNOTS('',3,(#49981,#49982,#49983,#49984,#49985,
#49986,#49987,#49988,#49989,#49990),.UNSPECIFIED.,.F.,.F.,(4,1,1,1,1,1,
1,4),(84.8230016469244,85.5796525842929,86.5782858184072,87.5769190525214,
88.5755522866357,89.5741855207499,90.5728187548642,91.106186954104),
 .UNSPECIFIED.);
#1347=B_SPLINE_CURVE_WITH_KNOTS('',3,(#49995,#49996,#49997,#49998,#49999,
#50000,#50001,#50002,#50003,#50004),.UNSPECIFIED.,.F.,.F.,(4,1,1,1,1,1,
1,4),(78.5398163397449,78.893801721047,79.8924349551613,80.8910681892755,
81.8897014233898,82.888334657504,83.8869678916183,84.8230016469245),
 .UNSPECIFIED.);
#1348=B_SPLINE_CURVE_WITH_KNOTS('',3,(#50005,#50006,#50007,#50008,#50009,
#50010,#50011,#50012,#50013,#50014,#50015),.UNSPECIFIED.,.F.,.F.,(4,1,1,
1,1,1,1,1,4),(78.5398163397448,78.5892199454931,79.5878531796074,80.5864864137216,
81.5851196478359,82.5837528819501,83.5823861160644,84.5810193501787,84.8230016469244),
 .UNSPECIFIED.);
#1349=B_SPLINE_CURVE_WITH_KNOTS('',3,(#50020,#50021,#50022,#50023,#50024,
#50025,#50026,#50027,#50028,#50029),.UNSPECIFIED.,.F.,.F.,(4,1,1,1,1,1,
1,4),(72.2566310325653,72.9020023163615,73.9006355504758,74.89926878459,
75.8979020187043,76.8965352528185,77.8951684869328,78.5398163397449),
 .UNSPECIFIED.);
#1350=B_SPLINE_CURVE_WITH_KNOTS('',3,(#50030,#50031,#50032,#50033,#50034,
#50035,#50036,#50037,#50038,#50039),.UNSPECIFIED.,.F.,.F.,(4,1,1,1,1,1,
1,4),(72.2566310325653,72.5974205408076,73.5960537749218,74.5946870090361,
75.5933202431503,76.5919534772646,77.5905867113789,78.5398163397448),
 .UNSPECIFIED.);
#1351=B_SPLINE_CURVE_WITH_KNOTS('',3,(#50044,#50045,#50046,#50047,#50048,
#50049,#50050,#50051,#50052,#50053),.UNSPECIFIED.,.F.,.F.,(4,1,1,1,1,1,
1,4),(65.9734457253857,66.910202911676,67.9088361457902,68.9074693799045,
69.9061026140187,70.904735848133,71.9033690822472,72.2566310325653),
 .UNSPECIFIED.);
#1352=B_SPLINE_CURVE_WITH_KNOTS('',3,(#50054,#50055,#50056,#50057,#50058,
#50059,#50060,#50061,#50062,#50063),.UNSPECIFIED.,.F.,.F.,(4,1,1,1,1,1,
1,4),(65.9734457253856,66.6056211361221,67.6042543702363,68.6028876043506,
69.6015208384648,70.6001540725791,71.5987873066933,72.2566310325653),
 .UNSPECIFIED.);
#1353=B_SPLINE_CURVE_WITH_KNOTS('',3,(#50068,#50069,#50070,#50071,#50072,
#50073,#50074,#50075,#50076,#50077,#50078),.UNSPECIFIED.,.F.,.F.,(4,1,1,
1,1,1,1,1,4),(59.6902604182061,59.9197702728762,60.9184035069904,61.9170367411047,
62.9156699752189,63.9143032093332,64.9129364434474,65.9115696775617,65.9734457253857),
 .UNSPECIFIED.);
#1354=B_SPLINE_CURVE_WITH_KNOTS('',3,(#50079,#50080,#50081,#50082,#50083,
#50084,#50085,#50086,#50087,#50088),.UNSPECIFIED.,.F.,.F.,(4,1,1,1,1,1,
1,4),(59.6902604182061,60.6138217314365,61.6124549655508,62.611088199665,
63.6097214337793,64.6083546678935,65.6069879020078,65.9734457253856),
 .UNSPECIFIED.);
#1355=B_SPLINE_CURVE_WITH_KNOTS('',3,(#50093,#50094,#50095,#50096,#50097,
#50098,#50099,#50100,#50101,#50102),.UNSPECIFIED.,.F.,.F.,(4,1,1,1,1,1,
1,4),(53.4070751110265,53.9279708681906,54.9266041023049,55.9252373364192,
56.9238705705334,57.9225038046477,58.9211370387619,59.6902604182061),
 .UNSPECIFIED.);
#1356=B_SPLINE_CURVE_WITH_KNOTS('',3,(#50103,#50104,#50105,#50106,#50107,
#50108,#50109,#50110,#50111,#50112,#50113),.UNSPECIFIED.,.F.,.F.,(4,1,1,
1,1,1,1,1,4),(53.4070751110265,53.6233890926367,54.622022326751,55.6206555608652,
56.6192887949795,57.6179220290938,58.616555263208,59.6151884973223,59.6902604182061),
 .UNSPECIFIED.);
#1357=B_SPLINE_CURVE_WITH_KNOTS('',3,(#50118,#50119,#50120,#50121,#50122,
#50123,#50124,#50125,#50126,#50127),.UNSPECIFIED.,.F.,.F.,(4,1,1,1,1,1,
1,4),(47.1238898038469,47.9361714635051,48.9348046976194,49.9334379317336,
50.9320711658479,51.9307043999621,52.9293376340764,53.4070751110265),
 .UNSPECIFIED.);
#1358=B_SPLINE_CURVE_WITH_KNOTS('',3,(#50128,#50129,#50130,#50131,#50132,
#50133,#50134,#50135,#50136,#50137),.UNSPECIFIED.,.F.,.F.,(4,1,1,1,1,1,
1,4),(47.1238898038469,47.6315896879512,48.6302229220655,49.6288561561797,
50.627489390294,51.6261226244082,52.6247558585225,53.4070751110265),
 .UNSPECIFIED.);
#1359=B_SPLINE_CURVE_WITH_KNOTS('',3,(#50142,#50143,#50144,#50145,#50146,
#50147,#50148,#50149,#50150,#50151,#50152),.UNSPECIFIED.,.F.,.F.,(4,1,1,
1,1,1,1,1,4),(40.8407044966673,40.9457388247053,41.9443720588196,42.9430052929338,
43.9416385270481,44.9402717611624,45.9389049952766,46.9375382293909,47.1238898038469),
 .UNSPECIFIED.);
#1360=B_SPLINE_CURVE_WITH_KNOTS('',3,(#50153,#50154,#50155,#50156,#50157,
#50158,#50159,#50160,#50161,#50162),.UNSPECIFIED.,.F.,.F.,(4,1,1,1,1,1,
1,4),(40.8407044966673,41.6397902832657,42.6384235173799,43.6370567514942,
44.6356899856084,45.6343232197227,46.6329564538369,47.1238898038469),
 .UNSPECIFIED.);
#1361=B_SPLINE_CURVE_WITH_KNOTS('',3,(#50167,#50168,#50169,#50170,#50171,
#50172,#50173,#50174,#50175,#50176),.UNSPECIFIED.,.F.,.F.,(4,1,1,1,1,1,
1,4),(34.5575191894877,34.9539394200198,35.9525726541341,36.9512058882483,
37.9498391223626,38.9484723564768,39.9471055905911,40.8407044966673),
 .UNSPECIFIED.);
#1362=B_SPLINE_CURVE_WITH_KNOTS('',3,(#50177,#50178,#50179,#50180,#50181,
#50182,#50183,#50184,#50185,#50186,#50187),.UNSPECIFIED.,.F.,.F.,(4,1,1,
1,1,1,1,1,4),(34.5575191894877,34.6493576444659,35.6479908785801,36.6466241126944,
37.6452573468086,38.6438905809229,39.6425238150372,40.6411570491514,40.8407044966673),
 .UNSPECIFIED.);
#1363=B_SPLINE_CURVE_WITH_KNOTS('',3,(#50192,#50193,#50194,#50195,#50196,
#50197,#50198,#50199,#50200,#50201),.UNSPECIFIED.,.F.,.F.,(4,1,1,1,1,1,
1,4),(28.2743338823081,28.9621400153343,29.9607732494485,30.9594064835628,
31.958039717677,32.9566729517913,33.9553061859055,34.5575191894877),
 .UNSPECIFIED.);
#1364=B_SPLINE_CURVE_WITH_KNOTS('',3,(#50202,#50203,#50204,#50205,#50206,
#50207,#50208,#50209,#50210,#50211),.UNSPECIFIED.,.F.,.F.,(4,1,1,1,1,1,
1,4),(28.2743338823081,28.6575582397804,29.6561914738946,30.6548247080089,
31.6534579421231,32.6520911762374,33.6507244103516,34.5575191894877),
 .UNSPECIFIED.);
#1365=B_SPLINE_CURVE_WITH_KNOTS('',3,(#50216,#50217,#50218,#50219,#50220,
#50221,#50222,#50223,#50224,#50225),.UNSPECIFIED.,.F.,.F.,(4,1,1,1,1,1,
1,4),(21.9911485751286,22.9703406106487,23.968973844763,24.9676070788772,
25.9662403129915,26.9648735471058,27.96350678122,28.2743338823081),
 .UNSPECIFIED.);
#1366=B_SPLINE_CURVE_WITH_KNOTS('',3,(#50226,#50227,#50228,#50229,#50230,
#50231,#50232,#50233,#50234,#50235),.UNSPECIFIED.,.F.,.F.,(4,1,1,1,1,1,
1,4),(21.9911485751285,22.6657588350948,23.6643920692091,24.6630253033233,
25.6616585374376,26.6602917715518,27.6589250056661,28.2743338823081),
 .UNSPECIFIED.);
#1367=B_SPLINE_CURVE_WITH_KNOTS('',3,(#50237,#50238,#50239,#50240,#50241,
#50242,#50243,#50244,#50245,#50246,#50247,#50248,#50249,#50250,#50251,#50252,
#50253,#50254,#50255,#50256,#50257,#50258,#50259,#50260,#50261,#50262,#50263,
#50264,#50265,#50266,#50267,#50268,#50269,#50270,#50271,#50272,#50273,#50274,
#50275,#50276,#50277,#50278,#50279,#50280,#50281,#50282,#50283,#50284,#50285,
#50286,#50287,#50288,#50289,#50290,#50291,#50292,#50293,#50294,#50295,#50296,
#50297,#50298,#50299,#50300,#50301,#50302,#50303),.UNSPECIFIED.,.F.,.F.,
(4,3,3,3,3,3,3,3,3,3,3,3,3,3,3,3,3,3,3,3,3,3,4),(-0.744397949170599,-0.723512326373845,
-0.67814128146552,-0.660070814808423,-0.64143235554036,-0.603511610277582,
-0.580894867390611,-0.559926333296091,-0.499651315427941,-0.461264137672083,
-0.440585195641156,-0.425519770416711,-0.378746357789259,-0.331403063065602,
-0.308554318991755,-0.284756837114195,-0.222432053558095,-0.166824040168571,
-0.151081566327468,-0.135602715089046,-0.067801357544523,-0.0036955840594098,
0.),.UNSPECIFIED.);
#1368=B_SPLINE_CURVE_WITH_KNOTS('',3,(#50306,#50307,#50308,#50309,#50310,
#50311,#50312,#50313,#50314,#50315,#50316,#50317,#50318,#50319,#50320,#50321,
#50322,#50323,#50324,#50325,#50326,#50327,#50328,#50329,#50330,#50331,#50332,
#50333,#50334,#50335,#50336,#50337,#50338,#50339,#50340,#50341,#50342,#50343,
#50344,#50345,#50346,#50347,#50348,#50349,#50350,#50351,#50352,#50353,#50354,
#50355,#50356,#50357,#50358,#50359,#50360,#50361,#50362,#50363,#50364,#50365,
#50366),.UNSPECIFIED.,.F.,.F.,(4,3,3,3,3,3,3,3,3,3,3,3,3,3,3,3,3,3,3,3,
4),(-0.741270768406385,-0.716169767752366,-0.669333551356706,-0.640523177314207,
-0.621116769028352,-0.55668187280839,-0.539299960590835,-0.476625058521356,
-0.415643967217881,-0.398597659266647,-0.383300584194447,-0.34148003658708,
-0.279262972561836,-0.262172158015018,-0.245773277293746,-0.18432995797031,
-0.134120924057982,-0.117952339761776,-0.0589761698808879,-0.00426655107714081,
0.),.UNSPECIFIED.);
#1369=B_SPLINE_CURVE_WITH_KNOTS('',3,(#50951,#50952,#50953,#50954),
 .UNSPECIFIED.,.F.,.F.,(4,4),(140.259980297833,140.743350880823),
 .UNSPECIFIED.);
#1370=B_SPLINE_CURVE_WITH_KNOTS('',3,(#50956,#50957,#50958,#50959,#50960,
#50961,#50962,#50963,#50964,#50965,#50966,#50967,#50968,#50969,#50970,#50971,
#50972,#50973,#50974,#50975,#50976,#50977,#50978,#50979,#50980,#50981,#50982,
#50983,#50984,#50985,#50986,#50987,#50988,#50989,#50990,#50991,#50992,#50993,
#50994,#50995,#50996,#50997,#50998,#50999,#51000,#51001,#51002,#51003,#51004,
#51005,#51006,#51007,#51008,#51009,#51010,#51011,#51012,#51013,#51014,#51015,
#51016,#51017,#51018,#51019,#51020,#51021,#51022),.UNSPECIFIED.,.F.,.F.,
(4,3,3,3,3,3,3,3,3,3,3,3,3,3,3,3,3,3,3,3,3,3,4),(-0.744397949170588,-0.723512326373835,
-0.678141283557063,-0.660070791965409,-0.641432356264828,-0.603511105696609,
-0.580893242636312,-0.559926125386239,-0.49965110747392,-0.461263890974675,
-0.440584493156864,-0.425519175711549,-0.378746357789258,-0.331403063065601,
-0.308554312972659,-0.284756838770636,-0.222432070198544,-0.166824052648908,
-0.151081614936169,-0.135602719887486,-0.0678013599437428,-0.00369554913725607,
0.),.UNSPECIFIED.);
#1371=B_SPLINE_CURVE_WITH_KNOTS('',3,(#51023,#51024,#51025,#51026,#51027,
#51028,#51029,#51030,#51031,#51032),.UNSPECIFIED.,.F.,.F.,(4,1,1,1,1,1,
1,4),(15.7392613255823,16.6739594304093,17.6725926645235,18.6712258986378,
19.6698591327521,20.6684923668663,21.6671256009806,21.9911485751285),
 .UNSPECIFIED.);
#1372=B_SPLINE_CURVE_WITH_KNOTS('',3,(#51035,#51036,#51037,#51038,#51039,
#51040,#51041,#51042,#51043,#51044,#51045,#51046,#51047,#51048,#51049,#51050,
#51051,#51052,#51053,#51054,#51055,#51056,#51057,#51058,#51059,#51060,#51061,
#51062,#51063,#51064,#51065,#51066,#51067,#51068,#51069,#51070,#51071,#51072,
#51073,#51074,#51075,#51076,#51077,#51078,#51079,#51080,#51081,#51082,#51083,
#51084,#51085,#51086,#51087,#51088,#51089,#51090,#51091,#51092,#51093,#51094,
#51095),.UNSPECIFIED.,.F.,.F.,(4,3,3,3,3,3,3,3,3,3,3,3,3,3,3,3,3,3,3,3,
4),(-0.741270768406348,-0.71616976775233,-0.669333551356673,-0.640523157685122,
-0.621116757431072,-0.556681858729078,-0.539299941990702,-0.476625031186337,
-0.415643911212875,-0.398597683318881,-0.383300587660851,-0.341480036587073,
-0.279263169943563,-0.262173473385454,-0.245773527378364,-0.184330145533773,
-0.134121233214564,-0.117952257539906,-0.0589761287699529,-0.00426656137973672,
0.),.UNSPECIFIED.);
#1373=B_SPLINE_CURVE_WITH_KNOTS('',3,(#51098,#51099,#51100,#51101,#51102,
#51103,#51104,#51105,#51106),.UNSPECIFIED.,.F.,.F.,(4,1,1,1,1,1,4),(16.9785412059632,
17.9771744400775,18.9758076741917,19.974440908306,20.9730741424202,21.9717073765345,
21.9911485751286),.UNSPECIFIED.);
#1374=B_SPLINE_CURVE_WITH_KNOTS('',3,(#52488,#52489,#52490,#52491,#52492,
#52493,#52494,#52495,#52496,#52497,#52498),.UNSPECIFIED.,.F.,.F.,(4,1,1,
1,1,1,1,1,4),(53.4070751110265,53.7139797041847,54.204378086024,54.6947764678633,
55.1851748497026,55.6755732315419,56.1659716133811,56.6563699952204,56.8720816739404),
 .UNSPECIFIED.);
#1375=B_SPLINE_CURVE_WITH_KNOTS('',3,(#52501,#52502,#52503,#52504,#52505,
#52506,#52507,#52508,#52509,#52510),.UNSPECIFIED.,.F.,.F.,(4,1,1,1,1,1,
1,4),(53.4070751110265,53.622996627145,54.1133950089843,54.6037933908236,
55.0941917726629,55.5845901545022,56.0749885363415,56.5653869181807),
 .UNSPECIFIED.);
#1376=B_SPLINE_CURVE_WITH_KNOTS('',3,(#52515,#52516,#52517,#52518,#52519,
#52520,#52521,#52522,#52523,#52524,#52525,#52526,#52527,#52528,#52529,#52530,
#52531),.UNSPECIFIED.,.F.,.F.,(4,1,1,1,1,1,1,1,1,1,1,1,1,1,4),(47.1238898038469,
47.338800740274,47.8291991221133,48.3195975039526,48.8099958857919,49.3003942676312,
49.7907926494704,50.2811910313097,50.771589413149,51.2619877949883,51.7523861768276,
52.2427845586669,52.7331829405062,53.2235813223454,53.4070751110265),
 .UNSPECIFIED.);
#1377=B_SPLINE_CURVE_WITH_KNOTS('',3,(#52532,#52533,#52534,#52535,#52536,
#52537,#52538,#52539,#52540,#52541,#52542,#52543,#52544,#52545,#52546,#52547,
#52548),.UNSPECIFIED.,.F.,.F.,(4,1,1,1,1,1,1,1,1,1,1,1,1,1,4),(47.1238898038469,
47.2478176632343,47.7382160450736,48.2286144269129,48.7190128087522,49.2094111905915,
49.6998095724308,50.1902079542701,50.6806063361093,51.1710047179486,51.6614030997879,
52.1518014816272,52.6421998634665,53.1325982453058,53.4070751110265),
 .UNSPECIFIED.);
#1378=B_SPLINE_CURVE_WITH_KNOTS('',3,(#52553,#52554,#52555,#52556,#52557,
#52558,#52559,#52560,#52561,#52562,#52563,#52564,#52565,#52566,#52567,#52568,
#52569),.UNSPECIFIED.,.F.,.F.,(4,1,1,1,1,1,1,1,1,1,1,1,1,1,4),(40.8407044966673,
40.9636217763633,41.4540201582026,41.9444185400419,42.4348169218812,42.9252153037205,
43.4156136855598,43.906012067399,44.3964104492383,44.8868088310776,45.3772072129169,
45.8676055947562,46.3580039765955,46.8484023584347,47.1238898038469),
 .UNSPECIFIED.);
#1379=B_SPLINE_CURVE_WITH_KNOTS('',3,(#52570,#52571,#52572,#52573,#52574,
#52575,#52576,#52577,#52578,#52579,#52580,#52581,#52582,#52583,#52584,#52585,
#52586),.UNSPECIFIED.,.F.,.F.,(4,1,1,1,1,1,1,1,1,1,1,1,1,1,4),(40.8407044966673,
40.8726386993237,41.3630370811629,41.8534354630022,42.3438338448415,42.8342322266808,
43.3246306085201,43.8150289903594,44.3054273721986,44.7958257540379,45.2862241358772,
45.7766225177165,46.2670208995558,46.7574192813951,47.1238898038469),
 .UNSPECIFIED.);
#1380=B_SPLINE_CURVE_WITH_KNOTS('',3,(#52591,#52592,#52593,#52594,#52595,
#52596,#52597,#52598,#52599,#52600,#52601,#52602,#52603,#52604,#52605,#52606,
#52607),.UNSPECIFIED.,.F.,.F.,(4,1,1,1,1,1,1,1,1,1,1,1,1,1,4),(34.5575191894877,
34.5884428124527,35.0788411942919,35.5692395761312,36.0596379579705,36.5500363398098,
37.0404347216491,37.5308331034883,38.0212314853276,38.5116298671669,39.0020282490062,
39.4924266308455,39.9828250126848,40.4732233945241,40.8407044966673),
 .UNSPECIFIED.);
#1381=B_SPLINE_CURVE_WITH_KNOTS('',3,(#52608,#52609,#52610,#52611,#52612,
#52613,#52614,#52615,#52616,#52617,#52618,#52619,#52620,#52621,#52622,#52623),
 .UNSPECIFIED.,.F.,.F.,(4,1,1,1,1,1,1,1,1,1,1,1,1,4),(34.5575191894877,
34.9878581172523,35.4782564990915,35.9686548809308,36.4590532627701,36.9494516446094,
37.4398500264487,37.930248408288,38.4206467901272,38.9110451719665,39.4014435538058,
39.8918419356451,40.3822403174844,40.8407044966673),.UNSPECIFIED.);
#1382=B_SPLINE_CURVE_WITH_KNOTS('',3,(#52628,#52629,#52630,#52631,#52632,
#52633,#52634,#52635,#52636,#52637,#52638,#52639,#52640,#52641,#52642,#52643),
 .UNSPECIFIED.,.F.,.F.,(4,1,1,1,1,1,1,1,1,1,1,1,1,4),(28.2743338823081,
28.7036622303812,29.1940606122205,29.6844589940598,30.1748573758991,30.6652557577384,
31.1556541395777,31.6460525214169,32.1364509032562,32.6268492850955,33.1172476669348,
33.6076460487741,34.0980444306134,34.5575191894877),.UNSPECIFIED.);
#1383=B_SPLINE_CURVE_WITH_KNOTS('',3,(#52644,#52645,#52646,#52647,#52648,
#52649,#52650,#52651,#52652,#52653,#52654,#52655,#52656,#52657,#52658,#52659,
#52660),.UNSPECIFIED.,.F.,.F.,(4,1,1,1,1,1,1,1,1,1,1,1,1,1,4),(28.2743338823081,
28.6126791533416,29.1030775351808,29.5934759170201,30.0838742988594,30.5742726806987,
31.064671062538,31.5550694443773,32.0454678262166,32.5358662080558,33.0262645898951,
33.5166629717344,34.0070613535737,34.497459735413,34.5575191894877),
 .UNSPECIFIED.);
#1384=B_SPLINE_CURVE_WITH_KNOTS('',3,(#52665,#52666,#52667,#52668,#52669,
#52670,#52671,#52672,#52673,#52674,#52675,#52676,#52677,#52678,#52679,#52680,
#52681),.UNSPECIFIED.,.F.,.F.,(4,1,1,1,1,1,1,1,1,1,1,1,1,1,4),(21.9911485751285,
22.3284832664706,22.8188816483098,23.3092800301491,23.7996784119884,24.2900767938277,
24.780475175667,25.2708735575063,25.7612719393455,26.2516703211848,26.7420687030241,
27.2324670848634,27.7228654667027,28.213263848542,28.2743338823081),
 .UNSPECIFIED.);
#1385=B_SPLINE_CURVE_WITH_KNOTS('',3,(#52682,#52683,#52684,#52685,#52686,
#52687,#52688,#52689,#52690,#52691,#52692,#52693,#52694,#52695,#52696,#52697,
#52698),.UNSPECIFIED.,.F.,.F.,(4,1,1,1,1,1,1,1,1,1,1,1,1,1,4),(21.9911485751285,
22.2375001894309,22.7278985712702,23.2182969531094,23.7086953349487,24.199093716788,
24.6894920986273,25.1798904804666,25.6702888623059,26.1606872441451,26.6510856259844,
27.1414840078237,27.631882389663,28.1222807715023,28.2743338823081),
 .UNSPECIFIED.);
#1386=B_SPLINE_CURVE_WITH_KNOTS('',3,(#52703,#52704,#52705,#52706,#52707,
#52708,#52709,#52710,#52711,#52712,#52713,#52714,#52715,#52716,#52717,#52718,
#52719),.UNSPECIFIED.,.F.,.F.,(4,1,1,1,1,1,1,1,1,1,1,1,1,1,4),(15.7079632679489,
15.9533043025599,16.4437026843991,16.9341010662384,17.4244994480777,17.914897829917,
18.4052962117563,18.8956945935956,19.3860929754348,19.8764913572741,20.3668897391134,
20.8572881209527,21.347686502792,21.8380848846313,21.9911485751285),
 .UNSPECIFIED.);
#1387=B_SPLINE_CURVE_WITH_KNOTS('',3,(#52720,#52721,#52722,#52723,#52724,
#52725,#52726,#52727,#52728,#52729,#52730,#52731,#52732,#52733,#52734,#52735,
#52736),.UNSPECIFIED.,.F.,.F.,(4,1,1,1,1,1,1,1,1,1,1,1,1,1,4),(15.7079632679489,
15.8623212255202,16.3527196073595,16.8431179891988,17.333516371038,17.8239147528773,
18.3143131347166,18.8047115165559,19.2951098983952,19.7855082802345,20.2759066620737,
20.766305043913,21.2567034257523,21.7471018075916,21.9911485751285),
 .UNSPECIFIED.);
#1388=B_SPLINE_CURVE_WITH_KNOTS('',3,(#52743,#52744,#52745,#52746,#52747,
#52748,#52749,#52750,#52751,#52752,#52753,#52754,#52755,#52756,#52757,#52758),
 .UNSPECIFIED.,.F.,.F.,(4,1,1,1,1,1,1,1,1,1,1,1,1,4),(9.57812533864917,
10.0685237204885,10.5589221023277,11.049320484167,11.5397188660063,12.0301172478456,
12.5205156296849,13.0109140115242,13.5013123933634,13.9917107752027,14.482109157042,
14.9725075388813,15.4629059207206,15.7079632679489),.UNSPECIFIED.);
#1389=B_SPLINE_CURVE_WITH_KNOTS('',3,(#52759,#52760,#52761,#52762,#52763,
#52764,#52765,#52766,#52767,#52768,#52769,#52770,#52771,#52772,#52773,#52774,
#52775),.UNSPECIFIED.,.F.,.F.,(4,1,1,1,1,1,1,1,1,1,1,1,1,1,4),(9.42477796076936,
9.4871422616095,9.97754064344878,10.4679390252881,10.9583374071273,11.4487357889666,
11.9391341708059,12.4295325526452,12.9199309344845,13.4103293163238,13.9007276981631,
14.3911260800023,14.8815244618416,15.3719228436809,15.7079632679489),
 .UNSPECIFIED.);
#1390=B_SPLINE_CURVE_WITH_KNOTS('',3,(#52781,#52782,#52783,#52784,#52785,
#52786,#52787,#52788,#52789,#52790,#52791,#52792,#52793,#52794,#52795,#52796),
 .UNSPECIFIED.,.F.,.F.,(4,3,3,3,3,4),(-4.09323272002469,-3.96713944972556,
-3.47124701850987,-2.97535458729417,-2.47946215607848,-2.07135887395548),
 .UNSPECIFIED.);
#1391=B_SPLINE_CURVE_WITH_KNOTS('',3,(#52799,#52800,#52801,#52802,#52803,
#52804,#52805,#52806,#52807,#52808),.UNSPECIFIED.,.F.,.F.,(4,3,3,4),(0.,
0.495892431215694,0.991784862431392,1.11971880752058),.UNSPECIFIED.);
#1392=B_SPLINE_CURVE_WITH_KNOTS('',3,(#52813,#52814,#52815,#52816,#52817,
#52818,#52819,#52820,#52821,#52822,#52823,#52824,#52825,#52826,#52827,#52828,
#52829,#52830,#52831,#52832,#52833,#52834,#52835,#52836,#52837,#52838,#52839,
#52840,#52841,#52842,#52843,#52844,#52845,#52846,#52847,#52848,#52849,#52850,
#52851,#52852),.UNSPECIFIED.,.F.,.F.,(4,3,3,3,3,3,3,3,3,3,3,3,3,4),(-10.3764180272043,
-9.91784862431391,-9.42195619309822,-8.92606376188252,-8.43017133066683,
-7.93427889945113,-7.43838646823544,-6.94249403701974,-6.44660160580404,
-5.95070917458835,-5.45481674337265,-4.95892431215696,-4.46303188094126,
-4.09323272002469),.UNSPECIFIED.);
#1393=B_SPLINE_CURVE_WITH_KNOTS('',3,(#52853,#52854,#52855,#52856,#52857,
#52858,#52859,#52860,#52861,#52862,#52863,#52864,#52865,#52866,#52867,#52868,
#52869,#52870,#52871,#52872,#52873,#52874,#52875,#52876,#52877,#52878,#52879,
#52880,#52881,#52882,#52883,#52884,#52885,#52886,#52887,#52888,#52889,#52890,
#52891,#52892),.UNSPECIFIED.,.F.,.F.,(4,3,3,3,3,3,3,3,3,3,3,3,3,4),(1.11971880752058,
1.48767729364709,1.98356972486278,2.47946215607848,2.97535458729418,3.47124701850987,
3.96713944972557,4.46303188094126,4.95892431215696,5.45481674337265,5.95070917458835,
6.44660160580405,6.94249403701974,7.40290411470016),.UNSPECIFIED.);
#1394=B_SPLINE_CURVE_WITH_KNOTS('',3,(#52897,#52898,#52899,#52900,#52901,
#52902,#52903,#52904,#52905,#52906,#52907,#52908,#52909,#52910,#52911,#52912,
#52913,#52914,#52915,#52916,#52917,#52918,#52919,#52920,#52921,#52922,#52923,
#52924,#52925,#52926,#52927,#52928,#52929,#52930,#52931,#52932,#52933,#52934,
#52935,#52936,#52937,#52938,#52939),.UNSPECIFIED.,.F.,.F.,(4,3,3,3,3,3,
3,3,3,3,3,3,3,3,4),(-16.6596033343839,-16.364450230118,-15.8685577989023,
-15.3726653676866,-14.8767729364709,-14.3808805052552,-13.8849880740395,
-13.3890956428238,-12.8932032116081,-12.3973107803924,-11.9014183491767,
-11.405525917961,-10.9096334867453,-10.4137410555296,-10.3764180272043),
 .UNSPECIFIED.);
#1395=B_SPLINE_CURVE_WITH_KNOTS('',3,(#52940,#52941,#52942,#52943,#52944,
#52945,#52946,#52947,#52948,#52949,#52950,#52951,#52952,#52953,#52954,#52955,
#52956,#52957,#52958,#52959,#52960,#52961,#52962,#52963,#52964,#52965,#52966,
#52967,#52968,#52969,#52970,#52971,#52972,#52973,#52974,#52975,#52976,#52977,
#52978,#52979,#52980,#52981,#52982),.UNSPECIFIED.,.F.,.F.,(4,3,3,3,3,3,
3,3,3,3,3,3,3,3,4),(7.40290411470016,7.43838646823544,7.93427889945113,
8.43017133066683,8.92606376188253,9.42195619309822,9.91784862431392,10.4137410555296,
10.9096334867453,11.405525917961,11.9014183491767,12.3973107803924,12.8932032116081,
13.3890956428238,13.6860894218797),.UNSPECIFIED.);
#1396=B_SPLINE_CURVE_WITH_KNOTS('',3,(#52987,#52988,#52989,#52990,#52991,
#52992,#52993,#52994,#52995,#52996,#52997,#52998,#52999,#53000,#53001,#53002,
#53003,#53004,#53005,#53006,#53007,#53008,#53009,#53010,#53011,#53012,#53013,
#53014,#53015,#53016,#53017,#53018,#53019,#53020,#53021,#53022,#53023,#53024,
#53025,#53026,#53027,#53028,#53029),.UNSPECIFIED.,.F.,.F.,(4,3,3,3,3,3,
3,3,3,3,3,3,3,3,4),(-22.9427886415634,-22.811051835922,-22.3151594047063,
-21.8192669734906,-21.3233745422749,-20.8274821110592,-20.3315896798435,
-19.8356972486278,-19.3398048174121,-18.8439123861964,-18.3480199549807,
-17.852127523765,-17.3562350925493,-16.8603426613336,-16.6596033343839),
 .UNSPECIFIED.);
#1397=B_SPLINE_CURVE_WITH_KNOTS('',3,(#53030,#53031,#53032,#53033,#53034,
#53035,#53036,#53037,#53038,#53039,#53040,#53041,#53042,#53043,#53044,#53045,
#53046,#53047,#53048,#53049,#53050,#53051,#53052,#53053,#53054,#53055,#53056,
#53057,#53058,#53059,#53060,#53061,#53062,#53063,#53064,#53065,#53066,#53067,
#53068,#53069,#53070,#53071,#53072),.UNSPECIFIED.,.F.,.F.,(4,3,3,3,3,3,
3,3,3,3,3,3,3,3,4),(13.6860894218797,13.8849880740395,14.3808805052552,
14.8767729364709,15.3726653676866,15.8685577989023,16.364450230118,16.8603426613337,
17.3562350925494,17.8521275237651,18.3480199549808,18.8439123861965,19.3398048174122,
19.8356972486278,19.9692747290593),.UNSPECIFIED.);
#1398=B_SPLINE_CURVE_WITH_KNOTS('',3,(#53077,#53078,#53079,#53080,#53081,
#53082,#53083,#53084,#53085,#53086,#53087,#53088,#53089,#53090,#53091,#53092,
#53093,#53094,#53095,#53096,#53097,#53098,#53099,#53100,#53101,#53102,#53103,
#53104,#53105,#53106,#53107,#53108,#53109,#53110,#53111,#53112,#53113,#53114,
#53115,#53116),.UNSPECIFIED.,.F.,.F.,(4,3,3,3,3,3,3,3,3,3,3,3,3,4),(-29.225973948743,
-28.7617610105103,-28.2658685792946,-27.7699761480789,-27.2740837168633,
-26.7781912856476,-26.2822988544319,-25.7864064232162,-25.2905139920005,
-24.7946215607848,-24.2987291295691,-23.8028366983534,-23.3069442671377,
-22.9427886415634),.UNSPECIFIED.);
#1399=B_SPLINE_CURVE_WITH_KNOTS('',3,(#53117,#53118,#53119,#53120,#53121,
#53122,#53123,#53124,#53125,#53126,#53127,#53128,#53129,#53130,#53131,#53132,
#53133,#53134,#53135,#53136,#53137,#53138,#53139,#53140,#53141,#53142,#53143,
#53144,#53145,#53146,#53147,#53148,#53149,#53150,#53151,#53152,#53153,#53154,
#53155,#53156),.UNSPECIFIED.,.F.,.F.,(4,3,3,3,3,3,3,3,3,3,3,3,3,4),(19.9692747290593,
20.3315896798435,20.8274821110592,21.3233745422749,21.8192669734906,22.3151594047063,
22.811051835922,23.3069442671377,23.8028366983534,24.2987291295691,24.7946215607848,
25.2905139920005,25.7864064232162,26.2524600362389),.UNSPECIFIED.);
#1400=B_SPLINE_CURVE_WITH_KNOTS('',3,(#53161,#53162,#53163,#53164,#53165,
#53166,#53167,#53168,#53169,#53170,#53171,#53172,#53173,#53174,#53175,#53176,
#53177,#53178,#53179,#53180,#53181,#53182,#53183,#53184,#53185,#53186,#53187,
#53188,#53189,#53190,#53191,#53192,#53193,#53194,#53195,#53196,#53197,#53198,
#53199,#53200,#53201,#53202,#53203),.UNSPECIFIED.,.F.,.F.,(4,3,3,3,3,3,
3,3,3,3,3,3,3,3,4),(-35.5091592559226,-35.2083626163144,-34.7124701850987,
-34.216577753883,-33.7206853226673,-33.2247928914516,-32.7289004602359,
-32.2330080290202,-31.7371155978045,-31.2412231665888,-30.7453307353731,
-30.2494383041574,-29.7535458729417,-29.2576534417261,-29.225973948743),
 .UNSPECIFIED.);
#1401=B_SPLINE_CURVE_WITH_KNOTS('',3,(#53204,#53205,#53206,#53207,#53208,
#53209,#53210,#53211,#53212,#53213,#53214,#53215,#53216,#53217,#53218,#53219,
#53220,#53221,#53222,#53223,#53224,#53225,#53226,#53227,#53228,#53229,#53230,
#53231,#53232,#53233,#53234,#53235,#53236,#53237,#53238,#53239,#53240,#53241,
#53242,#53243,#53244,#53245,#53246),.UNSPECIFIED.,.F.,.F.,(4,3,3,3,3,3,
3,3,3,3,3,3,3,3,4),(26.2524600362389,26.2822988544319,26.7781912856476,
27.2740837168633,27.769976148079,28.2658685792947,28.7617610105104,29.2576534417261,
29.7535458729418,30.2494383041575,30.7453307353731,31.2412231665888,31.7371155978045,
32.2330080290202,32.5356453434185),.UNSPECIFIED.);
#1402=B_SPLINE_CURVE_WITH_KNOTS('',3,(#53251,#53252,#53253,#53254,#53255,
#53256,#53257,#53258,#53259,#53260,#53261,#53262,#53263,#53264,#53265,#53266,
#53267,#53268,#53269,#53270,#53271,#53272,#53273,#53274,#53275,#53276,#53277,
#53278,#53279,#53280,#53281,#53282,#53283,#53284,#53285,#53286,#53287,#53288,
#53289,#53290,#53291,#53292,#53293),.UNSPECIFIED.,.F.,.F.,(4,3,3,3,3,3,
3,3,3,3,3,3,3,3,4),(-41.7923445631022,-41.6549642221184,-41.1590717909027,
-40.663179359687,-40.1672869284713,-39.6713944972556,-39.1755020660399,
-38.6796096348243,-38.1837172036086,-37.6878247723929,-37.1919323411772,
-36.6960399099615,-36.2001474787458,-35.7042550475301,-35.5091592559226),
 .UNSPECIFIED.);
#1403=B_SPLINE_CURVE_WITH_KNOTS('',3,(#53294,#53295,#53296,#53297,#53298,
#53299,#53300,#53301,#53302,#53303,#53304,#53305,#53306,#53307,#53308,#53309,
#53310,#53311,#53312,#53313,#53314,#53315,#53316,#53317,#53318,#53319,#53320,
#53321,#53322,#53323,#53324,#53325,#53326,#53327,#53328,#53329,#53330,#53331,
#53332,#53333,#53334,#53335,#53336),.UNSPECIFIED.,.F.,.F.,(4,3,3,3,3,3,
3,3,3,3,3,3,3,3,4),(32.5356453434185,32.7289004602359,33.2247928914516,
33.7206853226673,34.216577753883,34.7124701850987,35.2083626163144,35.7042550475301,
36.2001474787458,36.6960399099615,37.1919323411772,37.6878247723929,38.1837172036086,
38.6796096348243,38.8188306505981),.UNSPECIFIED.);
#1404=B_SPLINE_CURVE_WITH_KNOTS('',3,(#53341,#53342,#53343,#53344,#53345,
#53346,#53347,#53348,#53349,#53350,#53351,#53352,#53353,#53354,#53355,#53356,
#53357,#53358,#53359,#53360,#53361,#53362,#53363,#53364,#53365,#53366,#53367,
#53368,#53369,#53370,#53371,#53372,#53373,#53374,#53375,#53376,#53377,#53378,
#53379,#53380),.UNSPECIFIED.,.F.,.F.,(4,3,3,3,3,3,3,3,3,3,3,3,3,4),(-48.0755298702818,
-47.6056733967068,-47.1097809654911,-46.6138885342754,-46.1179961030597,
-45.622103671844,-45.1262112406283,-44.6303188094126,-44.1344263781969,
-43.6385339469812,-43.1426415157655,-42.6467490845498,-42.1508566533341,
-41.7923445631022),.UNSPECIFIED.);
#1405=B_SPLINE_CURVE_WITH_KNOTS('',3,(#53381,#53382,#53383,#53384,#53385,
#53386,#53387,#53388,#53389,#53390,#53391,#53392,#53393,#53394,#53395,#53396,
#53397,#53398,#53399,#53400,#53401,#53402,#53403,#53404,#53405,#53406,#53407,
#53408,#53409,#53410,#53411,#53412,#53413,#53414,#53415,#53416,#53417,#53418,
#53419,#53420),.UNSPECIFIED.,.F.,.F.,(4,3,3,3,3,3,3,3,3,3,3,3,3,4),(38.8188306505981,
39.17550206604,39.6713944972557,40.1672869284714,40.6631793596871,41.1590717909028,
41.6549642221185,42.1508566533342,42.6467490845498,43.1426415157655,43.6385339469812,
44.1344263781969,44.6303188094126,45.1020159577777),.UNSPECIFIED.);
#1406=B_SPLINE_CURVE_WITH_KNOTS('',3,(#53425,#53426,#53427,#53428,#53429,
#53430,#53431,#53432,#53433,#53434,#53435,#53436,#53437,#53438,#53439,#53440,
#53441,#53442,#53443,#53444,#53445,#53446,#53447,#53448,#53449,#53450,#53451,
#53452,#53453,#53454,#53455,#53456,#53457,#53458,#53459,#53460,#53461,#53462,
#53463,#53464,#53465,#53466,#53467),.UNSPECIFIED.,.F.,.F.,(4,3,3,3,3,3,
3,3,3,3,3,3,3,3,4),(-54.3587151774614,-54.0522750025108,-53.5563825712951,
-53.0604901400794,-52.5645977088637,-52.068705277648,-51.5728128464323,
-51.0769204152166,-50.5810279840009,-50.0851355527853,-49.5892431215696,
-49.0933506903539,-48.5974582591382,-48.1015658279225,-48.0755298702818),
 .UNSPECIFIED.);
#1407=B_SPLINE_CURVE_WITH_KNOTS('',3,(#53468,#53469,#53470,#53471,#53472,
#53473,#53474,#53475,#53476,#53477,#53478,#53479,#53480,#53481,#53482,#53483,
#53484,#53485,#53486,#53487,#53488,#53489,#53490,#53491,#53492,#53493,#53494,
#53495,#53496,#53497,#53498,#53499,#53500,#53501,#53502,#53503,#53504,#53505,
#53506,#53507,#53508,#53509,#53510),.UNSPECIFIED.,.F.,.F.,(4,3,3,3,3,3,
3,3,3,3,3,3,3,3,4),(45.1020159577777,45.1262112406283,45.622103671844,46.1179961030597,
46.6138885342754,47.1097809654911,47.6056733967068,48.1015658279225,48.5974582591382,
49.0933506903539,49.5892431215696,50.0851355527853,50.581027984001,51.0769204152167,
51.3852012649573),.UNSPECIFIED.);
#1408=B_SPLINE_CURVE_WITH_KNOTS('',3,(#53516,#53517,#53518,#53519,#53520,
#53521,#53522,#53523),.UNSPECIFIED.,.F.,.F.,(4,1,1,1,1,4),(65.9734457253856,
66.1628979816508,66.6587904128665,67.1546828440821,67.6505752752978,68.0586785574208),
 .UNSPECIFIED.);
#1409=B_SPLINE_CURVE_WITH_KNOTS('',3,(#53526,#53527,#53528,#53529,#53530),
 .UNSPECIFIED.,.F.,.F.,(4,1,4),(65.9734457253857,66.3244736054852,66.8203660367009),
 .UNSPECIFIED.);
#1410=B_SPLINE_CURVE_WITH_KNOTS('',3,(#53535,#53536,#53537,#53538,#53539,
#53540,#53541,#53542,#53543,#53544,#53545,#53546,#53547,#53548,#53549,#53550,
#53551),.UNSPECIFIED.,.F.,.F.,(4,1,1,1,1,1,1,1,1,1,1,1,1,1,4),(59.6902604182061,
59.7162963758467,60.2121888070624,60.7080812382781,61.2039736694938,61.6998661007095,
62.1957585319252,62.6916509631409,63.1875433943566,63.6834358255723,64.179328256788,
64.6752206880037,65.1711131192194,65.6670055504351,65.9734457253856),
 .UNSPECIFIED.);
#1411=B_SPLINE_CURVE_WITH_KNOTS('',3,(#53552,#53553,#53554,#53555,#53556,
#53557,#53558,#53559,#53560,#53561,#53562,#53563,#53564,#53565,#53566,#53567,
#53568),.UNSPECIFIED.,.F.,.F.,(4,1,1,1,1,1,1,1,1,1,1,1,1,1,4),(59.6902604182061,
59.8778719996811,60.3737644308968,60.8696568621125,61.3655492933282,61.8614417245439,
62.3573341557596,62.8532265869753,63.349119018191,63.8450114494067,64.3409038806224,
64.8367963118381,65.3326887430538,65.8285811742695,65.9734457253857),
 .UNSPECIFIED.);
#1412=B_SPLINE_CURVE_WITH_KNOTS('',3,(#53573,#53574,#53575,#53576,#53577,
#53578,#53579,#53580,#53581,#53582,#53583,#53584,#53585,#53586,#53587,#53588),
 .UNSPECIFIED.,.F.,.F.,(4,1,1,1,1,1,1,1,1,1,1,1,1,4),(53.4070751110265,
53.7655872012584,54.2614796324741,54.7573720636898,55.2532644949055,55.7491569261211,
56.2450493573368,56.7409417885525,57.2368342197682,57.7327266509839,58.2286190821996,
58.7245115134153,59.220403944631,59.6902604182061),.UNSPECIFIED.);
#1413=B_SPLINE_CURVE_WITH_KNOTS('',3,(#53589,#53590,#53591,#53592,#53593,
#53594,#53595,#53596,#53597,#53598,#53599,#53600,#53601,#53602,#53603,#53604,
#53605),.UNSPECIFIED.,.F.,.F.,(4,1,1,1,1,1,1,1,1,1,1,1,1,1,4),(53.4070751110265,
53.4312703938771,53.9271628250928,54.4230552563085,54.9189476875242,55.4148401187399,
55.9107325499556,56.4066249811712,56.9025174123869,57.3984098436026,57.8943022748183,
58.390194706034,58.8860871372497,59.3819795684654,59.6902604182061),
 .UNSPECIFIED.);
#1414=B_SPLINE_CURVE_WITH_KNOTS('',3,(#53610,#53611,#53612,#53613,#53614,
#53615,#53616,#53617,#53618,#53619,#53620,#53621,#53622,#53623,#53624,#53625,
#53626),.UNSPECIFIED.,.F.,.F.,(4,1,1,1,1,1,1,1,1,1,1,1,1,1,4),(47.1238898038469,
47.3189855954543,47.81487802667,48.3107704578857,48.8066628891014,49.3025553203171,
49.7984477515328,50.2943401827485,50.7902326139642,51.2861250451799,51.7820174763956,
52.2779099076113,52.773802338827,53.2696947700427,53.4070751110265),
 .UNSPECIFIED.);
#1415=B_SPLINE_CURVE_WITH_KNOTS('',3,(#53627,#53628,#53629,#53630,#53631,
#53632,#53633,#53634,#53635,#53636,#53637,#53638,#53639,#53640,#53641,#53642),
 .UNSPECIFIED.,.F.,.F.,(4,1,1,1,1,1,1,1,1,1,1,1,1,4),(47.1238898038469,
47.4805612192887,47.9764536505044,48.4723460817201,48.9682385129358,49.4641309441515,
49.9600233753672,50.4559158065829,50.9518082377986,51.4477006690143,51.94359310023,
52.4394855314457,52.9353779626614,53.4070751110265),.UNSPECIFIED.);
#1416=B_SPLINE_CURVE_WITH_KNOTS('',3,(#53647,#53648,#53649,#53650,#53651,
#53652,#53653,#53654,#53655,#53656,#53657,#53658,#53659,#53660,#53661,#53662,
#53663),.UNSPECIFIED.,.F.,.F.,(4,1,1,1,1,1,1,1,1,1,1,1,1,1,4),(40.8407044966673,
40.8723839896503,41.368276420866,41.8641688520817,42.3600612832974,42.8559537145131,
43.3518461457288,43.8477385769445,44.3436310081602,44.8395234393758,45.3354158705915,
45.8313083018072,46.3272007330229,46.8230931642386,47.1238898038469),
 .UNSPECIFIED.);
#1417=B_SPLINE_CURVE_WITH_KNOTS('',3,(#53664,#53665,#53666,#53667,#53668,
#53669,#53670,#53671,#53672,#53673,#53674,#53675,#53676,#53677,#53678,#53679,
#53680),.UNSPECIFIED.,.F.,.F.,(4,1,1,1,1,1,1,1,1,1,1,1,1,1,4),(40.8407044966673,
41.0339596134847,41.5298520447004,42.0257444759161,42.5216369071318,43.0175293383475,
43.5134217695632,44.0093142007789,44.5052066319946,45.0010990632102,45.4969914944259,
45.9928839256416,46.4887763568573,46.984668788073,47.1238898038469),
 .UNSPECIFIED.);
#1418=B_SPLINE_CURVE_WITH_KNOTS('',3,(#53685,#53686,#53687,#53688,#53689,
#53690,#53691,#53692,#53693,#53694,#53695,#53696,#53697,#53698,#53699,#53700),
 .UNSPECIFIED.,.F.,.F.,(4,1,1,1,1,1,1,1,1,1,1,1,1,4),(34.5575191894877,
34.9216748150619,35.4175672462776,35.9134596774933,36.409352108709,36.9052445399247,
37.4011369711404,37.8970294023561,38.3929218335718,38.8888142647875,39.3847066960032,
39.8805991272189,40.3764915584346,40.8407044966673),.UNSPECIFIED.);
#1419=B_SPLINE_CURVE_WITH_KNOTS('',3,(#53701,#53702,#53703,#53704,#53705,
#53706,#53707,#53708,#53709,#53710,#53711,#53712,#53713,#53714,#53715,#53716,
#53717),.UNSPECIFIED.,.F.,.F.,(4,1,1,1,1,1,1,1,1,1,1,1,1,1,4),(34.5575191894877,
34.5873580076806,35.0832504388963,35.579142870112,36.0750353013277,36.5709277325434,
37.0668201637591,37.5627125949748,38.0586050261905,38.5544974574062,39.0503898886219,
39.5462823198376,40.0421747510533,40.538067182269,40.8407044966673),
 .UNSPECIFIED.);
#1420=B_SPLINE_CURVE_WITH_KNOTS('',3,(#53722,#53723,#53724,#53725,#53726,
#53727,#53728,#53729,#53730,#53731,#53732,#53733,#53734,#53735,#53736,#53737,
#53738),.UNSPECIFIED.,.F.,.F.,(4,1,1,1,1,1,1,1,1,1,1,1,1,1,4),(28.2743338823081,
28.4750732092579,28.9709656404736,29.4668580716893,29.962750502905,30.4586429341207,
30.9545353653364,31.4504277965521,31.9463202277678,32.4422126589835,32.9381050901992,
33.4339975214149,33.9298899526305,34.4257823838462,34.5575191894877),
 .UNSPECIFIED.);
#1421=B_SPLINE_CURVE_WITH_KNOTS('',3,(#53739,#53740,#53741,#53742,#53743,
#53744,#53745,#53746,#53747,#53748,#53749,#53750,#53751,#53752,#53753,#53754),
 .UNSPECIFIED.,.F.,.F.,(4,1,1,1,1,1,1,1,1,1,1,1,1,4),(28.2743338823081,
28.6366488330923,29.132541264308,29.6284336955237,30.1243261267394,30.6202185579551,
31.1161109891708,31.6120034203865,32.1078958516022,32.6037882828178,33.0996807140335,
33.5955731452492,34.0914655764649,34.5575191894877),.UNSPECIFIED.);
#1422=B_SPLINE_CURVE_WITH_KNOTS('',3,(#53759,#53760,#53761,#53762,#53763,
#53764,#53765,#53766,#53767,#53768,#53769,#53770,#53771,#53772,#53773,#53774,
#53775),.UNSPECIFIED.,.F.,.F.,(4,1,1,1,1,1,1,1,1,1,1,1,1,1,4),(21.9911485751285,
22.0284716034539,22.5243640346695,23.0202564658852,23.5161488971009,24.0120413283166,
24.5079337595323,25.003826190748,25.4997186219637,25.9956110531794,26.4915034843951,
26.9873959156108,27.4832883468265,27.9791807780422,28.2743338823081),
 .UNSPECIFIED.);
#1423=B_SPLINE_CURVE_WITH_KNOTS('',3,(#53776,#53777,#53778,#53779,#53780,
#53781,#53782,#53783,#53784,#53785,#53786,#53787,#53788,#53789,#53790,#53791,
#53792),.UNSPECIFIED.,.F.,.F.,(4,1,1,1,1,1,1,1,1,1,1,1,1,1,4),(21.9911485751285,
22.1900472272882,22.6859396585039,23.1818320897196,23.6777245209353,24.173616952151,
24.6695093833667,25.1654018145824,25.6612942457981,26.1571866770138,26.6530791082295,
27.1489715394452,27.6448639706609,28.1407564018766,28.2743338823081),
 .UNSPECIFIED.);
#1424=B_SPLINE_CURVE_WITH_KNOTS('',3,(#53797,#53798,#53799,#53800,#53801,
#53802,#53803,#53804,#53805,#53806,#53807,#53808,#53809,#53810,#53811,#53812),
 .UNSPECIFIED.,.F.,.F.,(4,1,1,1,1,1,1,1,1,1,1,1,1,4),(15.7079632679489,
16.0777624288655,16.5736548600812,17.0695472912969,17.5654397225126,18.0613321537283,
18.557224584944,19.0531170161597,19.5490094473754,20.0449018785911,20.5407943098068,
21.0366867410225,21.5325791722382,21.9911485751285),.UNSPECIFIED.);
#1425=B_SPLINE_CURVE_WITH_KNOTS('',3,(#53813,#53814,#53815,#53816,#53817,
#53818,#53819,#53820,#53821,#53822,#53823,#53824,#53825,#53826,#53827,#53828,
#53829),.UNSPECIFIED.,.F.,.F.,(4,1,1,1,1,1,1,1,1,1,1,1,1,1,4),(15.7079632679489,
15.7434456214842,16.2393380526999,16.7352304839156,17.2311229151313,17.727015346347,
18.2229077775627,18.7188002087784,19.2146926399941,19.7105850712098,20.2064775024255,
20.7023699336412,21.1982623648568,21.6941547960725,21.9911485751285),
 .UNSPECIFIED.);
#1426=B_SPLINE_CURVE_WITH_KNOTS('',3,(#53832,#53833,#53834,#53835,#53836,
#53837,#53838,#53839,#53840,#53841,#53842,#53843,#53844,#53845,#53846,#53847,
#53848,#53849,#53850,#53851,#53852,#53853,#53854,#53855,#53856,#53857,#53858,
#53859,#53860,#53861,#53862,#53863,#53864,#53865,#53866,#53867,#53868,#53869,
#53870,#53871,#53872,#53873,#53874,#53875,#53876,#53877,#53878,#53879,#53880,
#53881,#53882,#53883,#53884,#53885,#53886,#53887,#53888,#53889,#53890,#53891,
#53892,#53893,#53894,#53895,#53896,#53897,#53898,#53899,#53900,#53901,#53902,
#53903,#53904,#53905,#53906,#53907),.UNSPECIFIED.,.F.,.F.,(4,3,3,3,3,3,
3,3,3,3,3,3,3,3,3,3,3,3,3,3,3,3,3,3,3,4),(-1.56128884155279,-1.49877186936406,
-1.40897117371964,-1.3789451251186,-1.34973794742057,-1.24465351710347,
-1.19072852613426,-1.16409839319326,-1.13956908678638,-1.0343472120063,
-0.958854548039817,-0.923551939224775,-0.900234537445069,-0.87856017707745,
-0.769660548406124,-0.674675099932122,-0.618451862218184,-0.590493256446276,
-0.481235354793128,-0.389718754510115,-0.339912463836043,-0.311813120045921,
-0.289600014462053,-0.179535399263025,-0.0689290207122846,0.),
 .UNSPECIFIED.);
#1427=B_SPLINE_CURVE_WITH_KNOTS('',3,(#53912,#53913,#53914,#53915,#53916,
#53917,#53918,#53919,#53920,#53921,#53922,#53923,#53924,#53925,#53926,#53927,
#53928,#53929,#53930,#53931,#53932,#53933,#53934,#53935,#53936,#53937,#53938,
#53939,#53940,#53941,#53942,#53943,#53944,#53945,#53946,#53947,#53948,#53949,
#53950,#53951,#53952,#53953,#53954,#53955,#53956,#53957,#53958,#53959,#53960,
#53961,#53962,#53963,#53964,#53965,#53966,#53967,#53968,#53969,#53970,#53971,
#53972,#53973,#53974,#53975,#53976,#53977,#53978,#53979,#53980,#53981,#53982,
#53983,#53984,#53985,#53986,#53987),.UNSPECIFIED.,.F.,.F.,(4,3,3,3,3,3,
3,3,3,3,3,3,3,3,3,3,3,3,3,3,3,3,3,3,3,4),(-1.55754822368995,-1.48810779253287,
-1.39149025036148,-1.35765137174339,-1.33135607863307,-1.21649685124019,
-1.16749625285341,-1.1349192461529,-1.10163762384731,-0.993163332584848,
-0.919274261648977,-0.861029472187144,-0.839159851919032,-0.732654366492018,
-0.724432241811757,-0.63260971160265,-0.577457931216515,-0.548301984883685,
-0.443554340183684,-0.35714212097533,-0.309118804342202,-0.283551498142216,
-0.26428345496014,-0.160948967379259,-0.0591655876679145,0.),
 .UNSPECIFIED.);
#1428=B_SPLINE_CURVE_WITH_KNOTS('',3,(#54472,#54473,#54474,#54475,#54476,
#54477,#54478,#54479,#54480,#54481,#54482,#54483,#54484,#54485,#54486,#54487,
#54488,#54489,#54490,#54491,#54492,#54493,#54494,#54495,#54496,#54497,#54498,
#54499,#54500,#54501,#54502,#54503,#54504,#54505),.UNSPECIFIED.,.F.,.F.,
(4,3,3,3,3,3,3,3,3,3,3,4),(51.3852012649573,51.5728128464324,52.0687052776481,
52.5645977088638,53.0604901400795,53.5563825712952,54.0522750025108,54.5481674337265,
55.0440598649422,55.5399522961579,56.0358447273736,56.4439480094966),
 .UNSPECIFIED.);
#1429=B_SPLINE_CURVE_WITH_KNOTS('',3,(#54507,#54508,#54509,#54510,#54511,
#54512,#54513,#54514,#54515,#54516,#54517,#54518,#54519,#54520,#54521,#54522,
#54523,#54524,#54525,#54526,#54527,#54528,#54529,#54530,#54531,#54532,#54533,
#54534,#54535,#54536,#54537,#54538,#54539,#54540,#54541,#54542,#54543,#54544,
#54545,#54546,#54547,#54548,#54549,#54550,#54551,#54552,#54553,#54554,#54555,
#54556,#54557,#54558,#54559,#54560,#54561,#54562,#54563,#54564,#54565,#54566,
#54567,#54568,#54569,#54570,#54571,#54572,#54573,#54574,#54575,#54576,#54577,
#54578,#54579,#54580,#54581,#54582),.UNSPECIFIED.,.F.,.F.,(4,3,3,3,3,3,
3,3,3,3,3,3,3,3,3,3,3,3,3,3,3,3,3,3,3,4),(-1.56128884155278,-1.49877186936405,
-1.40897117371963,-1.37894512088796,-1.34973794578355,-1.24465351628496,
-1.19072853582439,-1.16409839418051,-1.13956908678636,-1.03434721514391,
-0.958854555599736,-0.923551951909299,-0.900234570307523,-0.878560184924177,
-0.76966054840611,-0.674675099932109,-0.618451846751326,-0.590493252166945,
-0.481235352814289,-0.389718754510105,-0.339912466184574,-0.311813126525562,
-0.289600022326692,-0.179535354639491,-0.0689290178359763,0.),
 .UNSPECIFIED.);
#1430=B_SPLINE_CURVE_WITH_KNOTS('',3,(#54583,#54584,#54585,#54586,#54587,
#54588,#54589,#54590,#54591,#54592,#54593,#54594,#54595,#54596),
 .UNSPECIFIED.,.F.,.F.,(4,1,1,1,1,1,1,1,1,1,1,4),(10.3764180272042,10.7845213093272,
11.2804137405429,11.7763061717586,12.2721986029743,12.76809103419,13.2639834654057,
13.7598758966214,14.2557683278371,14.7516607590528,15.2475531902685,15.7079632679489),
 .UNSPECIFIED.);
#1431=B_SPLINE_CURVE_WITH_KNOTS('',3,(#54600,#54601,#54602,#54603,#54604,
#54605,#54606,#54607,#54608,#54609,#54610,#54611),.UNSPECIFIED.,.F.,.F.,
(4,1,1,1,1,1,1,1,1,4),(11.6147305479242,12.1106229791399,12.6065154103556,
13.1024078415713,13.598300272787,14.0941927040027,14.5900851352184,15.0859775664341,
15.5818699976498,15.7079632679489),.UNSPECIFIED.);
#1432=B_SPLINE_CURVE_WITH_KNOTS('',3,(#55096,#55097,#55098,#55099,#55100,
#55101,#55102,#55103,#55104,#55105,#55106,#55107,#55108,#55109,#55110,#55111,
#55112,#55113,#55114,#55115,#55116,#55117,#55118,#55119,#55120,#55121,#55122,
#55123,#55124,#55125,#55126,#55127,#55128,#55129,#55130,#55131,#55132,#55133,
#55134,#55135,#55136,#55137,#55138,#55139,#55140,#55141,#55142,#55143,#55144,
#55145,#55146,#55147,#55148,#55149,#55150,#55151,#55152,#55153,#55154,#55155,
#55156,#55157,#55158,#55159,#55160,#55161,#55162,#55163,#55164,#55165,#55166,
#55167,#55168,#55169,#55170,#55171),.UNSPECIFIED.,.F.,.F.,(4,3,3,3,3,3,
3,3,3,3,3,3,3,3,3,3,3,3,3,3,3,3,3,3,3,4),(-1.55754822368999,-1.48810779253295,
-1.39149025036156,-1.35765138493943,-1.33135610631869,-1.21649686508303,
-1.16749627584831,-1.1349192463022,-1.10163762384737,-0.993163329305883,
-0.919274250510989,-0.861029455716102,-0.839159838745014,-0.732654337878835,
-0.724432241811784,-0.632609711602674,-0.57745792727088,-0.548301986226071,
-0.443554379365538,-0.357142120975343,-0.309118815124666,-0.28355153569308,
-0.264283499949117,-0.160949023485775,-0.0591655579179677,0.),
 .UNSPECIFIED.);
#1433=B_SPLINE_CURVE_WITH_KNOTS('',3,(#55172,#55173,#55174,#55175,#55176,
#55177,#55178,#55179,#55180,#55181,#55182,#55183,#55184,#55185,#55186,#55187,
#55188,#55189,#55190,#55191,#55192,#55193,#55194,#55195,#55196,#55197,#55198,
#55199),.UNSPECIFIED.,.F.,.F.,(4,3,3,3,3,3,3,3,3,4),(-58.5153068834521,
-58.0194144522364,-57.5235220210207,-57.027629589805,-56.5317371585893,
-56.0358447273736,-55.5399522961579,-55.0440598649422,-54.5481674337265,
-54.3587151774614),.UNSPECIFIED.);
#1434=B_SPLINE_CURVE_WITH_KNOTS('',3,(#55709,#55710,#55711,#55712,#55713,
#55714,#55715,#55716),.UNSPECIFIED.,.F.,.F.,(4,2,2,4),(0.,0.303392014531485,
0.493985861454505,0.65589637197807),.UNSPECIFIED.);
#1435=B_SPLINE_CURVE_WITH_KNOTS('',3,(#55718,#55719,#55720,#55721,#55722,
#55723,#55724,#55725,#55726,#55727,#55728,#55729,#55730,#55731,#55732,#55733,
#55734,#55735,#55736,#55737,#55738,#55739,#55740,#55741,#55742,#55743,#55744,
#55745,#55746,#55747,#55748,#55749,#55750,#55751,#55752,#55753,#55754,#55755,
#55756,#55757,#55758,#55759,#55760,#55761,#55762,#55763,#55764,#55765,#55766,
#55767,#55768,#55769,#55770,#55771,#55772,#55773,#55774,#55775,#55776,#55777,
#55778,#55779,#55780,#55781,#55782,#55783,#55784,#55785,#55786,#55787,#55788,
#55789,#55790,#55791,#55792,#55793,#55794,#55795,#55796,#55797,#55798,#55799,
#55800,#55801,#55802,#55803,#55804,#55805,#55806,#55807,#55808,#55809,#55810,
#55811,#55812,#55813,#55814,#55815,#55816,#55817,#55818,#55819,#55820,#55821,
#55822,#55823,#55824,#55825,#55826,#55827,#55828,#55829,#55830,#55831,#55832,
#55833,#55834,#55835,#55836,#55837,#55838,#55839,#55840,#55841,#55842,#55843,
#55844,#55845,#55846,#55847,#55848,#55849,#55850,#55851,#55852,#55853,#55854,
#55855,#55856,#55857,#55858,#55859,#55860,#55861,#55862,#55863,#55864,#55865,
#55866,#55867,#55868,#55869,#55870,#55871,#55872,#55873,#55874,#55875,#55876,
#55877,#55878,#55879,#55880,#55881,#55882,#55883,#55884,#55885,#55886,#55887,
#55888,#55889,#55890,#55891,#55892,#55893,#55894,#55895,#55896,#55897,#55898,
#55899,#55900,#55901,#55902,#55903,#55904,#55905,#55906,#55907,#55908,#55909,
#55910,#55911,#55912,#55913,#55914,#55915,#55916,#55917,#55918,#55919,#55920,
#55921,#55922,#55923,#55924,#55925,#55926,#55927,#55928,#55929,#55930,#55931,
#55932,#55933,#55934,#55935,#55936,#55937,#55938,#55939,#55940,#55941,#55942,
#55943,#55944,#55945,#55946,#55947,#55948,#55949,#55950,#55951,#55952,#55953,
#55954,#55955,#55956,#55957,#55958,#55959,#55960,#55961,#55962,#55963,#55964,
#55965,#55966,#55967,#55968,#55969,#55970,#55971,#55972,#55973,#55974,#55975,
#55976,#55977,#55978,#55979,#55980,#55981,#55982,#55983,#55984,#55985,#55986,
#55987,#55988,#55989,#55990,#55991,#55992,#55993,#55994,#55995,#55996,#55997,
#55998,#55999,#56000,#56001,#56002,#56003,#56004,#56005,#56006,#56007,#56008,
#56009),.UNSPECIFIED.,.F.,.F.,(4,3,3,3,3,3,3,3,3,3,3,3,3,3,3,3,3,3,3,3,
3,3,3,3,3,3,3,3,3,3,3,3,3,3,3,3,3,3,3,3,3,3,3,3,3,3,3,3,3,3,3,3,3,3,3,3,
3,3,3,3,3,3,3,3,3,3,3,3,3,3,3,3,3,3,3,3,3,3,3,3,3,3,3,3,3,3,3,3,3,3,3,3,
3,3,3,3,3,4),(0.,0.490398381839284,0.980796763678567,1.47119514551785,1.96159352735714,
2.45199190919642,2.9423902910357,3.43278867287499,3.92318705471427,4.41358543655355,
4.90398381839284,5.39438220023212,5.88478058207141,6.37517896391069,6.86557734574997,
7.35597572758925,7.84637410942854,8.33677249126782,8.82717087310711,9.31756925494639,
9.80796763678567,10.298366018625,10.7887644004642,11.2791627823035,11.7695611641428,
12.2599595459821,12.7503579278214,13.2407563096607,13.7311546914999,14.2215530733392,
14.7119514551785,15.2023498370178,15.6927482188571,16.1831466006964,16.6735449825356,
17.1639433643749,17.6543417462142,18.1447401280535,18.6351385098928,19.1255368917321,
19.6159352735713,20.1063336554106,20.5967320372499,21.0871304190892,21.5775288009285,
22.0679271827678,22.558325564607,23.0487239464463,23.5391223282856,24.0295207101249,
24.5199190919642,25.0103174738035,25.5007158556428,25.991114237482,26.4815126193213,
26.9719110011606,27.4623093829999,27.9527077648392,28.4431061466785,28.9335045285177,
29.423902910357,29.9143012921963,30.4046996740356,30.8950980558749,31.3854964377142,
31.8758948195534,32.3662932013927,32.856691583232,33.3470899650713,33.8374883469106,
34.3278867287499,34.8182851105891,35.3086834924284,35.7990818742677,36.289480256107,
36.7798786379463,37.2702770197856,37.7606754016249,38.2510737834641,38.7414721653034,
39.2318705471427,39.722268928982,40.2126673108213,40.7030656926605,41.1934640744998,
41.6838624563391,42.1742608381784,42.6646592200177,43.155057601857,43.6454559836963,
44.1358543655355,44.6262527473748,45.1166511292141,45.6070495110534,46.0974478928927,
46.587846274732,47.0782446565712,47.2939563352912),.UNSPECIFIED.);
#1436=B_SPLINE_CURVE_WITH_KNOTS('',3,(#56011,#56012,#56013,#56014,#56015,
#56016,#56017,#56018),.UNSPECIFIED.,.F.,.F.,(4,2,2,4),(-0.655895828583228,
-0.493988108841948,-0.303390394118163,0.),.UNSPECIFIED.);
#1437=B_SPLINE_CURVE_WITH_KNOTS('',3,(#56019,#56020,#56021,#56022,#56023,
#56024,#56025,#56026,#56027,#56028,#56029,#56030,#56031,#56032,#56033,#56034,
#56035,#56036,#56037,#56038,#56039,#56040,#56041,#56042,#56043,#56044,#56045,
#56046,#56047,#56048,#56049,#56050,#56051,#56052,#56053,#56054,#56055,#56056,
#56057,#56058,#56059,#56060,#56061,#56062,#56063,#56064,#56065,#56066,#56067,
#56068,#56069,#56070,#56071,#56072,#56073,#56074,#56075,#56076,#56077,#56078,
#56079,#56080,#56081,#56082,#56083,#56084,#56085,#56086,#56087,#56088,#56089,
#56090,#56091,#56092,#56093,#56094,#56095,#56096,#56097,#56098,#56099,#56100,
#56101,#56102,#56103,#56104,#56105,#56106,#56107,#56108,#56109,#56110,#56111,
#56112,#56113,#56114,#56115,#56116,#56117,#56118),.UNSPECIFIED.,.F.,.F.,
(4,1,1,1,1,1,1,1,1,1,1,1,1,1,1,1,1,1,1,1,1,1,1,1,1,1,1,1,1,1,1,1,1,1,1,
1,1,1,1,1,1,1,1,1,1,1,1,1,1,1,1,1,1,1,1,1,1,1,1,1,1,1,1,1,1,1,1,1,1,1,1,
1,1,1,1,1,1,1,1,1,1,1,1,1,1,1,1,1,1,1,1,1,1,1,1,1,1,4),(7.04827039213812,
7.26398207085812,7.7543804526974,8.24477883453668,8.73517721637597,9.22557559821525,
9.71597398005454,10.2063723618938,10.6967707437331,11.1871691255724,11.6775675074117,
12.167965889251,12.6583642710902,13.1487626529295,13.6391610347688,14.1295594166081,
14.6199577984474,15.1103561802867,15.6007545621259,16.0911529439652,16.5815513258045,
17.0719497076438,17.5623480894831,18.0527464713224,18.5431448531616,19.0335432350009,
19.5239416168402,20.0143399986795,20.5047383805188,20.9951367623581,21.4855351441973,
21.9759335260366,22.4663319078759,22.9567302897152,23.4471286715545,23.9375270533938,
24.427925435233,24.9183238170723,25.4087221989116,25.8991205807509,26.3895189625902,
26.8799173444295,27.3703157262687,27.860714108108,28.3511124899473,28.8415108717866,
29.3319092536259,29.8223076354652,30.3127060173044,30.8031043991437,31.293502780983,
31.7839011628223,32.2742995446616,32.7646979265009,33.2550963083402,33.7454946901794,
34.2358930720187,34.726291453858,35.2166898356973,35.7070882175366,36.1974865993759,
36.6878849812151,37.1782833630544,37.6686817448937,38.159080126733,38.6494785085723,
39.1398768904116,39.6302752722508,40.1206736540901,40.6110720359294,41.1014704177687,
41.591868799608,42.0822671814473,42.5726655632865,43.0630639451258,43.5534623269651,
44.0438607088044,44.5342590906437,45.024657472483,45.5150558543222,46.0054542361615,
46.4958526180008,46.9862509998401,47.4766493816794,47.9670477635187,48.457446145358,
48.9478445271972,49.4382429090365,49.9286412908758,50.4190396727151,50.9094380545544,
51.3998364363937,51.8902348182329,52.3806332000722,52.8710315819115,53.3614299637508,
53.8518283455901,54.3422267274294),.UNSPECIFIED.);
#1438=B_SPLINE_CURVE_WITH_KNOTS('',3,(#56524,#56525,#56526,#56527,#56528,
#56529,#56530,#56531,#56532,#56533,#56534,#56535,#56536,#56537,#56538,#56539,
#56540,#56541,#56542,#56543,#56544,#56545,#56546,#56547,#56548,#56549,#56550,
#56551,#56552,#56553,#56554,#56555,#56556,#56557,#56558,#56559,#56560,#56561,
#56562,#56563,#56564,#56565,#56566,#56567,#56568,#56569,#56570,#56571,#56572,
#56573,#56574,#56575),.UNSPECIFIED.,.F.,.F.,(4,3,3,3,3,3,3,3,3,3,3,3,3,
3,3,3,3,4),(0.,0.113340575159286,0.226679014316618,0.308971226981702,0.331574139310527,
0.375660801919039,0.487626538864782,0.577647057862927,0.619647639303814,
0.642726778605582,0.752674952029806,0.769690750751167,0.865631662359539,
0.890410497302428,0.914699066250878,1.0235933762904,1.13055552817073,1.15345439718465),
 .UNSPECIFIED.);
#1439=B_SPLINE_CURVE_WITH_KNOTS('',3,(#56577,#56578,#56579,#56580,#56581,
#56582,#56583,#56584,#56585,#56586,#56587,#56588,#56589,#56590,#56591,#56592,
#56593,#56594,#56595,#56596,#56597,#56598,#56599,#56600,#56601,#56602,#56603,
#56604,#56605,#56606,#56607,#56608,#56609,#56610,#56611,#56612,#56613,#56614,
#56615,#56616,#56617,#56618,#56619,#56620,#56621,#56622,#56623,#56624,#56625),
 .UNSPECIFIED.,.F.,.F.,(4,3,3,3,3,3,3,3,3,3,3,3,3,3,3,3,4),(-1.15345439718468,
-1.04561219422299,-0.936713145930054,-0.898860433224846,-0.874966557590888,
-0.796527420497185,-0.69819122971956,-0.637686241518252,-0.608878950479122,
-0.496956393343038,-0.403182657386683,-0.351450861948057,-0.31601513468901,
-0.29336187161946,-0.180573976425843,-0.067406475320211,0.),
 .UNSPECIFIED.);
#1440=B_SPLINE_CURVE_WITH_KNOTS('',3,(#56626,#56627,#56628,#56629,#56630,
#56631,#56632,#56633,#56634,#56635,#56636,#56637,#56638,#56639,#56640,#56641,
#56642,#56643,#56644,#56645,#56646,#56647,#56648,#56649,#56650,#56651,#56652,
#56653,#56654,#56655,#56656,#56657,#56658,#56659,#56660,#56661,#56662,#56663,
#56664,#56665,#56666,#56667,#56668,#56669,#56670,#56671,#56672,#56673,#56674,
#56675,#56676,#56677,#56678,#56679,#56680,#56681,#56682,#56683,#56684,#56685,
#56686,#56687,#56688,#56689,#56690,#56691,#56692,#56693,#56694,#56695,#56696,
#56697,#56698,#56699,#56700,#56701,#56702,#56703,#56704,#56705,#56706,#56707,
#56708,#56709,#56710,#56711,#56712,#56713,#56714,#56715,#56716,#56717,#56718,
#56719,#56720,#56721,#56722,#56723,#56724),.UNSPECIFIED.,.F.,.F.,(4,1,1,
1,1,1,1,1,1,1,1,1,1,1,1,1,1,1,1,1,1,1,1,1,1,1,1,1,1,1,1,1,1,1,1,1,1,1,1,
1,1,1,1,1,1,1,1,1,1,1,1,1,1,1,1,1,1,1,1,1,1,1,1,1,1,1,1,1,1,1,1,1,1,1,1,
1,1,1,1,1,1,1,1,1,1,1,1,1,1,1,1,1,1,1,1,1,4),(8.50634549793093,8.54067951788559,
9.03814922646808,9.53561893505058,10.0330886436331,10.5305583522156,11.028028060798,
11.5254977693805,12.022967477963,12.5204371865455,13.017906895128,13.5153766037105,
14.012846312293,14.5103160208755,15.007785729458,15.5052554380405,16.002725146623,
16.5001948552054,16.9976645637879,17.4951342723704,17.9926039809529,18.4900736895354,
18.9875433981179,19.4850131067004,19.9824828152829,20.4799525238654,20.9774222324479,
21.4748919410303,21.9723616496128,22.4698313581953,22.9673010667778,23.4647707753603,
23.9622404839428,24.4597101925253,24.9571799011078,25.4546496096903,25.9521193182728,
26.4495890268552,26.9470587354377,27.4445284440202,27.9419981526027,28.4394678611852,
28.9369375697677,29.4344072783502,29.9318769869327,30.4293466955152,30.9268164040977,
31.4242861126801,31.9217558212626,32.4192255298451,32.9166952384276,33.4141649470101,
33.9116346555926,34.4091043641751,34.9065740727576,35.4040437813401,35.9015134899226,
36.3989831985051,36.8964529070875,37.39392261567,37.8913923242525,38.388862032835,
38.8863317414175,39.38380145,39.8812711585825,40.378740867165,40.8762105757475,
41.37368028433,41.8711499929124,42.3686197014949,42.8660894100774,43.3635591186599,
43.8610288272424,44.3584985358249,44.8559682444074,45.3534379529899,45.8509076615724,
46.3483773701549,46.8458470787373,47.3433167873198,47.8407864959023,48.3382562044848,
48.8357259130673,49.3331956216498,49.8306653302323,50.3281350388148,50.8256047473973,
51.3230744559798,51.8205441645622,52.3180138731447,52.8154835817272,53.3129532903097,
53.8104229988922,54.3078927074747,54.8053624160572,55.3028321246397,55.8003018332222),
 .UNSPECIFIED.);
#1441=B_SPLINE_CURVE_WITH_KNOTS('',3,(#57230,#57231,#57232,#57233,#57234,
#57235,#57236,#57237),.UNSPECIFIED.,.F.,.F.,(4,2,2,4),(0.,0.169060128143182,
0.25966506968926,0.35733520735872),.UNSPECIFIED.);
#1442=B_SPLINE_CURVE_WITH_KNOTS('',3,(#57239,#57240,#57241,#57242,#57243,
#57244,#57245,#57246),.UNSPECIFIED.,.F.,.F.,(4,2,2,4),(-0.357325312875914,
-0.25966481301295,-0.16906915003162,0.),.UNSPECIFIED.);
#1443=B_SPLINE_CURVE_WITH_KNOTS('',3,(#57247,#57248,#57249,#57250),
 .UNSPECIFIED.,.F.,.F.,(4,4),(9.27143058288951,9.42477796076936),
 .UNSPECIFIED.);
#1444=B_SPLINE_CURVE_WITH_KNOTS('',3,(#57256,#57257,#57258,#57259,#57260,
#57261,#57262,#57263),.UNSPECIFIED.,.F.,.F.,(4,2,2,4),(-0.415677006509057,
-0.30010857089105,-0.193253093542049,0.),.UNSPECIFIED.);
#1445=B_SPLINE_CURVE_WITH_KNOTS('',3,(#57265,#57266,#57267,#57268,#57269,
#57270,#57271,#57272,#57273,#57274,#57275,#57276,#57277,#57278,#57279,#57280,
#57281,#57282,#57283,#57284,#57285,#57286,#57287,#57288,#57289,#57290,#57291,
#57292,#57293,#57294,#57295,#57296,#57297,#57298,#57299,#57300,#57301,#57302,
#57303,#57304,#57305,#57306,#57307,#57308,#57309,#57310,#57311,#57312,#57313),
 .UNSPECIFIED.,.F.,.F.,(4,3,3,3,3,3,3,3,3,3,3,3,3,3,3,3,4),(-1.15166532125565,
-1.03829677946551,-0.92526093057982,-0.889798588874102,-0.85795025740414,
-0.776795567921361,-0.678445564828449,-0.620287810074995,-0.586753712344781,
-0.476556476810445,-0.383395555549714,-0.332702788626492,-0.305063279672108,
-0.282851348870515,-0.174044273873872,-0.0667784584837768,0.),
 .UNSPECIFIED.);
#1446=B_SPLINE_CURVE_WITH_KNOTS('',3,(#57314,#57315,#57316,#57317,#57318,
#57319),.UNSPECIFIED.,.F.,.F.,(4,2,4),(-0.659276662925401,-0.291453031942629,
0.),.UNSPECIFIED.);
#1447=B_SPLINE_CURVE_WITH_KNOTS('',3,(#57828,#57829,#57830,#57831,#57832,
#57833),.UNSPECIFIED.,.F.,.F.,(4,2,4),(0.,0.291454760594753,0.659275699695543),
 .UNSPECIFIED.);
#1448=B_SPLINE_CURVE_WITH_KNOTS('',3,(#57834,#57835,#57836,#57837,#57838,
#57839,#57840,#57841,#57842,#57843,#57844,#57845,#57846,#57847,#57848,#57849,
#57850,#57851,#57852,#57853,#57854,#57855,#57856,#57857,#57858,#57859,#57860,
#57861,#57862,#57863,#57864,#57865,#57866,#57867,#57868,#57869,#57870,#57871,
#57872,#57873,#57874,#57875,#57876,#57877,#57878,#57879,#57880,#57881,#57882,
#57883,#57884,#57885,#57886,#57887,#57888,#57889,#57890,#57891,#57892,#57893,
#57894,#57895,#57896,#57897,#57898,#57899,#57900,#57901,#57902,#57903,#57904,
#57905,#57906,#57907,#57908,#57909,#57910,#57911,#57912,#57913,#57914,#57915,
#57916,#57917,#57918,#57919,#57920,#57921,#57922,#57923,#57924,#57925,#57926,
#57927,#57928,#57929,#57930,#57931,#57932,#57933),.UNSPECIFIED.,.F.,.F.,
(4,1,1,1,1,1,1,1,1,1,1,1,1,1,1,1,1,1,1,1,1,1,1,1,1,1,1,1,1,1,1,1,1,1,1,
1,1,1,1,1,1,1,1,1,1,1,1,1,1,1,1,1,1,1,1,1,1,1,1,1,1,1,1,1,1,1,1,1,1,1,1,
1,1,1,1,1,1,1,1,1,1,1,1,1,1,1,1,1,1,1,1,1,1,1,1,1,1,4),(10.3432104236077,
10.5589221023277,11.049320484167,11.5397188660063,12.0301172478456,12.5205156296849,
13.0109140115242,13.5013123933634,13.9917107752027,14.482109157042,14.9725075388813,
15.4629059207206,15.9533043025599,16.4437026843991,16.9341010662384,17.4244994480777,
17.914897829917,18.4052962117563,18.8956945935956,19.3860929754348,19.8764913572741,
20.3668897391134,20.8572881209527,21.347686502792,21.8380848846313,22.3284832664706,
22.8188816483098,23.3092800301491,23.7996784119884,24.2900767938277,24.780475175667,
25.2708735575063,25.7612719393455,26.2516703211848,26.7420687030241,27.2324670848634,
27.7228654667027,28.213263848542,28.7036622303812,29.1940606122205,29.6844589940598,
30.1748573758991,30.6652557577384,31.1556541395777,31.6460525214169,32.1364509032562,
32.6268492850955,33.1172476669348,33.6076460487741,34.0980444306134,34.5884428124527,
35.0788411942919,35.5692395761312,36.0596379579705,36.5500363398098,37.0404347216491,
37.5308331034883,38.0212314853276,38.5116298671669,39.0020282490062,39.4924266308455,
39.9828250126848,40.4732233945241,40.9636217763633,41.4540201582026,41.9444185400419,
42.4348169218812,42.9252153037205,43.4156136855598,43.906012067399,44.3964104492383,
44.8868088310776,45.3772072129169,45.8676055947562,46.3580039765955,46.8484023584347,
47.338800740274,47.8291991221133,48.3195975039526,48.8099958857919,49.3003942676312,
49.7907926494704,50.2811910313097,50.771589413149,51.2619877949883,51.7523861768276,
52.2427845586669,52.7331829405062,53.2235813223454,53.7139797041847,54.204378086024,
54.6947764678633,55.1851748497026,55.6755732315419,56.1659716133811,56.6563699952204,
57.1467683770597,57.637166758899),.UNSPECIFIED.);
#1449=B_SPLINE_CURVE_WITH_KNOTS('',3,(#58339,#58340,#58341,#58342,#58343,
#58344,#58345,#58346,#58347,#58348,#58349,#58350,#58351,#58352,#58353,#58354,
#58355,#58356,#58357,#58358,#58359,#58360,#58361,#58362,#58363,#58364,#58365,
#58366,#58367,#58368,#58369,#58370,#58371,#58372,#58373,#58374,#58375,#58376,
#58377,#58378,#58379,#58380,#58381,#58382,#58383,#58384,#58385,#58386,#58387,
#58388,#58389,#58390),.UNSPECIFIED.,.F.,.F.,(4,3,3,3,3,3,3,3,3,3,3,3,3,
3,3,3,3,4),(0.,0.107536136059347,0.21639745378144,0.296736912823596,0.319843387979014,
0.356604402276687,0.466524670541788,0.54707448357054,0.595815754023213,
0.619047604474437,0.731049962221955,0.749314772119391,0.84990240940345,
0.873496420034821,0.898389588326068,1.01139267283444,1.12432918312036,1.15166532125563),
 .UNSPECIFIED.);
#1450=B_SPLINE_CURVE_WITH_KNOTS('',3,(#58391,#58392,#58393,#58394,#58395,
#58396,#58397,#58398,#58399,#58400,#58401,#58402,#58403,#58404,#58405,#58406,
#58407,#58408,#58409,#58410,#58411,#58412,#58413,#58414,#58415,#58416,#58417,
#58418,#58419,#58420,#58421,#58422,#58423,#58424,#58425,#58426,#58427,#58428,
#58429,#58430,#58431,#58432,#58433,#58434,#58435,#58436,#58437,#58438,#58439,
#58440,#58441,#58442,#58443,#58444,#58445,#58446,#58447,#58448,#58449,#58450,
#58451,#58452,#58453,#58454,#58455,#58456,#58457,#58458,#58459,#58460,#58461,
#58462,#58463,#58464,#58465,#58466,#58467,#58468,#58469,#58470,#58471,#58472,
#58473,#58474,#58475,#58476,#58477,#58478,#58479,#58480,#58481,#58482,#58483,
#58484,#58485,#58486,#58487,#58488,#58489),.UNSPECIFIED.,.F.,.F.,(4,1,1,
1,1,1,1,1,1,1,1,1,1,1,1,1,1,1,1,1,1,1,1,1,1,1,1,1,1,1,1,1,1,1,1,1,1,1,1,
1,1,1,1,1,1,1,1,1,1,1,1,1,1,1,1,1,1,1,1,1,1,1,1,1,1,1,1,1,1,1,1,1,1,1,1,
1,1,1,1,1,1,1,1,1,1,1,1,1,1,1,1,1,1,1,1,1,4),(11.8012855294006,11.8356195493552,
12.3330892579377,12.8305589665202,13.3280286751027,13.8254983836852,14.3229680922677,
14.8204378008502,15.3179075094327,15.8153772180151,16.3128469265976,16.8103166351801,
17.3077863437626,17.8052560523451,18.3027257609276,18.8001954695101,19.2976651780926,
19.7951348866751,20.2926045952576,20.79007430384,21.2875440124225,21.785013721005,
22.2824834295875,22.77995313817,23.2774228467525,23.774892555335,24.2723622639175,
24.7698319725,25.2673016810825,25.7647713896649,26.2622410982474,26.7597108068299,
27.2571805154124,27.7546502239949,28.2521199325774,28.7495896411599,29.2470593497424,
29.7445290583249,30.2419987669074,30.7394684754899,31.2369381840723,31.7344078926548,
32.2318776012373,32.7293473098198,33.2268170184023,33.7242867269848,34.2217564355673,
34.7192261441498,35.2166958527323,35.7141655613148,36.2116352698972,36.7091049784797,
37.2065746870622,37.7040443956447,38.2015141042272,38.6989838128097,39.1964535213922,
39.6939232299747,40.1913929385572,40.6888626471397,41.1863323557221,41.6838020643046,
42.1812717728871,42.6787414814696,43.1762111900521,43.6736808986346,44.1711506072171,
44.6686203157996,45.1660900243821,45.6635597329646,46.1610294415471,46.6584991501295,
47.155968858712,47.6534385672945,48.150908275877,48.6483779844595,49.145847693042,
49.6433174016245,50.140787110207,50.6382568187895,51.135726527372,51.6331962359544,
52.1306659445369,52.6281356531194,53.1256053617019,53.6230750702844,54.1205447788669,
54.6180144874494,55.1154841960319,55.6129539046144,56.1104236131969,56.6078933217793,
57.1053630303618,57.6028327389443,58.1003024475268,58.5977721561093,59.0952418646918),
 .UNSPECIFIED.);
#1451=B_SPLINE_CURVE_WITH_KNOTS('',3,(#58995,#58996,#58997,#58998,#58999,
#59000,#59001,#59002),.UNSPECIFIED.,.F.,.F.,(4,2,2,4),(0.,0.19323696658513,
0.300098749787172,0.415673620383952),.UNSPECIFIED.);
#1452=(
BOUNDED_CURVE()
B_SPLINE_CURVE(2,(#30883,#30884,#30885),.UNSPECIFIED.,.F.,.F.)
B_SPLINE_CURVE_WITH_KNOTS((3,3),(0.,0.113300250597084),.UNSPECIFIED.)
CURVE()
GEOMETRIC_REPRESENTATION_ITEM()
RATIONAL_B_SPLINE_CURVE((1.,1.00005131202982,1.))
REPRESENTATION_ITEM('')
);
#1453=(
BOUNDED_CURVE()
B_SPLINE_CURVE(2,(#30909,#30910,#30911),.UNSPECIFIED.,.F.,.F.)
B_SPLINE_CURVE_WITH_KNOTS((3,3),(0.,0.113300250597084),.UNSPECIFIED.)
CURVE()
GEOMETRIC_REPRESENTATION_ITEM()
RATIONAL_B_SPLINE_CURVE((1.,1.00005131202982,1.))
REPRESENTATION_ITEM('')
);
#1454=(
BOUNDED_CURVE()
B_SPLINE_CURVE(2,(#37008,#37009,#37010),.UNSPECIFIED.,.F.,.F.)
B_SPLINE_CURVE_WITH_KNOTS((3,3),(0.0827095041446621,0.74095125061019),
 .UNSPECIFIED.)
CURVE()
GEOMETRIC_REPRESENTATION_ITEM()
RATIONAL_B_SPLINE_CURVE((1.02109552796081,1.1000775419169,1.1000775419169))
REPRESENTATION_ITEM('')
);
#1455=(
BOUNDED_CURVE()
B_SPLINE_CURVE(2,(#37012,#37013,#37014),.UNSPECIFIED.,.F.,.F.)
B_SPLINE_CURVE_WITH_KNOTS((3,3),(0.0827095041446618,1.39919299707572),
 .UNSPECIFIED.)
CURVE()
GEOMETRIC_REPRESENTATION_ITEM()
RATIONAL_B_SPLINE_CURVE((1.02109552796081,1.17905955587299,1.02109552796081))
REPRESENTATION_ITEM('')
);
#1456=(
BOUNDED_CURVE()
B_SPLINE_CURVE(2,(#37016,#37017,#37018),.UNSPECIFIED.,.F.,.F.)
B_SPLINE_CURVE_WITH_KNOTS((3,3),(0.082709504144662,1.39919299707572),
 .UNSPECIFIED.)
CURVE()
GEOMETRIC_REPRESENTATION_ITEM()
RATIONAL_B_SPLINE_CURVE((1.02109552796081,1.17905955587299,1.02109552796081))
REPRESENTATION_ITEM('')
);
#1457=(
BOUNDED_CURVE()
B_SPLINE_CURVE(2,(#37020,#37021,#37022),.UNSPECIFIED.,.F.,.F.)
B_SPLINE_CURVE_WITH_KNOTS((3,3),(0.0827095041446621,1.39919299707572),
 .UNSPECIFIED.)
CURVE()
GEOMETRIC_REPRESENTATION_ITEM()
RATIONAL_B_SPLINE_CURVE((1.02109552796081,1.17905955587299,1.02109552796081))
REPRESENTATION_ITEM('')
);
#1458=(
BOUNDED_CURVE()
B_SPLINE_CURVE(2,(#37024,#37025,#37026),.UNSPECIFIED.,.F.,.F.)
B_SPLINE_CURVE_WITH_KNOTS((3,3),(0.0827095041446625,1.39919299707572),
 .UNSPECIFIED.)
CURVE()
GEOMETRIC_REPRESENTATION_ITEM()
RATIONAL_B_SPLINE_CURVE((1.02109552796081,1.17905955587299,1.02109552796081))
REPRESENTATION_ITEM('')
);
#1459=(
BOUNDED_CURVE()
B_SPLINE_CURVE(2,(#37028,#37029,#37030),.UNSPECIFIED.,.F.,.F.)
B_SPLINE_CURVE_WITH_KNOTS((3,3),(0.0827095041446619,1.39919299707572),
 .UNSPECIFIED.)
CURVE()
GEOMETRIC_REPRESENTATION_ITEM()
RATIONAL_B_SPLINE_CURVE((1.02109552796081,1.17905955587299,1.02109552796081))
REPRESENTATION_ITEM('')
);
#1460=(
BOUNDED_CURVE()
B_SPLINE_CURVE(2,(#37031,#37032,#37033),.UNSPECIFIED.,.F.,.F.)
B_SPLINE_CURVE_WITH_KNOTS((3,3),(0.74095125061019,1.39919299707572),
 .UNSPECIFIED.)
CURVE()
GEOMETRIC_REPRESENTATION_ITEM()
RATIONAL_B_SPLINE_CURVE((1.1000775419169,1.1000775419169,1.02109552796081))
REPRESENTATION_ITEM('')
);
#1461=(
BOUNDED_CURVE()
B_SPLINE_CURVE(2,(#37038,#37039,#37040),.UNSPECIFIED.,.F.,.F.)
B_SPLINE_CURVE_WITH_KNOTS((3,3),(0.0827095041446625,1.39919299707572),
 .UNSPECIFIED.)
CURVE()
GEOMETRIC_REPRESENTATION_ITEM()
RATIONAL_B_SPLINE_CURVE((1.02109552796081,1.17905955587299,1.02109552796081))
REPRESENTATION_ITEM('')
);
#1462=(
BOUNDED_CURVE()
B_SPLINE_CURVE(2,(#37045,#37046,#37047),.UNSPECIFIED.,.F.,.F.)
B_SPLINE_CURVE_WITH_KNOTS((3,3),(0.0827095041446616,1.39919299707572),
 .UNSPECIFIED.)
CURVE()
GEOMETRIC_REPRESENTATION_ITEM()
RATIONAL_B_SPLINE_CURVE((1.02109552796081,1.17905955587299,1.02109552796081))
REPRESENTATION_ITEM('')
);
#1463=(
BOUNDED_CURVE()
B_SPLINE_CURVE(2,(#37051,#37052,#37053),.UNSPECIFIED.,.F.,.F.)
B_SPLINE_CURVE_WITH_KNOTS((3,3),(0.082709504144662,1.39919299707572),
 .UNSPECIFIED.)
CURVE()
GEOMETRIC_REPRESENTATION_ITEM()
RATIONAL_B_SPLINE_CURVE((1.02109552796081,1.17905955587299,1.02109552796081))
REPRESENTATION_ITEM('')
);
#1464=(
BOUNDED_CURVE()
B_SPLINE_CURVE(2,(#37056,#37057,#37058),.UNSPECIFIED.,.F.,.F.)
B_SPLINE_CURVE_WITH_KNOTS((3,3),(0.0827095041446617,1.39919299707572),
 .UNSPECIFIED.)
CURVE()
GEOMETRIC_REPRESENTATION_ITEM()
RATIONAL_B_SPLINE_CURVE((1.02109552796081,1.17905955587299,1.02109552796081))
REPRESENTATION_ITEM('')
);
#1465=(
BOUNDED_CURVE()
B_SPLINE_CURVE(2,(#37060,#37061,#37062),.UNSPECIFIED.,.F.,.F.)
B_SPLINE_CURVE_WITH_KNOTS((3,3),(0.74095125061019,1.39919299707572),
 .UNSPECIFIED.)
CURVE()
GEOMETRIC_REPRESENTATION_ITEM()
RATIONAL_B_SPLINE_CURVE((1.1000775419169,1.1000775419169,1.02109552796081))
REPRESENTATION_ITEM('')
);
#1466=(
BOUNDED_CURVE()
B_SPLINE_CURVE(2,(#37067,#37068,#37069),.UNSPECIFIED.,.F.,.F.)
B_SPLINE_CURVE_WITH_KNOTS((3,3),(0.0827095041446617,0.74095125061019),
 .UNSPECIFIED.)
CURVE()
GEOMETRIC_REPRESENTATION_ITEM()
RATIONAL_B_SPLINE_CURVE((1.02109552796081,1.1000775419169,1.1000775419169))
REPRESENTATION_ITEM('')
);
#1467=(
BOUNDED_CURVE()
B_SPLINE_CURVE(2,(#37070,#37071,#37072),.UNSPECIFIED.,.F.,.F.)
B_SPLINE_CURVE_WITH_KNOTS((3,3),(0.0827095041446618,1.39919299707572),
 .UNSPECIFIED.)
CURVE()
GEOMETRIC_REPRESENTATION_ITEM()
RATIONAL_B_SPLINE_CURVE((1.02109552796081,1.17905955587299,1.02109552796081))
REPRESENTATION_ITEM('')
);
#1468=(
BOUNDED_CURVE()
B_SPLINE_CURVE(2,(#41740,#41741,#41742),.UNSPECIFIED.,.F.,.F.)
B_SPLINE_CURVE_WITH_KNOTS((3,3),(0.0820488586119731,0.652657405316371),
 .UNSPECIFIED.)
CURVE()
GEOMETRIC_REPRESENTATION_ITEM()
RATIONAL_B_SPLINE_CURVE((1.02442640079672,1.10366605866331,1.10366605866331))
REPRESENTATION_ITEM('')
);
#1469=(
BOUNDED_CURVE()
B_SPLINE_CURVE(2,(#41744,#41745,#41746),.UNSPECIFIED.,.F.,.F.)
B_SPLINE_CURVE_WITH_KNOTS((3,3),(0.0820488586119737,1.22326595202077),
 .UNSPECIFIED.)
CURVE()
GEOMETRIC_REPRESENTATION_ITEM()
RATIONAL_B_SPLINE_CURVE((1.02442640079672,1.18290571652989,1.02442640079672))
REPRESENTATION_ITEM('')
);
#1470=(
BOUNDED_CURVE()
B_SPLINE_CURVE(2,(#41748,#41749,#41750),.UNSPECIFIED.,.F.,.F.)
B_SPLINE_CURVE_WITH_KNOTS((3,3),(0.0820488586119732,1.22326595202077),
 .UNSPECIFIED.)
CURVE()
GEOMETRIC_REPRESENTATION_ITEM()
RATIONAL_B_SPLINE_CURVE((1.02442640079672,1.1829057165299,1.02442640079672))
REPRESENTATION_ITEM('')
);
#1471=(
BOUNDED_CURVE()
B_SPLINE_CURVE(2,(#41752,#41753,#41754),.UNSPECIFIED.,.F.,.F.)
B_SPLINE_CURVE_WITH_KNOTS((3,3),(0.082048858611974,1.22326595202077),
 .UNSPECIFIED.)
CURVE()
GEOMETRIC_REPRESENTATION_ITEM()
RATIONAL_B_SPLINE_CURVE((1.02442640079672,1.1829057165299,1.02442640079672))
REPRESENTATION_ITEM('')
);
#1472=(
BOUNDED_CURVE()
B_SPLINE_CURVE(2,(#41756,#41757,#41758),.UNSPECIFIED.,.F.,.F.)
B_SPLINE_CURVE_WITH_KNOTS((3,3),(0.0820488586119736,1.22326595202077),
 .UNSPECIFIED.)
CURVE()
GEOMETRIC_REPRESENTATION_ITEM()
RATIONAL_B_SPLINE_CURVE((1.02442640079672,1.1829057165299,1.02442640079672))
REPRESENTATION_ITEM('')
);
#1473=(
BOUNDED_CURVE()
B_SPLINE_CURVE(2,(#41760,#41761,#41762),.UNSPECIFIED.,.F.,.F.)
B_SPLINE_CURVE_WITH_KNOTS((3,3),(0.0820488586119736,1.22326595202077),
 .UNSPECIFIED.)
CURVE()
GEOMETRIC_REPRESENTATION_ITEM()
RATIONAL_B_SPLINE_CURVE((1.02442640079672,1.1829057165299,1.02442640079672))
REPRESENTATION_ITEM('')
);
#1474=(
BOUNDED_CURVE()
B_SPLINE_CURVE(2,(#41763,#41764,#41765),.UNSPECIFIED.,.F.,.F.)
B_SPLINE_CURVE_WITH_KNOTS((3,3),(0.652657405316371,1.22326595202077),
 .UNSPECIFIED.)
CURVE()
GEOMETRIC_REPRESENTATION_ITEM()
RATIONAL_B_SPLINE_CURVE((1.10366605866331,1.10366605866331,1.02442640079672))
REPRESENTATION_ITEM('')
);
#1475=(
BOUNDED_CURVE()
B_SPLINE_CURVE(2,(#41770,#41771,#41772),.UNSPECIFIED.,.F.,.F.)
B_SPLINE_CURVE_WITH_KNOTS((3,3),(0.0820488586119733,1.22326595202077),
 .UNSPECIFIED.)
CURVE()
GEOMETRIC_REPRESENTATION_ITEM()
RATIONAL_B_SPLINE_CURVE((1.02442640079672,1.1829057165299,1.02442640079672))
REPRESENTATION_ITEM('')
);
#1476=(
BOUNDED_CURVE()
B_SPLINE_CURVE(2,(#41777,#41778,#41779),.UNSPECIFIED.,.F.,.F.)
B_SPLINE_CURVE_WITH_KNOTS((3,3),(0.0820488586119739,1.22326595202077),
 .UNSPECIFIED.)
CURVE()
GEOMETRIC_REPRESENTATION_ITEM()
RATIONAL_B_SPLINE_CURVE((1.02442640079672,1.1829057165299,1.02442640079672))
REPRESENTATION_ITEM('')
);
#1477=(
BOUNDED_CURVE()
B_SPLINE_CURVE(2,(#41783,#41784,#41785),.UNSPECIFIED.,.F.,.F.)
B_SPLINE_CURVE_WITH_KNOTS((3,3),(0.0820488586119737,1.22326595202077),
 .UNSPECIFIED.)
CURVE()
GEOMETRIC_REPRESENTATION_ITEM()
RATIONAL_B_SPLINE_CURVE((1.02442640079672,1.1829057165299,1.02442640079672))
REPRESENTATION_ITEM('')
);
#1478=(
BOUNDED_CURVE()
B_SPLINE_CURVE(2,(#41788,#41789,#41790),.UNSPECIFIED.,.F.,.F.)
B_SPLINE_CURVE_WITH_KNOTS((3,3),(0.0820488586119733,1.22326595202077),
 .UNSPECIFIED.)
CURVE()
GEOMETRIC_REPRESENTATION_ITEM()
RATIONAL_B_SPLINE_CURVE((1.02442640079672,1.1829057165299,1.02442640079672))
REPRESENTATION_ITEM('')
);
#1479=(
BOUNDED_CURVE()
B_SPLINE_CURVE(2,(#41792,#41793,#41794),.UNSPECIFIED.,.F.,.F.)
B_SPLINE_CURVE_WITH_KNOTS((3,3),(0.652657405316372,1.22326595202077),
 .UNSPECIFIED.)
CURVE()
GEOMETRIC_REPRESENTATION_ITEM()
RATIONAL_B_SPLINE_CURVE((1.10366605866331,1.10366605866331,1.02442640079672))
REPRESENTATION_ITEM('')
);
#1480=(
BOUNDED_CURVE()
B_SPLINE_CURVE(2,(#41799,#41800,#41801),.UNSPECIFIED.,.F.,.F.)
B_SPLINE_CURVE_WITH_KNOTS((3,3),(0.0820488586119738,0.652657405316372),
 .UNSPECIFIED.)
CURVE()
GEOMETRIC_REPRESENTATION_ITEM()
RATIONAL_B_SPLINE_CURVE((1.02442640079672,1.10366605866331,1.10366605866331))
REPRESENTATION_ITEM('')
);
#1481=(
BOUNDED_CURVE()
B_SPLINE_CURVE(2,(#41802,#41803,#41804),.UNSPECIFIED.,.F.,.F.)
B_SPLINE_CURVE_WITH_KNOTS((3,3),(0.0820488586119739,1.22326595202077),
 .UNSPECIFIED.)
CURVE()
GEOMETRIC_REPRESENTATION_ITEM()
RATIONAL_B_SPLINE_CURVE((1.02442640079672,1.1829057165299,1.02442640079672))
REPRESENTATION_ITEM('')
);
#1482=(
BOUNDED_CURVE()
B_SPLINE_CURVE(2,(#42953,#42954,#42955),.UNSPECIFIED.,.F.,.F.)
B_SPLINE_CURVE_WITH_KNOTS((3,3),(0.,0.501003712116266),.UNSPECIFIED.)
CURVE()
GEOMETRIC_REPRESENTATION_ITEM()
RATIONAL_B_SPLINE_CURVE((1.,1.00062409811598,1.))
REPRESENTATION_ITEM('')
);
#1483=(
BOUNDED_CURVE()
B_SPLINE_CURVE(2,(#42958,#42959,#42960),.UNSPECIFIED.,.F.,.F.)
B_SPLINE_CURVE_WITH_KNOTS((3,3),(0.,0.501003712116271),.UNSPECIFIED.)
CURVE()
GEOMETRIC_REPRESENTATION_ITEM()
RATIONAL_B_SPLINE_CURVE((1.,1.00062409811548,1.))
REPRESENTATION_ITEM('')
);
#1484=(
BOUNDED_CURVE()
B_SPLINE_CURVE(2,(#42962,#42963,#42964),.UNSPECIFIED.,.F.,.F.)
B_SPLINE_CURVE_WITH_KNOTS((3,3),(0.,0.501003712116271),.UNSPECIFIED.)
CURVE()
GEOMETRIC_REPRESENTATION_ITEM()
RATIONAL_B_SPLINE_CURVE((1.,1.00062409811548,1.))
REPRESENTATION_ITEM('')
);
#1485=(
BOUNDED_CURVE()
B_SPLINE_CURVE(2,(#42967,#42968,#42969),.UNSPECIFIED.,.F.,.F.)
B_SPLINE_CURVE_WITH_KNOTS((3,3),(0.,0.501003712116266),.UNSPECIFIED.)
CURVE()
GEOMETRIC_REPRESENTATION_ITEM()
RATIONAL_B_SPLINE_CURVE((1.,1.00062409811598,1.))
REPRESENTATION_ITEM('')
);
#1486=(
BOUNDED_CURVE()
B_SPLINE_CURVE(2,(#42982,#42983,#42984),.UNSPECIFIED.,.F.,.F.)
B_SPLINE_CURVE_WITH_KNOTS((3,3),(0.,0.501003712116266),.UNSPECIFIED.)
CURVE()
GEOMETRIC_REPRESENTATION_ITEM()
RATIONAL_B_SPLINE_CURVE((1.,1.00062409811598,1.))
REPRESENTATION_ITEM('')
);
#1487=(
BOUNDED_CURVE()
B_SPLINE_CURVE(2,(#42987,#42988,#42989),.UNSPECIFIED.,.F.,.F.)
B_SPLINE_CURVE_WITH_KNOTS((3,3),(0.,0.501003712116271),.UNSPECIFIED.)
CURVE()
GEOMETRIC_REPRESENTATION_ITEM()
RATIONAL_B_SPLINE_CURVE((1.,1.00062409811541,1.))
REPRESENTATION_ITEM('')
);
#1488=(
BOUNDED_CURVE()
B_SPLINE_CURVE(2,(#42991,#42992,#42993),.UNSPECIFIED.,.F.,.F.)
B_SPLINE_CURVE_WITH_KNOTS((3,3),(0.,0.501003712116271),.UNSPECIFIED.)
CURVE()
GEOMETRIC_REPRESENTATION_ITEM()
RATIONAL_B_SPLINE_CURVE((1.,1.00062409811541,1.))
REPRESENTATION_ITEM('')
);
#1489=(
BOUNDED_CURVE()
B_SPLINE_CURVE(2,(#42996,#42997,#42998),.UNSPECIFIED.,.F.,.F.)
B_SPLINE_CURVE_WITH_KNOTS((3,3),(0.,0.501003712116266),.UNSPECIFIED.)
CURVE()
GEOMETRIC_REPRESENTATION_ITEM()
RATIONAL_B_SPLINE_CURVE((1.,1.00062409811598,1.))
REPRESENTATION_ITEM('')
);
#1490=(
BOUNDED_CURVE()
B_SPLINE_CURVE(2,(#43060,#43061,#43062),.UNSPECIFIED.,.F.,.F.)
B_SPLINE_CURVE_WITH_KNOTS((3,3),(0.,0.0102434961117393),.UNSPECIFIED.)
CURVE()
GEOMETRIC_REPRESENTATION_ITEM()
RATIONAL_B_SPLINE_CURVE((1.,1.01666622123361,1.03305467953702))
REPRESENTATION_ITEM('')
);
#1491=(
BOUNDED_CURVE()
B_SPLINE_CURVE(2,(#43064,#43065,#43066),.UNSPECIFIED.,.F.,.F.)
B_SPLINE_CURVE_WITH_KNOTS((3,3),(1.21900889027555,1.22925238638729),
 .UNSPECIFIED.)
CURVE()
GEOMETRIC_REPRESENTATION_ITEM()
RATIONAL_B_SPLINE_CURVE((1.03305467953703,1.01666622123362,1.))
REPRESENTATION_ITEM('')
);
#1492=(
BOUNDED_CURVE()
B_SPLINE_CURVE(2,(#43153,#43154,#43155),.UNSPECIFIED.,.F.,.F.)
B_SPLINE_CURVE_WITH_KNOTS((3,3),(0.,0.0102434961117392),.UNSPECIFIED.)
CURVE()
GEOMETRIC_REPRESENTATION_ITEM()
RATIONAL_B_SPLINE_CURVE((1.,1.01666622123361,1.03305467953702))
REPRESENTATION_ITEM('')
);
#1493=(
BOUNDED_CURVE()
B_SPLINE_CURVE(2,(#43157,#43158,#43159),.UNSPECIFIED.,.F.,.F.)
B_SPLINE_CURVE_WITH_KNOTS((3,3),(1.21900889027555,1.22925238638729),
 .UNSPECIFIED.)
CURVE()
GEOMETRIC_REPRESENTATION_ITEM()
RATIONAL_B_SPLINE_CURVE((1.03305467953701,1.01666622123361,1.))
REPRESENTATION_ITEM('')
);
#1494=(
BOUNDED_CURVE()
B_SPLINE_CURVE(2,(#59009,#59010,#59011),.UNSPECIFIED.,.F.,.F.)
B_SPLINE_CURVE_WITH_KNOTS((3,3),(0.0827095041446621,0.74095125061019),
 .UNSPECIFIED.)
CURVE()
GEOMETRIC_REPRESENTATION_ITEM()
RATIONAL_B_SPLINE_CURVE((1.02109552796081,1.1000775419169,1.1000775419169))
REPRESENTATION_ITEM('')
);
#1495=(
BOUNDED_CURVE()
B_SPLINE_CURVE(2,(#59013,#59014,#59015),.UNSPECIFIED.,.F.,.F.)
B_SPLINE_CURVE_WITH_KNOTS((3,3),(0.0827095041446618,1.39919299707572),
 .UNSPECIFIED.)
CURVE()
GEOMETRIC_REPRESENTATION_ITEM()
RATIONAL_B_SPLINE_CURVE((1.02109552796081,1.17905955587299,1.02109552796081))
REPRESENTATION_ITEM('')
);
#1496=(
BOUNDED_CURVE()
B_SPLINE_CURVE(2,(#59017,#59018,#59019),.UNSPECIFIED.,.F.,.F.)
B_SPLINE_CURVE_WITH_KNOTS((3,3),(0.082709504144662,1.39919299707572),
 .UNSPECIFIED.)
CURVE()
GEOMETRIC_REPRESENTATION_ITEM()
RATIONAL_B_SPLINE_CURVE((1.02109552796081,1.17905955587299,1.02109552796081))
REPRESENTATION_ITEM('')
);
#1497=(
BOUNDED_CURVE()
B_SPLINE_CURVE(2,(#59021,#59022,#59023),.UNSPECIFIED.,.F.,.F.)
B_SPLINE_CURVE_WITH_KNOTS((3,3),(0.0827095041446621,1.39919299707572),
 .UNSPECIFIED.)
CURVE()
GEOMETRIC_REPRESENTATION_ITEM()
RATIONAL_B_SPLINE_CURVE((1.02109552796081,1.17905955587299,1.02109552796081))
REPRESENTATION_ITEM('')
);
#1498=(
BOUNDED_CURVE()
B_SPLINE_CURVE(2,(#59025,#59026,#59027),.UNSPECIFIED.,.F.,.F.)
B_SPLINE_CURVE_WITH_KNOTS((3,3),(0.0827095041446625,1.39919299707572),
 .UNSPECIFIED.)
CURVE()
GEOMETRIC_REPRESENTATION_ITEM()
RATIONAL_B_SPLINE_CURVE((1.02109552796081,1.17905955587299,1.02109552796081))
REPRESENTATION_ITEM('')
);
#1499=(
BOUNDED_CURVE()
B_SPLINE_CURVE(2,(#59029,#59030,#59031),.UNSPECIFIED.,.F.,.F.)
B_SPLINE_CURVE_WITH_KNOTS((3,3),(0.0827095041446619,1.39919299707572),
 .UNSPECIFIED.)
CURVE()
GEOMETRIC_REPRESENTATION_ITEM()
RATIONAL_B_SPLINE_CURVE((1.02109552796081,1.17905955587299,1.02109552796081))
REPRESENTATION_ITEM('')
);
#1500=(
BOUNDED_CURVE()
B_SPLINE_CURVE(2,(#59032,#59033,#59034),.UNSPECIFIED.,.F.,.F.)
B_SPLINE_CURVE_WITH_KNOTS((3,3),(0.74095125061019,1.39919299707572),
 .UNSPECIFIED.)
CURVE()
GEOMETRIC_REPRESENTATION_ITEM()
RATIONAL_B_SPLINE_CURVE((1.1000775419169,1.1000775419169,1.02109552796081))
REPRESENTATION_ITEM('')
);
#1501=(
BOUNDED_CURVE()
B_SPLINE_CURVE(2,(#59039,#59040,#59041),.UNSPECIFIED.,.F.,.F.)
B_SPLINE_CURVE_WITH_KNOTS((3,3),(0.0827095041446625,1.39919299707572),
 .UNSPECIFIED.)
CURVE()
GEOMETRIC_REPRESENTATION_ITEM()
RATIONAL_B_SPLINE_CURVE((1.02109552796081,1.17905955587299,1.02109552796081))
REPRESENTATION_ITEM('')
);
#1502=(
BOUNDED_CURVE()
B_SPLINE_CURVE(2,(#59046,#59047,#59048),.UNSPECIFIED.,.F.,.F.)
B_SPLINE_CURVE_WITH_KNOTS((3,3),(0.0827095041446616,1.39919299707572),
 .UNSPECIFIED.)
CURVE()
GEOMETRIC_REPRESENTATION_ITEM()
RATIONAL_B_SPLINE_CURVE((1.02109552796081,1.17905955587299,1.02109552796081))
REPRESENTATION_ITEM('')
);
#1503=(
BOUNDED_CURVE()
B_SPLINE_CURVE(2,(#59052,#59053,#59054),.UNSPECIFIED.,.F.,.F.)
B_SPLINE_CURVE_WITH_KNOTS((3,3),(0.082709504144662,1.39919299707572),
 .UNSPECIFIED.)
CURVE()
GEOMETRIC_REPRESENTATION_ITEM()
RATIONAL_B_SPLINE_CURVE((1.02109552796081,1.17905955587299,1.02109552796081))
REPRESENTATION_ITEM('')
);
#1504=(
BOUNDED_CURVE()
B_SPLINE_CURVE(2,(#59057,#59058,#59059),.UNSPECIFIED.,.F.,.F.)
B_SPLINE_CURVE_WITH_KNOTS((3,3),(0.0827095041446617,1.39919299707572),
 .UNSPECIFIED.)
CURVE()
GEOMETRIC_REPRESENTATION_ITEM()
RATIONAL_B_SPLINE_CURVE((1.02109552796081,1.17905955587299,1.02109552796081))
REPRESENTATION_ITEM('')
);
#1505=(
BOUNDED_CURVE()
B_SPLINE_CURVE(2,(#59061,#59062,#59063),.UNSPECIFIED.,.F.,.F.)
B_SPLINE_CURVE_WITH_KNOTS((3,3),(0.74095125061019,1.39919299707572),
 .UNSPECIFIED.)
CURVE()
GEOMETRIC_REPRESENTATION_ITEM()
RATIONAL_B_SPLINE_CURVE((1.1000775419169,1.1000775419169,1.02109552796081))
REPRESENTATION_ITEM('')
);
#1506=(
BOUNDED_CURVE()
B_SPLINE_CURVE(2,(#59068,#59069,#59070),.UNSPECIFIED.,.F.,.F.)
B_SPLINE_CURVE_WITH_KNOTS((3,3),(0.0827095041446617,0.74095125061019),
 .UNSPECIFIED.)
CURVE()
GEOMETRIC_REPRESENTATION_ITEM()
RATIONAL_B_SPLINE_CURVE((1.02109552796081,1.1000775419169,1.1000775419169))
REPRESENTATION_ITEM('')
);
#1507=(
BOUNDED_CURVE()
B_SPLINE_CURVE(2,(#59071,#59072,#59073),.UNSPECIFIED.,.F.,.F.)
B_SPLINE_CURVE_WITH_KNOTS((3,3),(0.0827095041446618,1.39919299707572),
 .UNSPECIFIED.)
CURVE()
GEOMETRIC_REPRESENTATION_ITEM()
RATIONAL_B_SPLINE_CURVE((1.02109552796081,1.17905955587299,1.02109552796081))
REPRESENTATION_ITEM('')
);
#1508=SHAPE_REPRESENTATION_RELATIONSHIP('SRR','None',#59297,#1528);
#1509=SHAPE_REPRESENTATION_RELATIONSHIP('SRR','None',#59298,#1529);
#1510=SHAPE_REPRESENTATION_RELATIONSHIP('SRR','None',#59299,#1530);
#1511=SHAPE_REPRESENTATION_RELATIONSHIP('SRR','None',#59300,#1531);
#1512=SHAPE_REPRESENTATION_RELATIONSHIP('SRR','None',#59301,#1532);
#1513=SHAPE_REPRESENTATION_RELATIONSHIP('SRR','None',#59302,#1533);
#1514=SHAPE_REPRESENTATION_RELATIONSHIP('SRR','None',#59303,#1534);
#1515=SHAPE_REPRESENTATION_RELATIONSHIP('SRR','None',#59304,#1535);
#1516=SHAPE_REPRESENTATION_RELATIONSHIP('SRR','None',#59305,#1536);
#1517=SHAPE_REPRESENTATION_RELATIONSHIP('SRR','None',#59306,#1537);
#1518=SHAPE_REPRESENTATION_RELATIONSHIP('SRR','None',#59307,#1538);
#1519=SHAPE_REPRESENTATION_RELATIONSHIP('SRR','None',#59308,#1539);
#1520=SHAPE_REPRESENTATION_RELATIONSHIP('SRR','None',#59309,#1540);
#1521=SHAPE_REPRESENTATION_RELATIONSHIP('SRR','None',#59310,#1541);
#1522=SHAPE_REPRESENTATION_RELATIONSHIP('SRR','None',#59311,#1542);
#1523=SHAPE_REPRESENTATION_RELATIONSHIP('SRR','None',#59312,#1543);
#1524=SHAPE_REPRESENTATION_RELATIONSHIP('SRR','None',#59313,#1544);
#1525=SHAPE_REPRESENTATION_RELATIONSHIP('SRR','None',#59314,#1545);
#1526=SHAPE_REPRESENTATION_RELATIONSHIP('SRR','None',#59315,#1546);
#1527=SHAPE_REPRESENTATION_RELATIONSHIP('SRR','None',#59316,#1547);
#1528=ADVANCED_BREP_SHAPE_REPRESENTATION('',(#1575),#59184);
#1529=ADVANCED_BREP_SHAPE_REPRESENTATION('',(#1576),#59185);
#1530=ADVANCED_BREP_SHAPE_REPRESENTATION('',(#1577),#59186);
#1531=ADVANCED_BREP_SHAPE_REPRESENTATION('',(#1578),#59187);
#1532=ADVANCED_BREP_SHAPE_REPRESENTATION('',(#1579),#59188);
#1533=ADVANCED_BREP_SHAPE_REPRESENTATION('',(#1580),#59189);
#1534=ADVANCED_BREP_SHAPE_REPRESENTATION('',(#1581),#59190);
#1535=ADVANCED_BREP_SHAPE_REPRESENTATION('',(#1582),#59191);
#1536=ADVANCED_BREP_SHAPE_REPRESENTATION('',(#1583),#59192);
#1537=ADVANCED_BREP_SHAPE_REPRESENTATION('',(#1584),#59193);
#1538=ADVANCED_BREP_SHAPE_REPRESENTATION('',(#1585),#59194);
#1539=ADVANCED_BREP_SHAPE_REPRESENTATION('',(#1586),#59195);
#1540=ADVANCED_BREP_SHAPE_REPRESENTATION('',(#1587),#59196);
#1541=ADVANCED_BREP_SHAPE_REPRESENTATION('',(#1588),#59197);
#1542=ADVANCED_BREP_SHAPE_REPRESENTATION('',(#1589),#59198);
#1543=ADVANCED_BREP_SHAPE_REPRESENTATION('',(#1590),#59199);
#1544=ADVANCED_BREP_SHAPE_REPRESENTATION('',(#1591),#59200);
#1545=ADVANCED_BREP_SHAPE_REPRESENTATION('',(#1592),#59201);
#1546=ADVANCED_BREP_SHAPE_REPRESENTATION('',(#1593),#59202);
#1547=ADVANCED_BREP_SHAPE_REPRESENTATION('',(#1594),#59203);
#1548=STYLED_ITEM('',(#59579),#1575);
#1549=STYLED_ITEM('',(#59600),#1576);
#1550=STYLED_ITEM('',(#59572),#1577);
#1551=STYLED_ITEM('',(#59586),#1578);
#1552=STYLED_ITEM('',(#59586),#1579);
#1553=STYLED_ITEM('',(#59593),#1580);
#1554=STYLED_ITEM('',(#59572),#1581);
#1555=STYLED_ITEM('',(#59572),#1582);
#1556=STYLED_ITEM('',(#59586),#1583);
#1557=STYLED_ITEM('',(#59565),#1584);
#1558=STYLED_ITEM('',(#59565),#21883);
#1559=STYLED_ITEM('',(#59565),#21884);
#1560=STYLED_ITEM('',(#59565),#21885);
#1561=STYLED_ITEM('',(#59565),#21908);
#1562=STYLED_ITEM('',(#59565),#21911);
#1563=STYLED_ITEM('',(#59565),#21915);
#1564=STYLED_ITEM('',(#59565),#1585);
#1565=STYLED_ITEM('',(#59579),#1586);
#1566=STYLED_ITEM('',(#59586),#22320);
#1567=STYLED_ITEM('',(#59586),#1587);
#1568=STYLED_ITEM('',(#59579),#1588);
#1569=STYLED_ITEM('',(#59600),#1589);
#1570=STYLED_ITEM('',(#59586),#1590);
#1571=STYLED_ITEM('',(#59586),#1591);
#1572=STYLED_ITEM('',(#59600),#1592);
#1573=STYLED_ITEM('',(#59593),#1593);
#1574=STYLED_ITEM('',(#59572),#1594);
#1575=MANIFOLD_SOLID_BREP('Retainer plate',#22804);
#1576=MANIFOLD_SOLID_BREP('Ball guide',#22805);
#1577=MANIFOLD_SOLID_BREP('Swashplate',#22806);
#1578=MANIFOLD_SOLID_BREP('Spring',#22807);
#1579=MANIFOLD_SOLID_BREP('Key',#22808);
#1580=MANIFOLD_SOLID_BREP('Lip seal',#22809);
#1581=MANIFOLD_SOLID_BREP('Relief valve plug',#22810);
#1582=MANIFOLD_SOLID_BREP('Stud body',#22811);
#1583=MANIFOLD_SOLID_BREP('Drive shaft',#22812);
#1584=MANIFOLD_SOLID_BREP('Cylinder block',#22813);
#1585=MANIFOLD_SOLID_BREP('Front housing',#22814);
#1586=MANIFOLD_SOLID_BREP('Valve plate',#22815);
#1587=MANIFOLD_SOLID_BREP('Rear cover',#22816);
#1588=MANIFOLD_SOLID_BREP('Piston',#22817);
#1589=MANIFOLD_SOLID_BREP('Slipper',#22818);
#1590=MANIFOLD_SOLID_BREP('Cone assembly',#22819);
#1591=MANIFOLD_SOLID_BREP('Cup',#22820);
#1592=MANIFOLD_SOLID_BREP('Retaining ring',#22821);
#1593=MANIFOLD_SOLID_BREP('Socket head screw',#22822);
#1594=MANIFOLD_SOLID_BREP('Stud body',#22823);
#1595=SPHERICAL_SURFACE('',#23116,1.605);
#1596=SPHERICAL_SURFACE('',#23143,1.6);
#1597=SPHERICAL_SURFACE('',#24195,0.45);
#1598=SPHERICAL_SURFACE('',#24207,0.452);
#1599=FACE_BOUND('',#3977,.T.);
#1600=FACE_BOUND('',#3978,.T.);
#1601=FACE_BOUND('',#3979,.T.);
#1602=FACE_BOUND('',#3980,.T.);
#1603=FACE_BOUND('',#3981,.T.);
#1604=FACE_BOUND('',#3982,.T.);
#1605=FACE_BOUND('',#3983,.T.);
#1606=FACE_BOUND('',#3984,.T.);
#1607=FACE_BOUND('',#3985,.T.);
#1608=FACE_BOUND('',#3986,.T.);
#1609=FACE_BOUND('',#3989,.T.);
#1610=FACE_BOUND('',#3990,.T.);
#1611=FACE_BOUND('',#3991,.T.);
#1612=FACE_BOUND('',#3992,.T.);
#1613=FACE_BOUND('',#3993,.T.);
#1614=FACE_BOUND('',#3994,.T.);
#1615=FACE_BOUND('',#3995,.T.);
#1616=FACE_BOUND('',#3996,.T.);
#1617=FACE_BOUND('',#3997,.T.);
#1618=FACE_BOUND('',#3998,.T.);
#1619=FACE_BOUND('',#4029,.T.);
#1620=FACE_BOUND('',#4033,.T.);
#1621=FACE_BOUND('',#4038,.T.);
#1622=FACE_BOUND('',#4044,.T.);
#1623=FACE_BOUND('',#4051,.T.);
#1624=FACE_BOUND('',#4075,.T.);
#1625=FACE_BOUND('',#4077,.T.);
#1626=FACE_BOUND('',#4081,.T.);
#1627=FACE_BOUND('',#4084,.T.);
#1628=FACE_BOUND('',#4093,.T.);
#1629=FACE_BOUND('',#4244,.T.);
#1630=FACE_BOUND('',#4246,.T.);
#1631=FACE_BOUND('',#4252,.T.);
#1632=FACE_BOUND('',#4255,.T.);
#1633=FACE_BOUND('',#4260,.T.);
#1634=FACE_BOUND('',#4300,.T.);
#1635=FACE_BOUND('',#4303,.T.);
#1636=FACE_BOUND('',#4310,.T.);
#1637=FACE_BOUND('',#4313,.T.);
#1638=FACE_BOUND('',#4317,.T.);
#1639=FACE_BOUND('',#4332,.T.);
#1640=FACE_BOUND('',#4335,.T.);
#1641=FACE_BOUND('',#4337,.T.);
#1642=FACE_BOUND('',#4341,.T.);
#1643=FACE_BOUND('',#4344,.T.);
#1644=FACE_BOUND('',#4346,.T.);
#1645=FACE_BOUND('',#4348,.T.);
#1646=FACE_BOUND('',#4351,.T.);
#1647=FACE_BOUND('',#4356,.T.);
#1648=FACE_BOUND('',#4359,.T.);
#1649=FACE_BOUND('',#4365,.T.);
#1650=FACE_BOUND('',#4377,.T.);
#1651=FACE_BOUND('',#4380,.T.);
#1652=FACE_BOUND('',#4383,.T.);
#1653=FACE_BOUND('',#4386,.T.);
#1654=FACE_BOUND('',#4389,.T.);
#1655=FACE_BOUND('',#4392,.T.);
#1656=FACE_BOUND('',#4395,.T.);
#1657=FACE_BOUND('',#4398,.T.);
#1658=FACE_BOUND('',#4401,.T.);
#1659=FACE_BOUND('',#4403,.T.);
#1660=FACE_BOUND('',#4410,.T.);
#1661=FACE_BOUND('',#4411,.T.);
#1662=FACE_BOUND('',#4412,.T.);
#1663=FACE_BOUND('',#4413,.T.);
#1664=FACE_BOUND('',#4414,.T.);
#1665=FACE_BOUND('',#4415,.T.);
#1666=FACE_BOUND('',#4416,.T.);
#1667=FACE_BOUND('',#4417,.T.);
#1668=FACE_BOUND('',#4418,.T.);
#1669=FACE_BOUND('',#4419,.T.);
#1670=FACE_BOUND('',#4431,.T.);
#1671=FACE_BOUND('',#4435,.T.);
#1672=FACE_BOUND('',#4439,.T.);
#1673=FACE_BOUND('',#4443,.T.);
#1674=FACE_BOUND('',#4447,.T.);
#1675=FACE_BOUND('',#4451,.T.);
#1676=FACE_BOUND('',#4457,.T.);
#1677=FACE_BOUND('',#4465,.T.);
#1678=FACE_BOUND('',#4470,.T.);
#1679=FACE_BOUND('',#4471,.T.);
#1680=FACE_BOUND('',#4472,.T.);
#1681=FACE_BOUND('',#4473,.T.);
#1682=FACE_BOUND('',#4474,.T.);
#1683=FACE_BOUND('',#4475,.T.);
#1684=FACE_BOUND('',#4476,.T.);
#1685=FACE_BOUND('',#4478,.T.);
#1686=FACE_BOUND('',#4482,.T.);
#1687=FACE_BOUND('',#4483,.T.);
#1688=FACE_BOUND('',#4486,.T.);
#1689=FACE_BOUND('',#4494,.T.);
#1690=FACE_BOUND('',#4497,.T.);
#1691=FACE_BOUND('',#4500,.T.);
#1692=FACE_BOUND('',#4503,.T.);
#1693=FACE_BOUND('',#4506,.T.);
#1694=FACE_BOUND('',#4510,.T.);
#1695=FACE_BOUND('',#4511,.T.);
#1696=FACE_BOUND('',#4512,.T.);
#1697=FACE_BOUND('',#4513,.T.);
#1698=FACE_BOUND('',#4514,.T.);
#1699=FACE_BOUND('',#4515,.T.);
#1700=FACE_BOUND('',#4516,.T.);
#1701=FACE_BOUND('',#4517,.T.);
#1702=FACE_BOUND('',#4520,.T.);
#1703=FACE_BOUND('',#4521,.T.);
#1704=FACE_BOUND('',#4522,.T.);
#1705=FACE_BOUND('',#4523,.T.);
#1706=FACE_BOUND('',#4524,.T.);
#1707=FACE_BOUND('',#4525,.T.);
#1708=FACE_BOUND('',#4526,.T.);
#1709=FACE_BOUND('',#4527,.T.);
#1710=FACE_BOUND('',#4528,.T.);
#1711=FACE_BOUND('',#4548,.T.);
#1712=FACE_BOUND('',#4552,.T.);
#1713=FACE_BOUND('',#4556,.T.);
#1714=FACE_BOUND('',#4564,.T.);
#1715=FACE_BOUND('',#4568,.T.);
#1716=FACE_BOUND('',#4623,.T.);
#1717=FACE_BOUND('',#4645,.T.);
#1718=FACE_BOUND('',#4722,.T.);
#1719=FACE_BOUND('',#4833,.T.);
#1720=FACE_BOUND('',#4863,.T.);
#1721=FACE_BOUND('',#4886,.T.);
#1722=FACE_BOUND('',#4911,.T.);
#1723=FACE_BOUND('',#4915,.T.);
#1724=FACE_BOUND('',#4921,.T.);
#1725=FACE_BOUND('',#4922,.T.);
#1726=FACE_BOUND('',#4923,.T.);
#1727=FACE_BOUND('',#4924,.T.);
#1728=FACE_BOUND('',#4925,.T.);
#1729=FACE_BOUND('',#4926,.T.);
#1730=FACE_BOUND('',#4927,.T.);
#1731=FACE_BOUND('',#4928,.T.);
#1732=FACE_BOUND('',#4949,.T.);
#1733=FACE_BOUND('',#4950,.T.);
#1734=FACE_BOUND('',#4951,.T.);
#1735=FACE_BOUND('',#4952,.T.);
#1736=FACE_BOUND('',#4953,.T.);
#1737=FACE_BOUND('',#4954,.T.);
#1738=FACE_BOUND('',#4955,.T.);
#1739=FACE_BOUND('',#4956,.T.);
#1740=FACE_BOUND('',#4957,.T.);
#1741=FACE_BOUND('',#4958,.T.);
#1742=FACE_BOUND('',#4959,.T.);
#1743=FACE_BOUND('',#4960,.T.);
#1744=FACE_BOUND('',#4961,.T.);
#1745=FACE_BOUND('',#4962,.T.);
#1746=FACE_BOUND('',#4967,.T.);
#1747=FACE_BOUND('',#4969,.T.);
#1748=FACE_BOUND('',#4972,.T.);
#1749=FACE_BOUND('',#4975,.T.);
#1750=FACE_BOUND('',#4978,.T.);
#1751=FACE_BOUND('',#4986,.T.);
#1752=FACE_BOUND('',#4994,.T.);
#1753=FACE_BOUND('',#4996,.T.);
#1754=FACE_BOUND('',#5000,.T.);
#1755=FACE_BOUND('',#5003,.T.);
#1756=FACE_BOUND('',#5008,.T.);
#1757=FACE_BOUND('',#5012,.T.);
#1758=FACE_BOUND('',#5014,.T.);
#1759=FACE_BOUND('',#5015,.T.);
#1760=FACE_BOUND('',#5016,.T.);
#1761=FACE_BOUND('',#5017,.T.);
#1762=FACE_BOUND('',#5018,.T.);
#1763=FACE_BOUND('',#5019,.T.);
#1764=FACE_BOUND('',#5020,.T.);
#1765=FACE_BOUND('',#5021,.T.);
#1766=FACE_BOUND('',#5022,.T.);
#1767=FACE_BOUND('',#5023,.T.);
#1768=FACE_BOUND('',#5024,.T.);
#1769=FACE_BOUND('',#5025,.T.);
#1770=FACE_BOUND('',#5026,.T.);
#1771=FACE_BOUND('',#5027,.T.);
#1772=FACE_BOUND('',#5028,.T.);
#1773=FACE_BOUND('',#5029,.T.);
#1774=FACE_BOUND('',#5030,.T.);
#1775=FACE_BOUND('',#5032,.T.);
#1776=FACE_BOUND('',#5033,.T.);
#1777=FACE_BOUND('',#5034,.T.);
#1778=FACE_BOUND('',#5035,.T.);
#1779=FACE_BOUND('',#5036,.T.);
#1780=FACE_BOUND('',#5037,.T.);
#1781=FACE_BOUND('',#5038,.T.);
#1782=FACE_BOUND('',#5039,.T.);
#1783=FACE_BOUND('',#5040,.T.);
#1784=FACE_BOUND('',#5041,.T.);
#1785=FACE_BOUND('',#5042,.T.);
#1786=FACE_BOUND('',#5043,.T.);
#1787=FACE_BOUND('',#5044,.T.);
#1788=FACE_BOUND('',#5045,.T.);
#1789=FACE_BOUND('',#5046,.T.);
#1790=FACE_BOUND('',#5047,.T.);
#1791=FACE_BOUND('',#5048,.T.);
#1792=FACE_BOUND('',#5173,.T.);
#1793=FACE_BOUND('',#5177,.T.);
#1794=FACE_BOUND('',#5179,.T.);
#1795=FACE_BOUND('',#5182,.T.);
#1796=FACE_BOUND('',#5187,.T.);
#1797=FACE_BOUND('',#5192,.T.);
#1798=FACE_BOUND('',#5206,.T.);
#1799=FACE_BOUND('',#5207,.T.);
#1800=FACE_BOUND('',#5209,.T.);
#1801=FACE_BOUND('',#5210,.T.);
#1802=FACE_BOUND('',#5264,.T.);
#1803=FACE_BOUND('',#5273,.T.);
#1804=FACE_BOUND('',#5424,.T.);
#1805=FACE_BOUND('',#5471,.T.);
#1806=FACE_BOUND('',#5474,.T.);
#1807=FACE_BOUND('',#5481,.T.);
#1808=FACE_BOUND('',#5484,.T.);
#1809=FACE_BOUND('',#5488,.T.);
#1810=PLANE('',#23052);
#1811=PLANE('',#23065);
#1812=PLANE('',#23127);
#1813=PLANE('',#23133);
#1814=PLANE('',#23141);
#1815=PLANE('',#23146);
#1816=PLANE('',#23147);
#1817=PLANE('',#23148);
#1818=PLANE('',#23149);
#1819=PLANE('',#23158);
#1820=PLANE('',#23165);
#1821=PLANE('',#23167);
#1822=PLANE('',#23168);
#1823=PLANE('',#23171);
#1824=PLANE('',#23172);
#1825=PLANE('',#23175);
#1826=PLANE('',#23179);
#1827=PLANE('',#23185);
#1828=PLANE('',#23186);
#1829=PLANE('',#23189);
#1830=PLANE('',#23190);
#1831=PLANE('',#23198);
#1832=PLANE('',#23199);
#1833=PLANE('',#23208);
#1834=PLANE('',#23211);
#1835=PLANE('',#23227);
#1836=PLANE('',#23239);
#1837=PLANE('',#23244);
#1838=PLANE('',#23245);
#1839=PLANE('',#23246);
#1840=PLANE('',#23247);
#1841=PLANE('',#23248);
#1842=PLANE('',#23249);
#1843=PLANE('',#23250);
#1844=PLANE('',#23251);
#1845=PLANE('',#23252);
#1846=PLANE('',#23254);
#1847=PLANE('',#23255);
#1848=PLANE('',#23257);
#1849=PLANE('',#23258);
#1850=PLANE('',#23260);
#1851=PLANE('',#23261);
#1852=PLANE('',#23263);
#1853=PLANE('',#23264);
#1854=PLANE('',#23266);
#1855=PLANE('',#23267);
#1856=PLANE('',#23269);
#1857=PLANE('',#23270);
#1858=PLANE('',#23272);
#1859=PLANE('',#23273);
#1860=PLANE('',#23275);
#1861=PLANE('',#23276);
#1862=PLANE('',#23278);
#1863=PLANE('',#23279);
#1864=PLANE('',#23281);
#1865=PLANE('',#23282);
#1866=PLANE('',#23284);
#1867=PLANE('',#23285);
#1868=PLANE('',#23287);
#1869=PLANE('',#23288);
#1870=PLANE('',#23290);
#1871=PLANE('',#23291);
#1872=PLANE('',#23293);
#1873=PLANE('',#23295);
#1874=PLANE('',#23296);
#1875=PLANE('',#23297);
#1876=PLANE('',#23299);
#1877=PLANE('',#23300);
#1878=PLANE('',#23302);
#1879=PLANE('',#23303);
#1880=PLANE('',#23305);
#1881=PLANE('',#23306);
#1882=PLANE('',#23308);
#1883=PLANE('',#23309);
#1884=PLANE('',#23311);
#1885=PLANE('',#23312);
#1886=PLANE('',#23314);
#1887=PLANE('',#23315);
#1888=PLANE('',#23317);
#1889=PLANE('',#23318);
#1890=PLANE('',#23320);
#1891=PLANE('',#23321);
#1892=PLANE('',#23323);
#1893=PLANE('',#23324);
#1894=PLANE('',#23326);
#1895=PLANE('',#23327);
#1896=PLANE('',#23329);
#1897=PLANE('',#23330);
#1898=PLANE('',#23332);
#1899=PLANE('',#23333);
#1900=PLANE('',#23335);
#1901=PLANE('',#23336);
#1902=PLANE('',#23338);
#1903=PLANE('',#23339);
#1904=PLANE('',#23341);
#1905=PLANE('',#23342);
#1906=PLANE('',#23344);
#1907=PLANE('',#23345);
#1908=PLANE('',#23347);
#1909=PLANE('',#23348);
#1910=PLANE('',#23350);
#1911=PLANE('',#23351);
#1912=PLANE('',#23353);
#1913=PLANE('',#23354);
#1914=PLANE('',#23356);
#1915=PLANE('',#23357);
#1916=PLANE('',#23359);
#1917=PLANE('',#23360);
#1918=PLANE('',#23362);
#1919=PLANE('',#23363);
#1920=PLANE('',#23365);
#1921=PLANE('',#23366);
#1922=PLANE('',#23368);
#1923=PLANE('',#23369);
#1924=PLANE('',#23371);
#1925=PLANE('',#23372);
#1926=PLANE('',#23374);
#1927=PLANE('',#23375);
#1928=PLANE('',#23377);
#1929=PLANE('',#23378);
#1930=PLANE('',#23380);
#1931=PLANE('',#23381);
#1932=PLANE('',#23383);
#1933=PLANE('',#23384);
#1934=PLANE('',#23387);
#1935=PLANE('',#23388);
#1936=PLANE('',#23391);
#1937=PLANE('',#23392);
#1938=PLANE('',#23394);
#1939=PLANE('',#23395);
#1940=PLANE('',#23397);
#1941=PLANE('',#23398);
#1942=PLANE('',#23400);
#1943=PLANE('',#23401);
#1944=PLANE('',#23403);
#1945=PLANE('',#23404);
#1946=PLANE('',#23406);
#1947=PLANE('',#23407);
#1948=PLANE('',#23409);
#1949=PLANE('',#23410);
#1950=PLANE('',#23412);
#1951=PLANE('',#23413);
#1952=PLANE('',#23415);
#1953=PLANE('',#23416);
#1954=PLANE('',#23418);
#1955=PLANE('',#23419);
#1956=PLANE('',#23421);
#1957=PLANE('',#23422);
#1958=PLANE('',#23424);
#1959=PLANE('',#23425);
#1960=PLANE('',#23427);
#1961=PLANE('',#23428);
#1962=PLANE('',#23430);
#1963=PLANE('',#23431);
#1964=PLANE('',#23435);
#1965=PLANE('',#23436);
#1966=PLANE('',#23437);
#1967=PLANE('',#23440);
#1968=PLANE('',#23441);
#1969=PLANE('',#23443);
#1970=PLANE('',#23445);
#1971=PLANE('',#23446);
#1972=PLANE('',#23451);
#1973=PLANE('',#23454);
#1974=PLANE('',#23490);
#1975=PLANE('',#23515);
#1976=PLANE('',#23522);
#1977=PLANE('',#23529);
#1978=PLANE('',#23530);
#1979=PLANE('',#23531);
#1980=PLANE('',#23534);
#1981=PLANE('',#23535);
#1982=PLANE('',#23536);
#1983=PLANE('',#23538);
#1984=PLANE('',#23540);
#1985=PLANE('',#23542);
#1986=PLANE('',#23543);
#1987=PLANE('',#23548);
#1988=PLANE('',#23551);
#1989=PLANE('',#23556);
#1990=PLANE('',#23564);
#1991=PLANE('',#23567);
#1992=PLANE('',#23570);
#1993=PLANE('',#23571);
#1994=PLANE('',#23574);
#1995=PLANE('',#23577);
#1996=PLANE('',#23578);
#1997=PLANE('',#23584);
#1998=PLANE('',#23590);
#1999=PLANE('',#23594);
#2000=PLANE('',#23598);
#2001=PLANE('',#23602);
#2002=PLANE('',#23608);
#2003=PLANE('',#23610);
#2004=PLANE('',#23615);
#2005=PLANE('',#23619);
#2006=PLANE('',#23620);
#2007=PLANE('',#23621);
#2008=PLANE('',#23622);
#2009=PLANE('',#23656);
#2010=PLANE('',#23661);
#2011=PLANE('',#23666);
#2012=PLANE('',#23671);
#2013=PLANE('',#23676);
#2014=PLANE('',#23681);
#2015=PLANE('',#23686);
#2016=PLANE('',#23691);
#2017=PLANE('',#23696);
#2018=PLANE('',#23697);
#2019=PLANE('',#23717);
#2020=PLANE('',#23721);
#2021=PLANE('',#23722);
#2022=PLANE('',#23723);
#2023=PLANE('',#23724);
#2024=PLANE('',#23728);
#2025=PLANE('',#23732);
#2026=PLANE('',#23737);
#2027=PLANE('',#23745);
#2028=PLANE('',#23753);
#2029=PLANE('',#23761);
#2030=PLANE('',#23769);
#2031=PLANE('',#23777);
#2032=PLANE('',#23796);
#2033=PLANE('',#23813);
#2034=PLANE('',#23822);
#2035=PLANE('',#23832);
#2036=PLANE('',#23849);
#2037=PLANE('',#23853);
#2038=PLANE('',#23857);
#2039=PLANE('',#23861);
#2040=PLANE('',#23865);
#2041=PLANE('',#23872);
#2042=PLANE('',#23884);
#2043=PLANE('',#23932);
#2044=PLANE('',#23938);
#2045=PLANE('',#23945);
#2046=PLANE('',#23950);
#2047=PLANE('',#23965);
#2048=PLANE('',#23969);
#2049=PLANE('',#23977);
#2050=PLANE('',#23983);
#2051=PLANE('',#23997);
#2052=PLANE('',#23998);
#2053=PLANE('',#23999);
#2054=PLANE('',#24000);
#2055=PLANE('',#24001);
#2056=PLANE('',#24002);
#2057=PLANE('',#24003);
#2058=PLANE('',#24004);
#2059=PLANE('',#24005);
#2060=PLANE('',#24006);
#2061=PLANE('',#24007);
#2062=PLANE('',#24008);
#2063=PLANE('',#24009);
#2064=PLANE('',#24010);
#2065=PLANE('',#24011);
#2066=PLANE('',#24012);
#2067=PLANE('',#24013);
#2068=PLANE('',#24014);
#2069=PLANE('',#24015);
#2070=PLANE('',#24016);
#2071=PLANE('',#24017);
#2072=PLANE('',#24018);
#2073=PLANE('',#24019);
#2074=PLANE('',#24020);
#2075=PLANE('',#24021);
#2076=PLANE('',#24022);
#2077=PLANE('',#24023);
#2078=PLANE('',#24024);
#2079=PLANE('',#24025);
#2080=PLANE('',#24026);
#2081=PLANE('',#24027);
#2082=PLANE('',#24028);
#2083=PLANE('',#24029);
#2084=PLANE('',#24030);
#2085=PLANE('',#24031);
#2086=PLANE('',#24032);
#2087=PLANE('',#24033);
#2088=PLANE('',#24034);
#2089=PLANE('',#24035);
#2090=PLANE('',#24036);
#2091=PLANE('',#24037);
#2092=PLANE('',#24038);
#2093=PLANE('',#24039);
#2094=PLANE('',#24040);
#2095=PLANE('',#24041);
#2096=PLANE('',#24042);
#2097=PLANE('',#24043);
#2098=PLANE('',#24044);
#2099=PLANE('',#24045);
#2100=PLANE('',#24046);
#2101=PLANE('',#24047);
#2102=PLANE('',#24048);
#2103=PLANE('',#24049);
#2104=PLANE('',#24050);
#2105=PLANE('',#24051);
#2106=PLANE('',#24052);
#2107=PLANE('',#24053);
#2108=PLANE('',#24054);
#2109=PLANE('',#24055);
#2110=PLANE('',#24056);
#2111=PLANE('',#24057);
#2112=PLANE('',#24058);
#2113=PLANE('',#24059);
#2114=PLANE('',#24060);
#2115=PLANE('',#24061);
#2116=PLANE('',#24062);
#2117=PLANE('',#24063);
#2118=PLANE('',#24064);
#2119=PLANE('',#24065);
#2120=PLANE('',#24066);
#2121=PLANE('',#24067);
#2122=PLANE('',#24068);
#2123=PLANE('',#24069);
#2124=PLANE('',#24070);
#2125=PLANE('',#24071);
#2126=PLANE('',#24072);
#2127=PLANE('',#24073);
#2128=PLANE('',#24074);
#2129=PLANE('',#24075);
#2130=PLANE('',#24076);
#2131=PLANE('',#24077);
#2132=PLANE('',#24078);
#2133=PLANE('',#24079);
#2134=PLANE('',#24080);
#2135=PLANE('',#24081);
#2136=PLANE('',#24082);
#2137=PLANE('',#24083);
#2138=PLANE('',#24084);
#2139=PLANE('',#24085);
#2140=PLANE('',#24093);
#2141=PLANE('',#24098);
#2142=PLANE('',#24099);
#2143=PLANE('',#24111);
#2144=PLANE('',#24152);
#2145=PLANE('',#24154);
#2146=PLANE('',#24158);
#2147=PLANE('',#24160);
#2148=PLANE('',#24165);
#2149=PLANE('',#24169);
#2150=PLANE('',#24173);
#2151=PLANE('',#24187);
#2152=PLANE('',#24204);
#2153=PLANE('',#24205);
#2154=PLANE('',#24213);
#2155=PLANE('',#24217);
#2156=PLANE('',#24224);
#2157=PLANE('',#24230);
#2158=PLANE('',#24308);
#2159=PLANE('',#24310);
#2160=PLANE('',#24319);
#2161=PLANE('',#24320);
#2162=PLANE('',#24322);
#2163=PLANE('',#24331);
#2164=PLANE('',#24332);
#2165=PLANE('',#24334);
#2166=PLANE('',#24343);
#2167=PLANE('',#24344);
#2168=PLANE('',#24346);
#2169=PLANE('',#24355);
#2170=PLANE('',#24356);
#2171=PLANE('',#24358);
#2172=PLANE('',#24367);
#2173=PLANE('',#24368);
#2174=PLANE('',#24370);
#2175=PLANE('',#24379);
#2176=PLANE('',#24380);
#2177=PLANE('',#24382);
#2178=PLANE('',#24391);
#2179=PLANE('',#24392);
#2180=PLANE('',#24394);
#2181=PLANE('',#24403);
#2182=PLANE('',#24404);
#2183=PLANE('',#24406);
#2184=PLANE('',#24415);
#2185=PLANE('',#24416);
#2186=PLANE('',#24418);
#2187=PLANE('',#24427);
#2188=PLANE('',#24428);
#2189=PLANE('',#24430);
#2190=PLANE('',#24439);
#2191=PLANE('',#24440);
#2192=PLANE('',#24442);
#2193=PLANE('',#24451);
#2194=PLANE('',#24452);
#2195=PLANE('',#24454);
#2196=PLANE('',#24463);
#2197=PLANE('',#24464);
#2198=PLANE('',#24466);
#2199=PLANE('',#24475);
#2200=PLANE('',#24476);
#2201=PLANE('',#24478);
#2202=PLANE('',#24487);
#2203=PLANE('',#24488);
#2204=PLANE('',#24490);
#2205=PLANE('',#24499);
#2206=PLANE('',#24500);
#2207=PLANE('',#24502);
#2208=PLANE('',#24504);
#2209=PLANE('',#24512);
#2210=PLANE('',#24536);
#2211=PLANE('',#24540);
#2212=PLANE('',#24544);
#2213=PLANE('',#24548);
#2214=PLANE('',#24552);
#2215=PLANE('',#24556);
#2216=PLANE('',#24560);
#2217=PLANE('',#24564);
#2218=PLANE('',#24568);
#2219=PLANE('',#24572);
#2220=PLANE('',#24576);
#2221=PLANE('',#24580);
#2222=PLANE('',#24584);
#2223=PLANE('',#24588);
#2224=PLANE('',#24592);
#2225=PLANE('',#24599);
#2226=PLANE('',#24603);
#2227=PLANE('',#24609);
#2228=PLANE('',#24610);
#2229=PLANE('',#24614);
#2230=PLANE('',#24623);
#2231=PLANE('',#24631);
#2232=PLANE('',#24643);
#2233=PLANE('',#24647);
#2234=PLANE('',#24651);
#2235=PLANE('',#24655);
#2236=PLANE('',#24659);
#2237=PLANE('',#24660);
#2238=PLANE('',#24712);
#2239=PLANE('',#24714);
#2240=PLANE('',#24722);
#2241=PLANE('',#24726);
#2242=PLANE('',#24727);
#2243=PLANE('',#24728);
#2244=PLANE('',#24729);
#2245=PLANE('',#24730);
#2246=PLANE('',#24731);
#2247=PLANE('',#24732);
#2248=PLANE('',#24733);
#2249=PLANE('',#24734);
#2250=PLANE('',#24736);
#2251=PLANE('',#24737);
#2252=PLANE('',#24739);
#2253=PLANE('',#24740);
#2254=PLANE('',#24742);
#2255=PLANE('',#24743);
#2256=PLANE('',#24745);
#2257=PLANE('',#24746);
#2258=PLANE('',#24748);
#2259=PLANE('',#24749);
#2260=PLANE('',#24751);
#2261=PLANE('',#24752);
#2262=PLANE('',#24754);
#2263=PLANE('',#24755);
#2264=PLANE('',#24757);
#2265=PLANE('',#24758);
#2266=PLANE('',#24760);
#2267=PLANE('',#24761);
#2268=PLANE('',#24763);
#2269=PLANE('',#24764);
#2270=PLANE('',#24766);
#2271=PLANE('',#24767);
#2272=PLANE('',#24769);
#2273=PLANE('',#24770);
#2274=PLANE('',#24772);
#2275=PLANE('',#24773);
#2276=PLANE('',#24775);
#2277=PLANE('',#24776);
#2278=PLANE('',#24778);
#2279=PLANE('',#24779);
#2280=PLANE('',#24781);
#2281=PLANE('',#24782);
#2282=PLANE('',#24785);
#2283=PLANE('',#24786);
#2284=PLANE('',#24789);
#2285=PLANE('',#24790);
#2286=PLANE('',#24792);
#2287=PLANE('',#24793);
#2288=PLANE('',#24795);
#2289=PLANE('',#24796);
#2290=PLANE('',#24798);
#2291=PLANE('',#24799);
#2292=PLANE('',#24801);
#2293=PLANE('',#24802);
#2294=PLANE('',#24804);
#2295=PLANE('',#24805);
#2296=PLANE('',#24807);
#2297=PLANE('',#24808);
#2298=PLANE('',#24810);
#2299=PLANE('',#24811);
#2300=PLANE('',#24813);
#2301=PLANE('',#24814);
#2302=PLANE('',#24816);
#2303=PLANE('',#24817);
#2304=PLANE('',#24819);
#2305=PLANE('',#24820);
#2306=PLANE('',#24822);
#2307=PLANE('',#24823);
#2308=PLANE('',#24825);
#2309=PLANE('',#24826);
#2310=PLANE('',#24828);
#2311=PLANE('',#24829);
#2312=PLANE('',#24831);
#2313=PLANE('',#24832);
#2314=PLANE('',#24834);
#2315=PLANE('',#24835);
#2316=PLANE('',#24837);
#2317=PLANE('',#24838);
#2318=PLANE('',#24840);
#2319=PLANE('',#24841);
#2320=PLANE('',#24843);
#2321=PLANE('',#24844);
#2322=PLANE('',#24846);
#2323=PLANE('',#24847);
#2324=PLANE('',#24849);
#2325=PLANE('',#24850);
#2326=PLANE('',#24852);
#2327=PLANE('',#24853);
#2328=PLANE('',#24855);
#2329=PLANE('',#24856);
#2330=PLANE('',#24858);
#2331=PLANE('',#24859);
#2332=PLANE('',#24861);
#2333=PLANE('',#24862);
#2334=PLANE('',#24864);
#2335=PLANE('',#24865);
#2336=PLANE('',#24867);
#2337=PLANE('',#24868);
#2338=PLANE('',#24870);
#2339=PLANE('',#24871);
#2340=PLANE('',#24873);
#2341=PLANE('',#24874);
#2342=PLANE('',#24876);
#2343=PLANE('',#24877);
#2344=PLANE('',#24879);
#2345=PLANE('',#24880);
#2346=PLANE('',#24882);
#2347=PLANE('',#24883);
#2348=PLANE('',#24885);
#2349=PLANE('',#24886);
#2350=PLANE('',#24888);
#2351=PLANE('',#24889);
#2352=PLANE('',#24891);
#2353=PLANE('',#24893);
#2354=PLANE('',#24894);
#2355=PLANE('',#24895);
#2356=PLANE('',#24897);
#2357=PLANE('',#24898);
#2358=PLANE('',#24900);
#2359=PLANE('',#24901);
#2360=PLANE('',#24903);
#2361=PLANE('',#24904);
#2362=PLANE('',#24906);
#2363=PLANE('',#24907);
#2364=PLANE('',#24909);
#2365=PLANE('',#24910);
#2366=PLANE('',#24912);
#2367=PLANE('',#24913);
#2368=PLANE('',#24915);
#2369=PLANE('',#24916);
#2370=PLANE('',#24918);
#2371=PLANE('',#24919);
#2372=PLANE('',#24921);
#2373=PLANE('',#24922);
#2374=PLANE('',#24924);
#2375=PLANE('',#24925);
#2376=PLANE('',#24927);
#2377=PLANE('',#24928);
#2378=PLANE('',#24930);
#2379=PLANE('',#24931);
#2380=PLANE('',#24933);
#2381=PLANE('',#24934);
#2382=PLANE('',#24936);
#2383=PLANE('',#24937);
#2384=PLANE('',#24939);
#2385=PLANE('',#24940);
#2386=PLANE('',#24942);
#2387=PLANE('',#24943);
#2388=PLANE('',#24945);
#2389=PLANE('',#24946);
#2390=PLANE('',#24948);
#2391=PLANE('',#24949);
#2392=PLANE('',#24951);
#2393=PLANE('',#24995);
#2394=PLANE('',#25027);
#2395=PLANE('',#25034);
#2396=PLANE('',#25041);
#2397=PLANE('',#25042);
#2398=PLANE('',#25043);
#2399=PLANE('',#25046);
#2400=PLANE('',#25047);
#2401=PLANE('',#25048);
#2402=PLANE('',#25050);
#2403=PLANE('',#25052);
#2404=PLANE('',#25054);
#2405=PLANE('',#25055);
#2406=PLANE('',#25060);
#2407=PLANE('',#25063);
#2408=PLANE('',#25068);
#2409=CYLINDRICAL_SURFACE('',#23050,0.62);
#2410=CYLINDRICAL_SURFACE('',#23078,0.62);
#2411=CYLINDRICAL_SURFACE('',#23083,0.62);
#2412=CYLINDRICAL_SURFACE('',#23088,0.62);
#2413=CYLINDRICAL_SURFACE('',#23093,0.62);
#2414=CYLINDRICAL_SURFACE('',#23098,0.62);
#2415=CYLINDRICAL_SURFACE('',#23103,0.62);
#2416=CYLINDRICAL_SURFACE('',#23108,0.62);
#2417=CYLINDRICAL_SURFACE('',#23113,0.62);
#2418=CYLINDRICAL_SURFACE('',#23120,3.45);
#2419=CYLINDRICAL_SURFACE('',#23124,1.49);
#2420=CYLINDRICAL_SURFACE('',#23131,1.65);
#2421=CYLINDRICAL_SURFACE('',#23137,1.255);
#2422=CYLINDRICAL_SURFACE('',#23157,1.8);
#2423=CYLINDRICAL_SURFACE('',#23159,3.6);
#2424=CYLINDRICAL_SURFACE('',#23161,4.);
#2425=CYLINDRICAL_SURFACE('',#23183,0.4);
#2426=CYLINDRICAL_SURFACE('',#23187,0.4);
#2427=CYLINDRICAL_SURFACE('',#23192,1.9);
#2428=CYLINDRICAL_SURFACE('',#23195,1.7);
#2429=CYLINDRICAL_SURFACE('',#23205,2.);
#2430=CYLINDRICAL_SURFACE('',#23213,1.65);
#2431=CYLINDRICAL_SURFACE('',#23215,1.4);
#2432=CYLINDRICAL_SURFACE('',#23219,1.55);
#2433=CYLINDRICAL_SURFACE('',#23223,1.25);
#2434=CYLINDRICAL_SURFACE('',#23229,0.7475);
#2435=CYLINDRICAL_SURFACE('',#23231,0.7475);
#2436=CYLINDRICAL_SURFACE('',#23232,0.7475);
#2437=CYLINDRICAL_SURFACE('',#23233,0.7475);
#2438=CYLINDRICAL_SURFACE('',#23234,0.7475);
#2439=CYLINDRICAL_SURFACE('',#23235,0.7475);
#2440=CYLINDRICAL_SURFACE('',#23236,0.7475);
#2441=CYLINDRICAL_SURFACE('',#23237,0.7475);
#2442=CYLINDRICAL_SURFACE('',#23243,0.7475);
#2443=CYLINDRICAL_SURFACE('',#23447,0.3);
#2444=CYLINDRICAL_SURFACE('',#23456,0.7431);
#2445=CYLINDRICAL_SURFACE('',#23457,0.9);
#2446=CYLINDRICAL_SURFACE('',#23492,0.57225);
#2447=CYLINDRICAL_SURFACE('',#23494,0.57225);
#2448=CYLINDRICAL_SURFACE('',#23495,0.57225);
#2449=CYLINDRICAL_SURFACE('',#23496,0.57225);
#2450=CYLINDRICAL_SURFACE('',#23497,0.57225);
#2451=CYLINDRICAL_SURFACE('',#23499,0.6925);
#2452=CYLINDRICAL_SURFACE('',#23501,0.6925);
#2453=CYLINDRICAL_SURFACE('',#23502,0.6925);
#2454=CYLINDRICAL_SURFACE('',#23503,0.6925);
#2455=CYLINDRICAL_SURFACE('',#23504,0.6925);
#2456=CYLINDRICAL_SURFACE('',#23505,0.6925);
#2457=CYLINDRICAL_SURFACE('',#23506,0.6925);
#2458=CYLINDRICAL_SURFACE('',#23507,0.60685);
#2459=CYLINDRICAL_SURFACE('',#23509,0.60685);
#2460=CYLINDRICAL_SURFACE('',#23510,0.60685);
#2461=CYLINDRICAL_SURFACE('',#23511,0.60685);
#2462=CYLINDRICAL_SURFACE('',#23512,0.60685);
#2463=CYLINDRICAL_SURFACE('',#23513,0.60685);
#2464=CYLINDRICAL_SURFACE('',#23514,0.60685);
#2465=CYLINDRICAL_SURFACE('',#23518,0.60685);
#2466=CYLINDRICAL_SURFACE('',#23520,0.6925);
#2467=CYLINDRICAL_SURFACE('',#23526,0.57225);
#2468=CYLINDRICAL_SURFACE('',#23544,0.3);
#2469=CYLINDRICAL_SURFACE('',#23546,0.3);
#2470=CYLINDRICAL_SURFACE('',#23553,0.56785);
#2471=CYLINDRICAL_SURFACE('',#23565,0.3);
#2472=CYLINDRICAL_SURFACE('',#23568,0.3);
#2473=CYLINDRICAL_SURFACE('',#23572,0.4);
#2474=CYLINDRICAL_SURFACE('',#23575,0.4);
#2475=CYLINDRICAL_SURFACE('',#23582,1.1);
#2476=CYLINDRICAL_SURFACE('',#23588,1.25);
#2477=CYLINDRICAL_SURFACE('',#23592,1.195);
#2478=CYLINDRICAL_SURFACE('',#23596,1.25);
#2479=CYLINDRICAL_SURFACE('',#23600,1.195);
#2480=CYLINDRICAL_SURFACE('',#23604,1.25);
#2481=CYLINDRICAL_SURFACE('',#23613,3.6);
#2482=CYLINDRICAL_SURFACE('',#23617,3.7);
#2483=CYLINDRICAL_SURFACE('',#23625,0.35);
#2484=CYLINDRICAL_SURFACE('',#23628,0.35);
#2485=CYLINDRICAL_SURFACE('',#23631,0.35);
#2486=CYLINDRICAL_SURFACE('',#23634,0.35);
#2487=CYLINDRICAL_SURFACE('',#23637,0.35);
#2488=CYLINDRICAL_SURFACE('',#23640,0.35);
#2489=CYLINDRICAL_SURFACE('',#23643,0.35);
#2490=CYLINDRICAL_SURFACE('',#23646,0.35);
#2491=CYLINDRICAL_SURFACE('',#23649,0.35);
#2492=CYLINDRICAL_SURFACE('',#23652,0.601);
#2493=CYLINDRICAL_SURFACE('',#23657,0.601);
#2494=CYLINDRICAL_SURFACE('',#23662,0.601);
#2495=CYLINDRICAL_SURFACE('',#23667,0.601);
#2496=CYLINDRICAL_SURFACE('',#23672,0.601);
#2497=CYLINDRICAL_SURFACE('',#23677,0.601);
#2498=CYLINDRICAL_SURFACE('',#23682,0.601);
#2499=CYLINDRICAL_SURFACE('',#23687,0.601);
#2500=CYLINDRICAL_SURFACE('',#23692,0.601);
#2501=CYLINDRICAL_SURFACE('',#23709,1.7);
#2502=CYLINDRICAL_SURFACE('',#23713,3.7);
#2503=CYLINDRICAL_SURFACE('',#23719,1.252);
#2504=CYLINDRICAL_SURFACE('',#23725,2.56);
#2505=CYLINDRICAL_SURFACE('',#23729,2.84);
#2506=CYLINDRICAL_SURFACE('',#23739,0.45);
#2507=CYLINDRICAL_SURFACE('',#23747,0.45);
#2508=CYLINDRICAL_SURFACE('',#23755,0.45);
#2509=CYLINDRICAL_SURFACE('',#23763,0.45);
#2510=CYLINDRICAL_SURFACE('',#23771,0.45);
#2511=CYLINDRICAL_SURFACE('',#23779,0.45);
#2512=CYLINDRICAL_SURFACE('',#23781,0.7);
#2513=CYLINDRICAL_SURFACE('',#23793,0.7);
#2514=CYLINDRICAL_SURFACE('',#23805,0.7);
#2515=CYLINDRICAL_SURFACE('',#23806,0.7);
#2516=CYLINDRICAL_SURFACE('',#23807,0.7);
#2517=CYLINDRICAL_SURFACE('',#23808,0.7);
#2518=CYLINDRICAL_SURFACE('',#23812,0.66285);
#2519=CYLINDRICAL_SURFACE('',#23817,1.3);
#2520=CYLINDRICAL_SURFACE('',#23824,4.3);
#2521=CYLINDRICAL_SURFACE('',#23830,2.);
#2522=CYLINDRICAL_SURFACE('',#23838,5.);
#2523=CYLINDRICAL_SURFACE('',#23843,3.2);
#2524=CYLINDRICAL_SURFACE('',#23846,7.);
#2525=CYLINDRICAL_SURFACE('',#23851,4.005);
#2526=CYLINDRICAL_SURFACE('',#23855,2.2);
#2527=CYLINDRICAL_SURFACE('',#23859,2.6);
#2528=CYLINDRICAL_SURFACE('',#23863,2.4);
#2529=CYLINDRICAL_SURFACE('',#23870,0.45);
#2530=CYLINDRICAL_SURFACE('',#23903,0.45);
#2531=CYLINDRICAL_SURFACE('',#23908,0.45);
#2532=CYLINDRICAL_SURFACE('',#23913,0.45);
#2533=CYLINDRICAL_SURFACE('',#23918,0.45);
#2534=CYLINDRICAL_SURFACE('',#23923,0.45);
#2535=CYLINDRICAL_SURFACE('',#23926,0.3);
#2536=CYLINDRICAL_SURFACE('',#23930,0.8381);
#2537=CYLINDRICAL_SURFACE('',#23936,0.8381);
#2538=CYLINDRICAL_SURFACE('',#23939,0.6);
#2539=CYLINDRICAL_SURFACE('',#23942,0.6);
#2540=CYLINDRICAL_SURFACE('',#23947,2.25);
#2541=CYLINDRICAL_SURFACE('',#23955,7.);
#2542=CYLINDRICAL_SURFACE('',#23958,0.6);
#2543=CYLINDRICAL_SURFACE('',#23961,0.6);
#2544=CYLINDRICAL_SURFACE('',#23966,2.25);
#2545=CYLINDRICAL_SURFACE('',#23972,0.35);
#2546=CYLINDRICAL_SURFACE('',#23974,2.95);
#2547=CYLINDRICAL_SURFACE('',#23976,0.35);
#2548=CYLINDRICAL_SURFACE('',#23978,0.35);
#2549=CYLINDRICAL_SURFACE('',#23980,2.95);
#2550=CYLINDRICAL_SURFACE('',#23982,0.35);
#2551=CYLINDRICAL_SURFACE('',#23987,1.5);
#2552=CYLINDRICAL_SURFACE('',#23993,7.);
#2553=CYLINDRICAL_SURFACE('',#24086,0.3);
#2554=CYLINDRICAL_SURFACE('',#24091,0.8381);
#2555=CYLINDRICAL_SURFACE('',#24096,0.5);
#2556=CYLINDRICAL_SURFACE('',#24101,7.);
#2557=CYLINDRICAL_SURFACE('',#24119,0.404999999999999);
#2558=CYLINDRICAL_SURFACE('',#24123,0.404999999999999);
#2559=CYLINDRICAL_SURFACE('',#24127,0.405);
#2560=CYLINDRICAL_SURFACE('',#24131,0.404999999999999);
#2561=CYLINDRICAL_SURFACE('',#24135,0.405);
#2562=CYLINDRICAL_SURFACE('',#24139,0.404999999999999);
#2563=CYLINDRICAL_SURFACE('',#24150,2.6);
#2564=CYLINDRICAL_SURFACE('',#24156,2.4);
#2565=CYLINDRICAL_SURFACE('',#24163,0.575);
#2566=CYLINDRICAL_SURFACE('',#24167,0.6);
#2567=CYLINDRICAL_SURFACE('',#24171,0.575);
#2568=CYLINDRICAL_SURFACE('',#24175,0.6);
#2569=CYLINDRICAL_SURFACE('',#24177,0.3);
#2570=CYLINDRICAL_SURFACE('',#24183,0.6);
#2571=CYLINDRICAL_SURFACE('',#24189,0.25);
#2572=CYLINDRICAL_SURFACE('',#24193,0.075);
#2573=CYLINDRICAL_SURFACE('',#24198,0.59);
#2574=CYLINDRICAL_SURFACE('',#24201,0.65);
#2575=CYLINDRICAL_SURFACE('',#24211,0.075);
#2576=CYLINDRICAL_SURFACE('',#24215,0.4);
#2577=CYLINDRICAL_SURFACE('',#24220,0.8);
#2578=CYLINDRICAL_SURFACE('',#24226,0.55);
#2579=CYLINDRICAL_SURFACE('',#24607,1.9);
#2580=CYLINDRICAL_SURFACE('',#24612,1.6);
#2581=CYLINDRICAL_SURFACE('',#24618,1.25);
#2582=CYLINDRICAL_SURFACE('',#24627,2.6);
#2583=CYLINDRICAL_SURFACE('',#24637,0.1);
#2584=CYLINDRICAL_SURFACE('',#24640,0.1);
#2585=CYLINDRICAL_SURFACE('',#24644,0.328820889047374);
#2586=CYLINDRICAL_SURFACE('',#24648,1.195);
#2587=CYLINDRICAL_SURFACE('',#24652,0.328820889047374);
#2588=CYLINDRICAL_SURFACE('',#24656,1.53);
#2589=CYLINDRICAL_SURFACE('',#24662,0.3933);
#2590=CYLINDRICAL_SURFACE('',#24666,0.3933);
#2591=CYLINDRICAL_SURFACE('',#24667,0.3933);
#2592=CYLINDRICAL_SURFACE('',#24668,0.3933);
#2593=CYLINDRICAL_SURFACE('',#24669,0.3933);
#2594=CYLINDRICAL_SURFACE('',#24670,0.3933);
#2595=CYLINDRICAL_SURFACE('',#24671,0.3933);
#2596=CYLINDRICAL_SURFACE('',#24672,0.3933);
#2597=CYLINDRICAL_SURFACE('',#24673,0.3933);
#2598=CYLINDRICAL_SURFACE('',#24674,0.3933);
#2599=CYLINDRICAL_SURFACE('',#24675,0.3933);
#2600=CYLINDRICAL_SURFACE('',#24676,0.3933);
#2601=CYLINDRICAL_SURFACE('',#24677,0.3933);
#2602=CYLINDRICAL_SURFACE('',#24678,0.3933);
#2603=CYLINDRICAL_SURFACE('',#24679,0.3933);
#2604=CYLINDRICAL_SURFACE('',#24680,0.3933);
#2605=CYLINDRICAL_SURFACE('',#24681,0.3933);
#2606=CYLINDRICAL_SURFACE('',#24682,0.3933);
#2607=CYLINDRICAL_SURFACE('',#24683,0.3933);
#2608=CYLINDRICAL_SURFACE('',#24684,0.3933);
#2609=CYLINDRICAL_SURFACE('',#24685,0.3933);
#2610=CYLINDRICAL_SURFACE('',#24686,0.3933);
#2611=CYLINDRICAL_SURFACE('',#24687,0.3933);
#2612=CYLINDRICAL_SURFACE('',#24689,0.322275);
#2613=CYLINDRICAL_SURFACE('',#24691,0.322275);
#2614=CYLINDRICAL_SURFACE('',#24692,0.322275);
#2615=CYLINDRICAL_SURFACE('',#24693,0.322275);
#2616=CYLINDRICAL_SURFACE('',#24694,0.322275);
#2617=CYLINDRICAL_SURFACE('',#24695,0.322275);
#2618=CYLINDRICAL_SURFACE('',#24696,0.322275);
#2619=CYLINDRICAL_SURFACE('',#24697,0.322275);
#2620=CYLINDRICAL_SURFACE('',#24698,0.322275);
#2621=CYLINDRICAL_SURFACE('',#24699,0.322275);
#2622=CYLINDRICAL_SURFACE('',#24700,0.322275);
#2623=CYLINDRICAL_SURFACE('',#24701,0.322275);
#2624=CYLINDRICAL_SURFACE('',#24702,0.322275);
#2625=CYLINDRICAL_SURFACE('',#24703,0.322275);
#2626=CYLINDRICAL_SURFACE('',#24704,0.322275);
#2627=CYLINDRICAL_SURFACE('',#24705,0.322275);
#2628=CYLINDRICAL_SURFACE('',#24706,0.322275);
#2629=CYLINDRICAL_SURFACE('',#24707,0.322275);
#2630=CYLINDRICAL_SURFACE('',#24708,0.322275);
#2631=CYLINDRICAL_SURFACE('',#24709,0.322275);
#2632=CYLINDRICAL_SURFACE('',#24710,0.322275);
#2633=CYLINDRICAL_SURFACE('',#24711,0.322275);
#2634=CYLINDRICAL_SURFACE('',#24716,0.322275);
#2635=CYLINDRICAL_SURFACE('',#24717,0.3933);
#2636=CYLINDRICAL_SURFACE('',#24956,0.65);
#2637=CYLINDRICAL_SURFACE('',#24997,0.7475);
#2638=CYLINDRICAL_SURFACE('',#24999,0.7475);
#2639=CYLINDRICAL_SURFACE('',#25000,0.7475);
#2640=CYLINDRICAL_SURFACE('',#25001,0.7475);
#2641=CYLINDRICAL_SURFACE('',#25002,0.7475);
#2642=CYLINDRICAL_SURFACE('',#25003,0.7475);
#2643=CYLINDRICAL_SURFACE('',#25004,0.7475);
#2644=CYLINDRICAL_SURFACE('',#25005,0.7475);
#2645=CYLINDRICAL_SURFACE('',#25007,0.7925);
#2646=CYLINDRICAL_SURFACE('',#25009,0.7925);
#2647=CYLINDRICAL_SURFACE('',#25010,0.7925);
#2648=CYLINDRICAL_SURFACE('',#25011,0.7925);
#2649=CYLINDRICAL_SURFACE('',#25012,0.7925);
#2650=CYLINDRICAL_SURFACE('',#25013,0.7925);
#2651=CYLINDRICAL_SURFACE('',#25014,0.7925);
#2652=CYLINDRICAL_SURFACE('',#25015,0.7925);
#2653=CYLINDRICAL_SURFACE('',#25016,0.7925);
#2654=CYLINDRICAL_SURFACE('',#25017,0.70685);
#2655=CYLINDRICAL_SURFACE('',#25019,0.70685);
#2656=CYLINDRICAL_SURFACE('',#25020,0.70685);
#2657=CYLINDRICAL_SURFACE('',#25021,0.70685);
#2658=CYLINDRICAL_SURFACE('',#25022,0.70685);
#2659=CYLINDRICAL_SURFACE('',#25023,0.70685);
#2660=CYLINDRICAL_SURFACE('',#25024,0.70685);
#2661=CYLINDRICAL_SURFACE('',#25025,0.70685);
#2662=CYLINDRICAL_SURFACE('',#25026,0.70685);
#2663=CYLINDRICAL_SURFACE('',#25030,0.70685);
#2664=CYLINDRICAL_SURFACE('',#25032,0.7925);
#2665=CYLINDRICAL_SURFACE('',#25038,0.7475);
#2666=CYLINDRICAL_SURFACE('',#25056,0.4);
#2667=CYLINDRICAL_SURFACE('',#25058,0.4);
#2668=CYLINDRICAL_SURFACE('',#25065,0.7431);
#2669=FACE_OUTER_BOUND('',#3974,.T.);
#2670=FACE_OUTER_BOUND('',#3975,.T.);
#2671=FACE_OUTER_BOUND('',#3976,.T.);
#2672=FACE_OUTER_BOUND('',#3987,.T.);
#2673=FACE_OUTER_BOUND('',#3988,.T.);
#2674=FACE_OUTER_BOUND('',#3999,.T.);
#2675=FACE_OUTER_BOUND('',#4000,.T.);
#2676=FACE_OUTER_BOUND('',#4001,.T.);
#2677=FACE_OUTER_BOUND('',#4002,.T.);
#2678=FACE_OUTER_BOUND('',#4003,.T.);
#2679=FACE_OUTER_BOUND('',#4004,.T.);
#2680=FACE_OUTER_BOUND('',#4005,.T.);
#2681=FACE_OUTER_BOUND('',#4006,.T.);
#2682=FACE_OUTER_BOUND('',#4007,.T.);
#2683=FACE_OUTER_BOUND('',#4008,.T.);
#2684=FACE_OUTER_BOUND('',#4009,.T.);
#2685=FACE_OUTER_BOUND('',#4010,.T.);
#2686=FACE_OUTER_BOUND('',#4011,.T.);
#2687=FACE_OUTER_BOUND('',#4012,.T.);
#2688=FACE_OUTER_BOUND('',#4013,.T.);
#2689=FACE_OUTER_BOUND('',#4014,.T.);
#2690=FACE_OUTER_BOUND('',#4015,.T.);
#2691=FACE_OUTER_BOUND('',#4016,.T.);
#2692=FACE_OUTER_BOUND('',#4017,.T.);
#2693=FACE_OUTER_BOUND('',#4018,.T.);
#2694=FACE_OUTER_BOUND('',#4019,.T.);
#2695=FACE_OUTER_BOUND('',#4020,.T.);
#2696=FACE_OUTER_BOUND('',#4021,.T.);
#2697=FACE_OUTER_BOUND('',#4022,.T.);
#2698=FACE_OUTER_BOUND('',#4023,.T.);
#2699=FACE_OUTER_BOUND('',#4024,.T.);
#2700=FACE_OUTER_BOUND('',#4025,.T.);
#2701=FACE_OUTER_BOUND('',#4026,.T.);
#2702=FACE_OUTER_BOUND('',#4027,.T.);
#2703=FACE_OUTER_BOUND('',#4028,.T.);
#2704=FACE_OUTER_BOUND('',#4030,.T.);
#2705=FACE_OUTER_BOUND('',#4031,.T.);
#2706=FACE_OUTER_BOUND('',#4032,.T.);
#2707=FACE_OUTER_BOUND('',#4034,.T.);
#2708=FACE_OUTER_BOUND('',#4035,.T.);
#2709=FACE_OUTER_BOUND('',#4036,.T.);
#2710=FACE_OUTER_BOUND('',#4037,.T.);
#2711=FACE_OUTER_BOUND('',#4039,.T.);
#2712=FACE_OUTER_BOUND('',#4040,.T.);
#2713=FACE_OUTER_BOUND('',#4041,.T.);
#2714=FACE_OUTER_BOUND('',#4042,.T.);
#2715=FACE_OUTER_BOUND('',#4043,.T.);
#2716=FACE_OUTER_BOUND('',#4045,.T.);
#2717=FACE_OUTER_BOUND('',#4046,.T.);
#2718=FACE_OUTER_BOUND('',#4047,.T.);
#2719=FACE_OUTER_BOUND('',#4048,.T.);
#2720=FACE_OUTER_BOUND('',#4049,.T.);
#2721=FACE_OUTER_BOUND('',#4050,.T.);
#2722=FACE_OUTER_BOUND('',#4052,.T.);
#2723=FACE_OUTER_BOUND('',#4053,.T.);
#2724=FACE_OUTER_BOUND('',#4054,.T.);
#2725=FACE_OUTER_BOUND('',#4055,.T.);
#2726=FACE_OUTER_BOUND('',#4056,.T.);
#2727=FACE_OUTER_BOUND('',#4057,.T.);
#2728=FACE_OUTER_BOUND('',#4058,.T.);
#2729=FACE_OUTER_BOUND('',#4059,.T.);
#2730=FACE_OUTER_BOUND('',#4060,.T.);
#2731=FACE_OUTER_BOUND('',#4061,.T.);
#2732=FACE_OUTER_BOUND('',#4062,.T.);
#2733=FACE_OUTER_BOUND('',#4063,.T.);
#2734=FACE_OUTER_BOUND('',#4064,.T.);
#2735=FACE_OUTER_BOUND('',#4065,.T.);
#2736=FACE_OUTER_BOUND('',#4066,.T.);
#2737=FACE_OUTER_BOUND('',#4067,.T.);
#2738=FACE_OUTER_BOUND('',#4068,.T.);
#2739=FACE_OUTER_BOUND('',#4069,.T.);
#2740=FACE_OUTER_BOUND('',#4070,.T.);
#2741=FACE_OUTER_BOUND('',#4071,.T.);
#2742=FACE_OUTER_BOUND('',#4072,.T.);
#2743=FACE_OUTER_BOUND('',#4073,.T.);
#2744=FACE_OUTER_BOUND('',#4074,.T.);
#2745=FACE_OUTER_BOUND('',#4076,.T.);
#2746=FACE_OUTER_BOUND('',#4078,.T.);
#2747=FACE_OUTER_BOUND('',#4079,.T.);
#2748=FACE_OUTER_BOUND('',#4080,.T.);
#2749=FACE_OUTER_BOUND('',#4082,.T.);
#2750=FACE_OUTER_BOUND('',#4083,.T.);
#2751=FACE_OUTER_BOUND('',#4085,.T.);
#2752=FACE_OUTER_BOUND('',#4086,.T.);
#2753=FACE_OUTER_BOUND('',#4087,.T.);
#2754=FACE_OUTER_BOUND('',#4088,.T.);
#2755=FACE_OUTER_BOUND('',#4089,.T.);
#2756=FACE_OUTER_BOUND('',#4090,.T.);
#2757=FACE_OUTER_BOUND('',#4091,.T.);
#2758=FACE_OUTER_BOUND('',#4092,.T.);
#2759=FACE_OUTER_BOUND('',#4094,.T.);
#2760=FACE_OUTER_BOUND('',#4095,.T.);
#2761=FACE_OUTER_BOUND('',#4096,.T.);
#2762=FACE_OUTER_BOUND('',#4097,.T.);
#2763=FACE_OUTER_BOUND('',#4098,.T.);
#2764=FACE_OUTER_BOUND('',#4099,.T.);
#2765=FACE_OUTER_BOUND('',#4100,.T.);
#2766=FACE_OUTER_BOUND('',#4101,.T.);
#2767=FACE_OUTER_BOUND('',#4102,.T.);
#2768=FACE_OUTER_BOUND('',#4103,.T.);
#2769=FACE_OUTER_BOUND('',#4104,.T.);
#2770=FACE_OUTER_BOUND('',#4105,.T.);
#2771=FACE_OUTER_BOUND('',#4106,.T.);
#2772=FACE_OUTER_BOUND('',#4107,.T.);
#2773=FACE_OUTER_BOUND('',#4108,.T.);
#2774=FACE_OUTER_BOUND('',#4109,.T.);
#2775=FACE_OUTER_BOUND('',#4110,.T.);
#2776=FACE_OUTER_BOUND('',#4111,.T.);
#2777=FACE_OUTER_BOUND('',#4112,.T.);
#2778=FACE_OUTER_BOUND('',#4113,.T.);
#2779=FACE_OUTER_BOUND('',#4114,.T.);
#2780=FACE_OUTER_BOUND('',#4115,.T.);
#2781=FACE_OUTER_BOUND('',#4116,.T.);
#2782=FACE_OUTER_BOUND('',#4117,.T.);
#2783=FACE_OUTER_BOUND('',#4118,.T.);
#2784=FACE_OUTER_BOUND('',#4119,.T.);
#2785=FACE_OUTER_BOUND('',#4120,.T.);
#2786=FACE_OUTER_BOUND('',#4121,.T.);
#2787=FACE_OUTER_BOUND('',#4122,.T.);
#2788=FACE_OUTER_BOUND('',#4123,.T.);
#2789=FACE_OUTER_BOUND('',#4124,.T.);
#2790=FACE_OUTER_BOUND('',#4125,.T.);
#2791=FACE_OUTER_BOUND('',#4126,.T.);
#2792=FACE_OUTER_BOUND('',#4127,.T.);
#2793=FACE_OUTER_BOUND('',#4128,.T.);
#2794=FACE_OUTER_BOUND('',#4129,.T.);
#2795=FACE_OUTER_BOUND('',#4130,.T.);
#2796=FACE_OUTER_BOUND('',#4131,.T.);
#2797=FACE_OUTER_BOUND('',#4132,.T.);
#2798=FACE_OUTER_BOUND('',#4133,.T.);
#2799=FACE_OUTER_BOUND('',#4134,.T.);
#2800=FACE_OUTER_BOUND('',#4135,.T.);
#2801=FACE_OUTER_BOUND('',#4136,.T.);
#2802=FACE_OUTER_BOUND('',#4137,.T.);
#2803=FACE_OUTER_BOUND('',#4138,.T.);
#2804=FACE_OUTER_BOUND('',#4139,.T.);
#2805=FACE_OUTER_BOUND('',#4140,.T.);
#2806=FACE_OUTER_BOUND('',#4141,.T.);
#2807=FACE_OUTER_BOUND('',#4142,.T.);
#2808=FACE_OUTER_BOUND('',#4143,.T.);
#2809=FACE_OUTER_BOUND('',#4144,.T.);
#2810=FACE_OUTER_BOUND('',#4145,.T.);
#2811=FACE_OUTER_BOUND('',#4146,.T.);
#2812=FACE_OUTER_BOUND('',#4147,.T.);
#2813=FACE_OUTER_BOUND('',#4148,.T.);
#2814=FACE_OUTER_BOUND('',#4149,.T.);
#2815=FACE_OUTER_BOUND('',#4150,.T.);
#2816=FACE_OUTER_BOUND('',#4151,.T.);
#2817=FACE_OUTER_BOUND('',#4152,.T.);
#2818=FACE_OUTER_BOUND('',#4153,.T.);
#2819=FACE_OUTER_BOUND('',#4154,.T.);
#2820=FACE_OUTER_BOUND('',#4155,.T.);
#2821=FACE_OUTER_BOUND('',#4156,.T.);
#2822=FACE_OUTER_BOUND('',#4157,.T.);
#2823=FACE_OUTER_BOUND('',#4158,.T.);
#2824=FACE_OUTER_BOUND('',#4159,.T.);
#2825=FACE_OUTER_BOUND('',#4160,.T.);
#2826=FACE_OUTER_BOUND('',#4161,.T.);
#2827=FACE_OUTER_BOUND('',#4162,.T.);
#2828=FACE_OUTER_BOUND('',#4163,.T.);
#2829=FACE_OUTER_BOUND('',#4164,.T.);
#2830=FACE_OUTER_BOUND('',#4165,.T.);
#2831=FACE_OUTER_BOUND('',#4166,.T.);
#2832=FACE_OUTER_BOUND('',#4167,.T.);
#2833=FACE_OUTER_BOUND('',#4168,.T.);
#2834=FACE_OUTER_BOUND('',#4169,.T.);
#2835=FACE_OUTER_BOUND('',#4170,.T.);
#2836=FACE_OUTER_BOUND('',#4171,.T.);
#2837=FACE_OUTER_BOUND('',#4172,.T.);
#2838=FACE_OUTER_BOUND('',#4173,.T.);
#2839=FACE_OUTER_BOUND('',#4174,.T.);
#2840=FACE_OUTER_BOUND('',#4175,.T.);
#2841=FACE_OUTER_BOUND('',#4176,.T.);
#2842=FACE_OUTER_BOUND('',#4177,.T.);
#2843=FACE_OUTER_BOUND('',#4178,.T.);
#2844=FACE_OUTER_BOUND('',#4179,.T.);
#2845=FACE_OUTER_BOUND('',#4180,.T.);
#2846=FACE_OUTER_BOUND('',#4181,.T.);
#2847=FACE_OUTER_BOUND('',#4182,.T.);
#2848=FACE_OUTER_BOUND('',#4183,.T.);
#2849=FACE_OUTER_BOUND('',#4184,.T.);
#2850=FACE_OUTER_BOUND('',#4185,.T.);
#2851=FACE_OUTER_BOUND('',#4186,.T.);
#2852=FACE_OUTER_BOUND('',#4187,.T.);
#2853=FACE_OUTER_BOUND('',#4188,.T.);
#2854=FACE_OUTER_BOUND('',#4189,.T.);
#2855=FACE_OUTER_BOUND('',#4190,.T.);
#2856=FACE_OUTER_BOUND('',#4191,.T.);
#2857=FACE_OUTER_BOUND('',#4192,.T.);
#2858=FACE_OUTER_BOUND('',#4193,.T.);
#2859=FACE_OUTER_BOUND('',#4194,.T.);
#2860=FACE_OUTER_BOUND('',#4195,.T.);
#2861=FACE_OUTER_BOUND('',#4196,.T.);
#2862=FACE_OUTER_BOUND('',#4197,.T.);
#2863=FACE_OUTER_BOUND('',#4198,.T.);
#2864=FACE_OUTER_BOUND('',#4199,.T.);
#2865=FACE_OUTER_BOUND('',#4200,.T.);
#2866=FACE_OUTER_BOUND('',#4201,.T.);
#2867=FACE_OUTER_BOUND('',#4202,.T.);
#2868=FACE_OUTER_BOUND('',#4203,.T.);
#2869=FACE_OUTER_BOUND('',#4204,.T.);
#2870=FACE_OUTER_BOUND('',#4205,.T.);
#2871=FACE_OUTER_BOUND('',#4206,.T.);
#2872=FACE_OUTER_BOUND('',#4207,.T.);
#2873=FACE_OUTER_BOUND('',#4208,.T.);
#2874=FACE_OUTER_BOUND('',#4209,.T.);
#2875=FACE_OUTER_BOUND('',#4210,.T.);
#2876=FACE_OUTER_BOUND('',#4211,.T.);
#2877=FACE_OUTER_BOUND('',#4212,.T.);
#2878=FACE_OUTER_BOUND('',#4213,.T.);
#2879=FACE_OUTER_BOUND('',#4214,.T.);
#2880=FACE_OUTER_BOUND('',#4215,.T.);
#2881=FACE_OUTER_BOUND('',#4216,.T.);
#2882=FACE_OUTER_BOUND('',#4217,.T.);
#2883=FACE_OUTER_BOUND('',#4218,.T.);
#2884=FACE_OUTER_BOUND('',#4219,.T.);
#2885=FACE_OUTER_BOUND('',#4220,.T.);
#2886=FACE_OUTER_BOUND('',#4221,.T.);
#2887=FACE_OUTER_BOUND('',#4222,.T.);
#2888=FACE_OUTER_BOUND('',#4223,.T.);
#2889=FACE_OUTER_BOUND('',#4224,.T.);
#2890=FACE_OUTER_BOUND('',#4225,.T.);
#2891=FACE_OUTER_BOUND('',#4226,.T.);
#2892=FACE_OUTER_BOUND('',#4227,.T.);
#2893=FACE_OUTER_BOUND('',#4228,.T.);
#2894=FACE_OUTER_BOUND('',#4229,.T.);
#2895=FACE_OUTER_BOUND('',#4230,.T.);
#2896=FACE_OUTER_BOUND('',#4231,.T.);
#2897=FACE_OUTER_BOUND('',#4232,.T.);
#2898=FACE_OUTER_BOUND('',#4233,.T.);
#2899=FACE_OUTER_BOUND('',#4234,.T.);
#2900=FACE_OUTER_BOUND('',#4235,.T.);
#2901=FACE_OUTER_BOUND('',#4236,.T.);
#2902=FACE_OUTER_BOUND('',#4237,.T.);
#2903=FACE_OUTER_BOUND('',#4238,.T.);
#2904=FACE_OUTER_BOUND('',#4239,.T.);
#2905=FACE_OUTER_BOUND('',#4240,.T.);
#2906=FACE_OUTER_BOUND('',#4241,.T.);
#2907=FACE_OUTER_BOUND('',#4242,.T.);
#2908=FACE_OUTER_BOUND('',#4243,.T.);
#2909=FACE_OUTER_BOUND('',#4245,.T.);
#2910=FACE_OUTER_BOUND('',#4247,.T.);
#2911=FACE_OUTER_BOUND('',#4248,.T.);
#2912=FACE_OUTER_BOUND('',#4249,.T.);
#2913=FACE_OUTER_BOUND('',#4250,.T.);
#2914=FACE_OUTER_BOUND('',#4251,.T.);
#2915=FACE_OUTER_BOUND('',#4253,.T.);
#2916=FACE_OUTER_BOUND('',#4254,.T.);
#2917=FACE_OUTER_BOUND('',#4256,.T.);
#2918=FACE_OUTER_BOUND('',#4257,.T.);
#2919=FACE_OUTER_BOUND('',#4258,.T.);
#2920=FACE_OUTER_BOUND('',#4259,.T.);
#2921=FACE_OUTER_BOUND('',#4261,.T.);
#2922=FACE_OUTER_BOUND('',#4262,.T.);
#2923=FACE_OUTER_BOUND('',#4263,.T.);
#2924=FACE_OUTER_BOUND('',#4264,.T.);
#2925=FACE_OUTER_BOUND('',#4265,.T.);
#2926=FACE_OUTER_BOUND('',#4266,.T.);
#2927=FACE_OUTER_BOUND('',#4267,.T.);
#2928=FACE_OUTER_BOUND('',#4268,.T.);
#2929=FACE_OUTER_BOUND('',#4269,.T.);
#2930=FACE_OUTER_BOUND('',#4270,.T.);
#2931=FACE_OUTER_BOUND('',#4271,.T.);
#2932=FACE_OUTER_BOUND('',#4272,.T.);
#2933=FACE_OUTER_BOUND('',#4273,.T.);
#2934=FACE_OUTER_BOUND('',#4274,.T.);
#2935=FACE_OUTER_BOUND('',#4275,.T.);
#2936=FACE_OUTER_BOUND('',#4276,.T.);
#2937=FACE_OUTER_BOUND('',#4277,.T.);
#2938=FACE_OUTER_BOUND('',#4278,.T.);
#2939=FACE_OUTER_BOUND('',#4279,.T.);
#2940=FACE_OUTER_BOUND('',#4280,.T.);
#2941=FACE_OUTER_BOUND('',#4281,.T.);
#2942=FACE_OUTER_BOUND('',#4282,.T.);
#2943=FACE_OUTER_BOUND('',#4283,.T.);
#2944=FACE_OUTER_BOUND('',#4284,.T.);
#2945=FACE_OUTER_BOUND('',#4285,.T.);
#2946=FACE_OUTER_BOUND('',#4286,.T.);
#2947=FACE_OUTER_BOUND('',#4287,.T.);
#2948=FACE_OUTER_BOUND('',#4288,.T.);
#2949=FACE_OUTER_BOUND('',#4289,.T.);
#2950=FACE_OUTER_BOUND('',#4290,.T.);
#2951=FACE_OUTER_BOUND('',#4291,.T.);
#2952=FACE_OUTER_BOUND('',#4292,.T.);
#2953=FACE_OUTER_BOUND('',#4293,.T.);
#2954=FACE_OUTER_BOUND('',#4294,.T.);
#2955=FACE_OUTER_BOUND('',#4295,.T.);
#2956=FACE_OUTER_BOUND('',#4296,.T.);
#2957=FACE_OUTER_BOUND('',#4297,.T.);
#2958=FACE_OUTER_BOUND('',#4298,.T.);
#2959=FACE_OUTER_BOUND('',#4299,.T.);
#2960=FACE_OUTER_BOUND('',#4301,.T.);
#2961=FACE_OUTER_BOUND('',#4302,.T.);
#2962=FACE_OUTER_BOUND('',#4304,.T.);
#2963=FACE_OUTER_BOUND('',#4305,.T.);
#2964=FACE_OUTER_BOUND('',#4306,.T.);
#2965=FACE_OUTER_BOUND('',#4307,.T.);
#2966=FACE_OUTER_BOUND('',#4308,.T.);
#2967=FACE_OUTER_BOUND('',#4309,.T.);
#2968=FACE_OUTER_BOUND('',#4311,.T.);
#2969=FACE_OUTER_BOUND('',#4312,.T.);
#2970=FACE_OUTER_BOUND('',#4314,.T.);
#2971=FACE_OUTER_BOUND('',#4315,.T.);
#2972=FACE_OUTER_BOUND('',#4316,.T.);
#2973=FACE_OUTER_BOUND('',#4318,.T.);
#2974=FACE_OUTER_BOUND('',#4319,.T.);
#2975=FACE_OUTER_BOUND('',#4320,.T.);
#2976=FACE_OUTER_BOUND('',#4321,.T.);
#2977=FACE_OUTER_BOUND('',#4322,.T.);
#2978=FACE_OUTER_BOUND('',#4323,.T.);
#2979=FACE_OUTER_BOUND('',#4324,.T.);
#2980=FACE_OUTER_BOUND('',#4325,.T.);
#2981=FACE_OUTER_BOUND('',#4326,.T.);
#2982=FACE_OUTER_BOUND('',#4327,.T.);
#2983=FACE_OUTER_BOUND('',#4328,.T.);
#2984=FACE_OUTER_BOUND('',#4329,.T.);
#2985=FACE_OUTER_BOUND('',#4330,.T.);
#2986=FACE_OUTER_BOUND('',#4331,.T.);
#2987=FACE_OUTER_BOUND('',#4333,.T.);
#2988=FACE_OUTER_BOUND('',#4334,.T.);
#2989=FACE_OUTER_BOUND('',#4336,.T.);
#2990=FACE_OUTER_BOUND('',#4338,.T.);
#2991=FACE_OUTER_BOUND('',#4339,.T.);
#2992=FACE_OUTER_BOUND('',#4340,.T.);
#2993=FACE_OUTER_BOUND('',#4342,.T.);
#2994=FACE_OUTER_BOUND('',#4343,.T.);
#2995=FACE_OUTER_BOUND('',#4345,.T.);
#2996=FACE_OUTER_BOUND('',#4347,.T.);
#2997=FACE_OUTER_BOUND('',#4349,.T.);
#2998=FACE_OUTER_BOUND('',#4350,.T.);
#2999=FACE_OUTER_BOUND('',#4352,.T.);
#3000=FACE_OUTER_BOUND('',#4353,.T.);
#3001=FACE_OUTER_BOUND('',#4354,.T.);
#3002=FACE_OUTER_BOUND('',#4355,.T.);
#3003=FACE_OUTER_BOUND('',#4357,.T.);
#3004=FACE_OUTER_BOUND('',#4358,.T.);
#3005=FACE_OUTER_BOUND('',#4360,.T.);
#3006=FACE_OUTER_BOUND('',#4361,.T.);
#3007=FACE_OUTER_BOUND('',#4362,.T.);
#3008=FACE_OUTER_BOUND('',#4363,.T.);
#3009=FACE_OUTER_BOUND('',#4364,.T.);
#3010=FACE_OUTER_BOUND('',#4366,.T.);
#3011=FACE_OUTER_BOUND('',#4367,.T.);
#3012=FACE_OUTER_BOUND('',#4368,.T.);
#3013=FACE_OUTER_BOUND('',#4369,.T.);
#3014=FACE_OUTER_BOUND('',#4370,.T.);
#3015=FACE_OUTER_BOUND('',#4371,.T.);
#3016=FACE_OUTER_BOUND('',#4372,.T.);
#3017=FACE_OUTER_BOUND('',#4373,.T.);
#3018=FACE_OUTER_BOUND('',#4374,.T.);
#3019=FACE_OUTER_BOUND('',#4375,.T.);
#3020=FACE_OUTER_BOUND('',#4376,.T.);
#3021=FACE_OUTER_BOUND('',#4378,.T.);
#3022=FACE_OUTER_BOUND('',#4379,.T.);
#3023=FACE_OUTER_BOUND('',#4381,.T.);
#3024=FACE_OUTER_BOUND('',#4382,.T.);
#3025=FACE_OUTER_BOUND('',#4384,.T.);
#3026=FACE_OUTER_BOUND('',#4385,.T.);
#3027=FACE_OUTER_BOUND('',#4387,.T.);
#3028=FACE_OUTER_BOUND('',#4388,.T.);
#3029=FACE_OUTER_BOUND('',#4390,.T.);
#3030=FACE_OUTER_BOUND('',#4391,.T.);
#3031=FACE_OUTER_BOUND('',#4393,.T.);
#3032=FACE_OUTER_BOUND('',#4394,.T.);
#3033=FACE_OUTER_BOUND('',#4396,.T.);
#3034=FACE_OUTER_BOUND('',#4397,.T.);
#3035=FACE_OUTER_BOUND('',#4399,.T.);
#3036=FACE_OUTER_BOUND('',#4400,.T.);
#3037=FACE_OUTER_BOUND('',#4402,.T.);
#3038=FACE_OUTER_BOUND('',#4404,.T.);
#3039=FACE_OUTER_BOUND('',#4405,.T.);
#3040=FACE_OUTER_BOUND('',#4406,.T.);
#3041=FACE_OUTER_BOUND('',#4407,.T.);
#3042=FACE_OUTER_BOUND('',#4408,.T.);
#3043=FACE_OUTER_BOUND('',#4409,.T.);
#3044=FACE_OUTER_BOUND('',#4420,.T.);
#3045=FACE_OUTER_BOUND('',#4421,.T.);
#3046=FACE_OUTER_BOUND('',#4422,.T.);
#3047=FACE_OUTER_BOUND('',#4423,.T.);
#3048=FACE_OUTER_BOUND('',#4424,.T.);
#3049=FACE_OUTER_BOUND('',#4425,.T.);
#3050=FACE_OUTER_BOUND('',#4426,.T.);
#3051=FACE_OUTER_BOUND('',#4427,.T.);
#3052=FACE_OUTER_BOUND('',#4428,.T.);
#3053=FACE_OUTER_BOUND('',#4429,.T.);
#3054=FACE_OUTER_BOUND('',#4430,.T.);
#3055=FACE_OUTER_BOUND('',#4432,.T.);
#3056=FACE_OUTER_BOUND('',#4433,.T.);
#3057=FACE_OUTER_BOUND('',#4434,.T.);
#3058=FACE_OUTER_BOUND('',#4436,.T.);
#3059=FACE_OUTER_BOUND('',#4437,.T.);
#3060=FACE_OUTER_BOUND('',#4438,.T.);
#3061=FACE_OUTER_BOUND('',#4440,.T.);
#3062=FACE_OUTER_BOUND('',#4441,.T.);
#3063=FACE_OUTER_BOUND('',#4442,.T.);
#3064=FACE_OUTER_BOUND('',#4444,.T.);
#3065=FACE_OUTER_BOUND('',#4445,.T.);
#3066=FACE_OUTER_BOUND('',#4446,.T.);
#3067=FACE_OUTER_BOUND('',#4448,.T.);
#3068=FACE_OUTER_BOUND('',#4449,.T.);
#3069=FACE_OUTER_BOUND('',#4450,.T.);
#3070=FACE_OUTER_BOUND('',#4452,.T.);
#3071=FACE_OUTER_BOUND('',#4453,.T.);
#3072=FACE_OUTER_BOUND('',#4454,.T.);
#3073=FACE_OUTER_BOUND('',#4455,.T.);
#3074=FACE_OUTER_BOUND('',#4456,.T.);
#3075=FACE_OUTER_BOUND('',#4458,.T.);
#3076=FACE_OUTER_BOUND('',#4459,.T.);
#3077=FACE_OUTER_BOUND('',#4460,.T.);
#3078=FACE_OUTER_BOUND('',#4461,.T.);
#3079=FACE_OUTER_BOUND('',#4462,.T.);
#3080=FACE_OUTER_BOUND('',#4463,.T.);
#3081=FACE_OUTER_BOUND('',#4464,.T.);
#3082=FACE_OUTER_BOUND('',#4466,.T.);
#3083=FACE_OUTER_BOUND('',#4467,.T.);
#3084=FACE_OUTER_BOUND('',#4468,.T.);
#3085=FACE_OUTER_BOUND('',#4469,.T.);
#3086=FACE_OUTER_BOUND('',#4477,.T.);
#3087=FACE_OUTER_BOUND('',#4479,.T.);
#3088=FACE_OUTER_BOUND('',#4480,.T.);
#3089=FACE_OUTER_BOUND('',#4481,.T.);
#3090=FACE_OUTER_BOUND('',#4484,.T.);
#3091=FACE_OUTER_BOUND('',#4485,.T.);
#3092=FACE_OUTER_BOUND('',#4487,.T.);
#3093=FACE_OUTER_BOUND('',#4488,.T.);
#3094=FACE_OUTER_BOUND('',#4489,.T.);
#3095=FACE_OUTER_BOUND('',#4490,.T.);
#3096=FACE_OUTER_BOUND('',#4491,.T.);
#3097=FACE_OUTER_BOUND('',#4492,.T.);
#3098=FACE_OUTER_BOUND('',#4493,.T.);
#3099=FACE_OUTER_BOUND('',#4495,.T.);
#3100=FACE_OUTER_BOUND('',#4496,.T.);
#3101=FACE_OUTER_BOUND('',#4498,.T.);
#3102=FACE_OUTER_BOUND('',#4499,.T.);
#3103=FACE_OUTER_BOUND('',#4501,.T.);
#3104=FACE_OUTER_BOUND('',#4502,.T.);
#3105=FACE_OUTER_BOUND('',#4504,.T.);
#3106=FACE_OUTER_BOUND('',#4505,.T.);
#3107=FACE_OUTER_BOUND('',#4507,.T.);
#3108=FACE_OUTER_BOUND('',#4508,.T.);
#3109=FACE_OUTER_BOUND('',#4509,.T.);
#3110=FACE_OUTER_BOUND('',#4518,.T.);
#3111=FACE_OUTER_BOUND('',#4519,.T.);
#3112=FACE_OUTER_BOUND('',#4529,.T.);
#3113=FACE_OUTER_BOUND('',#4530,.T.);
#3114=FACE_OUTER_BOUND('',#4531,.T.);
#3115=FACE_OUTER_BOUND('',#4532,.T.);
#3116=FACE_OUTER_BOUND('',#4533,.T.);
#3117=FACE_OUTER_BOUND('',#4534,.T.);
#3118=FACE_OUTER_BOUND('',#4535,.T.);
#3119=FACE_OUTER_BOUND('',#4536,.T.);
#3120=FACE_OUTER_BOUND('',#4537,.T.);
#3121=FACE_OUTER_BOUND('',#4538,.T.);
#3122=FACE_OUTER_BOUND('',#4539,.T.);
#3123=FACE_OUTER_BOUND('',#4540,.T.);
#3124=FACE_OUTER_BOUND('',#4541,.T.);
#3125=FACE_OUTER_BOUND('',#4542,.T.);
#3126=FACE_OUTER_BOUND('',#4543,.T.);
#3127=FACE_OUTER_BOUND('',#4544,.T.);
#3128=FACE_OUTER_BOUND('',#4545,.T.);
#3129=FACE_OUTER_BOUND('',#4546,.T.);
#3130=FACE_OUTER_BOUND('',#4547,.T.);
#3131=FACE_OUTER_BOUND('',#4549,.T.);
#3132=FACE_OUTER_BOUND('',#4550,.T.);
#3133=FACE_OUTER_BOUND('',#4551,.T.);
#3134=FACE_OUTER_BOUND('',#4553,.T.);
#3135=FACE_OUTER_BOUND('',#4554,.T.);
#3136=FACE_OUTER_BOUND('',#4555,.T.);
#3137=FACE_OUTER_BOUND('',#4557,.T.);
#3138=FACE_OUTER_BOUND('',#4558,.T.);
#3139=FACE_OUTER_BOUND('',#4559,.T.);
#3140=FACE_OUTER_BOUND('',#4560,.T.);
#3141=FACE_OUTER_BOUND('',#4561,.T.);
#3142=FACE_OUTER_BOUND('',#4562,.T.);
#3143=FACE_OUTER_BOUND('',#4563,.T.);
#3144=FACE_OUTER_BOUND('',#4565,.T.);
#3145=FACE_OUTER_BOUND('',#4566,.T.);
#3146=FACE_OUTER_BOUND('',#4567,.T.);
#3147=FACE_OUTER_BOUND('',#4569,.T.);
#3148=FACE_OUTER_BOUND('',#4570,.T.);
#3149=FACE_OUTER_BOUND('',#4571,.T.);
#3150=FACE_OUTER_BOUND('',#4572,.T.);
#3151=FACE_OUTER_BOUND('',#4573,.T.);
#3152=FACE_OUTER_BOUND('',#4574,.T.);
#3153=FACE_OUTER_BOUND('',#4575,.T.);
#3154=FACE_OUTER_BOUND('',#4576,.T.);
#3155=FACE_OUTER_BOUND('',#4577,.T.);
#3156=FACE_OUTER_BOUND('',#4578,.T.);
#3157=FACE_OUTER_BOUND('',#4579,.T.);
#3158=FACE_OUTER_BOUND('',#4580,.T.);
#3159=FACE_OUTER_BOUND('',#4581,.T.);
#3160=FACE_OUTER_BOUND('',#4582,.T.);
#3161=FACE_OUTER_BOUND('',#4583,.T.);
#3162=FACE_OUTER_BOUND('',#4584,.T.);
#3163=FACE_OUTER_BOUND('',#4585,.T.);
#3164=FACE_OUTER_BOUND('',#4586,.T.);
#3165=FACE_OUTER_BOUND('',#4587,.T.);
#3166=FACE_OUTER_BOUND('',#4588,.T.);
#3167=FACE_OUTER_BOUND('',#4589,.T.);
#3168=FACE_OUTER_BOUND('',#4590,.T.);
#3169=FACE_OUTER_BOUND('',#4591,.T.);
#3170=FACE_OUTER_BOUND('',#4592,.T.);
#3171=FACE_OUTER_BOUND('',#4593,.T.);
#3172=FACE_OUTER_BOUND('',#4594,.T.);
#3173=FACE_OUTER_BOUND('',#4595,.T.);
#3174=FACE_OUTER_BOUND('',#4596,.T.);
#3175=FACE_OUTER_BOUND('',#4597,.T.);
#3176=FACE_OUTER_BOUND('',#4598,.T.);
#3177=FACE_OUTER_BOUND('',#4599,.T.);
#3178=FACE_OUTER_BOUND('',#4600,.T.);
#3179=FACE_OUTER_BOUND('',#4601,.T.);
#3180=FACE_OUTER_BOUND('',#4602,.T.);
#3181=FACE_OUTER_BOUND('',#4603,.T.);
#3182=FACE_OUTER_BOUND('',#4604,.T.);
#3183=FACE_OUTER_BOUND('',#4605,.T.);
#3184=FACE_OUTER_BOUND('',#4606,.T.);
#3185=FACE_OUTER_BOUND('',#4607,.T.);
#3186=FACE_OUTER_BOUND('',#4608,.T.);
#3187=FACE_OUTER_BOUND('',#4609,.T.);
#3188=FACE_OUTER_BOUND('',#4610,.T.);
#3189=FACE_OUTER_BOUND('',#4611,.T.);
#3190=FACE_OUTER_BOUND('',#4612,.T.);
#3191=FACE_OUTER_BOUND('',#4613,.T.);
#3192=FACE_OUTER_BOUND('',#4614,.T.);
#3193=FACE_OUTER_BOUND('',#4615,.T.);
#3194=FACE_OUTER_BOUND('',#4616,.T.);
#3195=FACE_OUTER_BOUND('',#4617,.T.);
#3196=FACE_OUTER_BOUND('',#4618,.T.);
#3197=FACE_OUTER_BOUND('',#4619,.T.);
#3198=FACE_OUTER_BOUND('',#4620,.T.);
#3199=FACE_OUTER_BOUND('',#4621,.T.);
#3200=FACE_OUTER_BOUND('',#4622,.T.);
#3201=FACE_OUTER_BOUND('',#4624,.T.);
#3202=FACE_OUTER_BOUND('',#4625,.T.);
#3203=FACE_OUTER_BOUND('',#4626,.T.);
#3204=FACE_OUTER_BOUND('',#4627,.T.);
#3205=FACE_OUTER_BOUND('',#4628,.T.);
#3206=FACE_OUTER_BOUND('',#4629,.T.);
#3207=FACE_OUTER_BOUND('',#4630,.T.);
#3208=FACE_OUTER_BOUND('',#4631,.T.);
#3209=FACE_OUTER_BOUND('',#4632,.T.);
#3210=FACE_OUTER_BOUND('',#4633,.T.);
#3211=FACE_OUTER_BOUND('',#4634,.T.);
#3212=FACE_OUTER_BOUND('',#4635,.T.);
#3213=FACE_OUTER_BOUND('',#4636,.T.);
#3214=FACE_OUTER_BOUND('',#4637,.T.);
#3215=FACE_OUTER_BOUND('',#4638,.T.);
#3216=FACE_OUTER_BOUND('',#4639,.T.);
#3217=FACE_OUTER_BOUND('',#4640,.T.);
#3218=FACE_OUTER_BOUND('',#4641,.T.);
#3219=FACE_OUTER_BOUND('',#4642,.T.);
#3220=FACE_OUTER_BOUND('',#4643,.T.);
#3221=FACE_OUTER_BOUND('',#4644,.T.);
#3222=FACE_OUTER_BOUND('',#4646,.T.);
#3223=FACE_OUTER_BOUND('',#4647,.T.);
#3224=FACE_OUTER_BOUND('',#4648,.T.);
#3225=FACE_OUTER_BOUND('',#4649,.T.);
#3226=FACE_OUTER_BOUND('',#4650,.T.);
#3227=FACE_OUTER_BOUND('',#4651,.T.);
#3228=FACE_OUTER_BOUND('',#4652,.T.);
#3229=FACE_OUTER_BOUND('',#4653,.T.);
#3230=FACE_OUTER_BOUND('',#4654,.T.);
#3231=FACE_OUTER_BOUND('',#4655,.T.);
#3232=FACE_OUTER_BOUND('',#4656,.T.);
#3233=FACE_OUTER_BOUND('',#4657,.T.);
#3234=FACE_OUTER_BOUND('',#4658,.T.);
#3235=FACE_OUTER_BOUND('',#4659,.T.);
#3236=FACE_OUTER_BOUND('',#4660,.T.);
#3237=FACE_OUTER_BOUND('',#4661,.T.);
#3238=FACE_OUTER_BOUND('',#4662,.T.);
#3239=FACE_OUTER_BOUND('',#4663,.T.);
#3240=FACE_OUTER_BOUND('',#4664,.T.);
#3241=FACE_OUTER_BOUND('',#4665,.T.);
#3242=FACE_OUTER_BOUND('',#4666,.T.);
#3243=FACE_OUTER_BOUND('',#4667,.T.);
#3244=FACE_OUTER_BOUND('',#4668,.T.);
#3245=FACE_OUTER_BOUND('',#4669,.T.);
#3246=FACE_OUTER_BOUND('',#4670,.T.);
#3247=FACE_OUTER_BOUND('',#4671,.T.);
#3248=FACE_OUTER_BOUND('',#4672,.T.);
#3249=FACE_OUTER_BOUND('',#4673,.T.);
#3250=FACE_OUTER_BOUND('',#4674,.T.);
#3251=FACE_OUTER_BOUND('',#4675,.T.);
#3252=FACE_OUTER_BOUND('',#4676,.T.);
#3253=FACE_OUTER_BOUND('',#4677,.T.);
#3254=FACE_OUTER_BOUND('',#4678,.T.);
#3255=FACE_OUTER_BOUND('',#4679,.T.);
#3256=FACE_OUTER_BOUND('',#4680,.T.);
#3257=FACE_OUTER_BOUND('',#4681,.T.);
#3258=FACE_OUTER_BOUND('',#4682,.T.);
#3259=FACE_OUTER_BOUND('',#4683,.T.);
#3260=FACE_OUTER_BOUND('',#4684,.T.);
#3261=FACE_OUTER_BOUND('',#4685,.T.);
#3262=FACE_OUTER_BOUND('',#4686,.T.);
#3263=FACE_OUTER_BOUND('',#4687,.T.);
#3264=FACE_OUTER_BOUND('',#4688,.T.);
#3265=FACE_OUTER_BOUND('',#4689,.T.);
#3266=FACE_OUTER_BOUND('',#4690,.T.);
#3267=FACE_OUTER_BOUND('',#4691,.T.);
#3268=FACE_OUTER_BOUND('',#4692,.T.);
#3269=FACE_OUTER_BOUND('',#4693,.T.);
#3270=FACE_OUTER_BOUND('',#4694,.T.);
#3271=FACE_OUTER_BOUND('',#4695,.T.);
#3272=FACE_OUTER_BOUND('',#4696,.T.);
#3273=FACE_OUTER_BOUND('',#4697,.T.);
#3274=FACE_OUTER_BOUND('',#4698,.T.);
#3275=FACE_OUTER_BOUND('',#4699,.T.);
#3276=FACE_OUTER_BOUND('',#4700,.T.);
#3277=FACE_OUTER_BOUND('',#4701,.T.);
#3278=FACE_OUTER_BOUND('',#4702,.T.);
#3279=FACE_OUTER_BOUND('',#4703,.T.);
#3280=FACE_OUTER_BOUND('',#4704,.T.);
#3281=FACE_OUTER_BOUND('',#4705,.T.);
#3282=FACE_OUTER_BOUND('',#4706,.T.);
#3283=FACE_OUTER_BOUND('',#4707,.T.);
#3284=FACE_OUTER_BOUND('',#4708,.T.);
#3285=FACE_OUTER_BOUND('',#4709,.T.);
#3286=FACE_OUTER_BOUND('',#4710,.T.);
#3287=FACE_OUTER_BOUND('',#4711,.T.);
#3288=FACE_OUTER_BOUND('',#4712,.T.);
#3289=FACE_OUTER_BOUND('',#4713,.T.);
#3290=FACE_OUTER_BOUND('',#4714,.T.);
#3291=FACE_OUTER_BOUND('',#4715,.T.);
#3292=FACE_OUTER_BOUND('',#4716,.T.);
#3293=FACE_OUTER_BOUND('',#4717,.T.);
#3294=FACE_OUTER_BOUND('',#4718,.T.);
#3295=FACE_OUTER_BOUND('',#4719,.T.);
#3296=FACE_OUTER_BOUND('',#4720,.T.);
#3297=FACE_OUTER_BOUND('',#4721,.T.);
#3298=FACE_OUTER_BOUND('',#4723,.T.);
#3299=FACE_OUTER_BOUND('',#4724,.T.);
#3300=FACE_OUTER_BOUND('',#4725,.T.);
#3301=FACE_OUTER_BOUND('',#4726,.T.);
#3302=FACE_OUTER_BOUND('',#4727,.T.);
#3303=FACE_OUTER_BOUND('',#4728,.T.);
#3304=FACE_OUTER_BOUND('',#4729,.T.);
#3305=FACE_OUTER_BOUND('',#4730,.T.);
#3306=FACE_OUTER_BOUND('',#4731,.T.);
#3307=FACE_OUTER_BOUND('',#4732,.T.);
#3308=FACE_OUTER_BOUND('',#4733,.T.);
#3309=FACE_OUTER_BOUND('',#4734,.T.);
#3310=FACE_OUTER_BOUND('',#4735,.T.);
#3311=FACE_OUTER_BOUND('',#4736,.T.);
#3312=FACE_OUTER_BOUND('',#4737,.T.);
#3313=FACE_OUTER_BOUND('',#4738,.T.);
#3314=FACE_OUTER_BOUND('',#4739,.T.);
#3315=FACE_OUTER_BOUND('',#4740,.T.);
#3316=FACE_OUTER_BOUND('',#4741,.T.);
#3317=FACE_OUTER_BOUND('',#4742,.T.);
#3318=FACE_OUTER_BOUND('',#4743,.T.);
#3319=FACE_OUTER_BOUND('',#4744,.T.);
#3320=FACE_OUTER_BOUND('',#4745,.T.);
#3321=FACE_OUTER_BOUND('',#4746,.T.);
#3322=FACE_OUTER_BOUND('',#4747,.T.);
#3323=FACE_OUTER_BOUND('',#4748,.T.);
#3324=FACE_OUTER_BOUND('',#4749,.T.);
#3325=FACE_OUTER_BOUND('',#4750,.T.);
#3326=FACE_OUTER_BOUND('',#4751,.T.);
#3327=FACE_OUTER_BOUND('',#4752,.T.);
#3328=FACE_OUTER_BOUND('',#4753,.T.);
#3329=FACE_OUTER_BOUND('',#4754,.T.);
#3330=FACE_OUTER_BOUND('',#4755,.T.);
#3331=FACE_OUTER_BOUND('',#4756,.T.);
#3332=FACE_OUTER_BOUND('',#4757,.T.);
#3333=FACE_OUTER_BOUND('',#4758,.T.);
#3334=FACE_OUTER_BOUND('',#4759,.T.);
#3335=FACE_OUTER_BOUND('',#4760,.T.);
#3336=FACE_OUTER_BOUND('',#4761,.T.);
#3337=FACE_OUTER_BOUND('',#4762,.T.);
#3338=FACE_OUTER_BOUND('',#4763,.T.);
#3339=FACE_OUTER_BOUND('',#4764,.T.);
#3340=FACE_OUTER_BOUND('',#4765,.T.);
#3341=FACE_OUTER_BOUND('',#4766,.T.);
#3342=FACE_OUTER_BOUND('',#4767,.T.);
#3343=FACE_OUTER_BOUND('',#4768,.T.);
#3344=FACE_OUTER_BOUND('',#4769,.T.);
#3345=FACE_OUTER_BOUND('',#4770,.T.);
#3346=FACE_OUTER_BOUND('',#4771,.T.);
#3347=FACE_OUTER_BOUND('',#4772,.T.);
#3348=FACE_OUTER_BOUND('',#4773,.T.);
#3349=FACE_OUTER_BOUND('',#4774,.T.);
#3350=FACE_OUTER_BOUND('',#4775,.T.);
#3351=FACE_OUTER_BOUND('',#4776,.T.);
#3352=FACE_OUTER_BOUND('',#4777,.T.);
#3353=FACE_OUTER_BOUND('',#4778,.T.);
#3354=FACE_OUTER_BOUND('',#4779,.T.);
#3355=FACE_OUTER_BOUND('',#4780,.T.);
#3356=FACE_OUTER_BOUND('',#4781,.T.);
#3357=FACE_OUTER_BOUND('',#4782,.T.);
#3358=FACE_OUTER_BOUND('',#4783,.T.);
#3359=FACE_OUTER_BOUND('',#4784,.T.);
#3360=FACE_OUTER_BOUND('',#4785,.T.);
#3361=FACE_OUTER_BOUND('',#4786,.T.);
#3362=FACE_OUTER_BOUND('',#4787,.T.);
#3363=FACE_OUTER_BOUND('',#4788,.T.);
#3364=FACE_OUTER_BOUND('',#4789,.T.);
#3365=FACE_OUTER_BOUND('',#4790,.T.);
#3366=FACE_OUTER_BOUND('',#4791,.T.);
#3367=FACE_OUTER_BOUND('',#4792,.T.);
#3368=FACE_OUTER_BOUND('',#4793,.T.);
#3369=FACE_OUTER_BOUND('',#4794,.T.);
#3370=FACE_OUTER_BOUND('',#4795,.T.);
#3371=FACE_OUTER_BOUND('',#4796,.T.);
#3372=FACE_OUTER_BOUND('',#4797,.T.);
#3373=FACE_OUTER_BOUND('',#4798,.T.);
#3374=FACE_OUTER_BOUND('',#4799,.T.);
#3375=FACE_OUTER_BOUND('',#4800,.T.);
#3376=FACE_OUTER_BOUND('',#4801,.T.);
#3377=FACE_OUTER_BOUND('',#4802,.T.);
#3378=FACE_OUTER_BOUND('',#4803,.T.);
#3379=FACE_OUTER_BOUND('',#4804,.T.);
#3380=FACE_OUTER_BOUND('',#4805,.T.);
#3381=FACE_OUTER_BOUND('',#4806,.T.);
#3382=FACE_OUTER_BOUND('',#4807,.T.);
#3383=FACE_OUTER_BOUND('',#4808,.T.);
#3384=FACE_OUTER_BOUND('',#4809,.T.);
#3385=FACE_OUTER_BOUND('',#4810,.T.);
#3386=FACE_OUTER_BOUND('',#4811,.T.);
#3387=FACE_OUTER_BOUND('',#4812,.T.);
#3388=FACE_OUTER_BOUND('',#4813,.T.);
#3389=FACE_OUTER_BOUND('',#4814,.T.);
#3390=FACE_OUTER_BOUND('',#4815,.T.);
#3391=FACE_OUTER_BOUND('',#4816,.T.);
#3392=FACE_OUTER_BOUND('',#4817,.T.);
#3393=FACE_OUTER_BOUND('',#4818,.T.);
#3394=FACE_OUTER_BOUND('',#4819,.T.);
#3395=FACE_OUTER_BOUND('',#4820,.T.);
#3396=FACE_OUTER_BOUND('',#4821,.T.);
#3397=FACE_OUTER_BOUND('',#4822,.T.);
#3398=FACE_OUTER_BOUND('',#4823,.T.);
#3399=FACE_OUTER_BOUND('',#4824,.T.);
#3400=FACE_OUTER_BOUND('',#4825,.T.);
#3401=FACE_OUTER_BOUND('',#4826,.T.);
#3402=FACE_OUTER_BOUND('',#4827,.T.);
#3403=FACE_OUTER_BOUND('',#4828,.T.);
#3404=FACE_OUTER_BOUND('',#4829,.T.);
#3405=FACE_OUTER_BOUND('',#4830,.T.);
#3406=FACE_OUTER_BOUND('',#4831,.T.);
#3407=FACE_OUTER_BOUND('',#4832,.T.);
#3408=FACE_OUTER_BOUND('',#4834,.T.);
#3409=FACE_OUTER_BOUND('',#4835,.T.);
#3410=FACE_OUTER_BOUND('',#4836,.T.);
#3411=FACE_OUTER_BOUND('',#4837,.T.);
#3412=FACE_OUTER_BOUND('',#4838,.T.);
#3413=FACE_OUTER_BOUND('',#4839,.T.);
#3414=FACE_OUTER_BOUND('',#4840,.T.);
#3415=FACE_OUTER_BOUND('',#4841,.T.);
#3416=FACE_OUTER_BOUND('',#4842,.T.);
#3417=FACE_OUTER_BOUND('',#4843,.T.);
#3418=FACE_OUTER_BOUND('',#4844,.T.);
#3419=FACE_OUTER_BOUND('',#4845,.T.);
#3420=FACE_OUTER_BOUND('',#4846,.T.);
#3421=FACE_OUTER_BOUND('',#4847,.T.);
#3422=FACE_OUTER_BOUND('',#4848,.T.);
#3423=FACE_OUTER_BOUND('',#4849,.T.);
#3424=FACE_OUTER_BOUND('',#4850,.T.);
#3425=FACE_OUTER_BOUND('',#4851,.T.);
#3426=FACE_OUTER_BOUND('',#4852,.T.);
#3427=FACE_OUTER_BOUND('',#4853,.T.);
#3428=FACE_OUTER_BOUND('',#4854,.T.);
#3429=FACE_OUTER_BOUND('',#4855,.T.);
#3430=FACE_OUTER_BOUND('',#4856,.T.);
#3431=FACE_OUTER_BOUND('',#4857,.T.);
#3432=FACE_OUTER_BOUND('',#4858,.T.);
#3433=FACE_OUTER_BOUND('',#4859,.T.);
#3434=FACE_OUTER_BOUND('',#4860,.T.);
#3435=FACE_OUTER_BOUND('',#4861,.T.);
#3436=FACE_OUTER_BOUND('',#4862,.T.);
#3437=FACE_OUTER_BOUND('',#4864,.T.);
#3438=FACE_OUTER_BOUND('',#4865,.T.);
#3439=FACE_OUTER_BOUND('',#4866,.T.);
#3440=FACE_OUTER_BOUND('',#4867,.T.);
#3441=FACE_OUTER_BOUND('',#4868,.T.);
#3442=FACE_OUTER_BOUND('',#4869,.T.);
#3443=FACE_OUTER_BOUND('',#4870,.T.);
#3444=FACE_OUTER_BOUND('',#4871,.T.);
#3445=FACE_OUTER_BOUND('',#4872,.T.);
#3446=FACE_OUTER_BOUND('',#4873,.T.);
#3447=FACE_OUTER_BOUND('',#4874,.T.);
#3448=FACE_OUTER_BOUND('',#4875,.T.);
#3449=FACE_OUTER_BOUND('',#4876,.T.);
#3450=FACE_OUTER_BOUND('',#4877,.T.);
#3451=FACE_OUTER_BOUND('',#4878,.T.);
#3452=FACE_OUTER_BOUND('',#4879,.T.);
#3453=FACE_OUTER_BOUND('',#4880,.T.);
#3454=FACE_OUTER_BOUND('',#4881,.T.);
#3455=FACE_OUTER_BOUND('',#4882,.T.);
#3456=FACE_OUTER_BOUND('',#4883,.T.);
#3457=FACE_OUTER_BOUND('',#4884,.T.);
#3458=FACE_OUTER_BOUND('',#4885,.T.);
#3459=FACE_OUTER_BOUND('',#4887,.T.);
#3460=FACE_OUTER_BOUND('',#4888,.T.);
#3461=FACE_OUTER_BOUND('',#4889,.T.);
#3462=FACE_OUTER_BOUND('',#4890,.T.);
#3463=FACE_OUTER_BOUND('',#4891,.T.);
#3464=FACE_OUTER_BOUND('',#4892,.T.);
#3465=FACE_OUTER_BOUND('',#4893,.T.);
#3466=FACE_OUTER_BOUND('',#4894,.T.);
#3467=FACE_OUTER_BOUND('',#4895,.T.);
#3468=FACE_OUTER_BOUND('',#4896,.T.);
#3469=FACE_OUTER_BOUND('',#4897,.T.);
#3470=FACE_OUTER_BOUND('',#4898,.T.);
#3471=FACE_OUTER_BOUND('',#4899,.T.);
#3472=FACE_OUTER_BOUND('',#4900,.T.);
#3473=FACE_OUTER_BOUND('',#4901,.T.);
#3474=FACE_OUTER_BOUND('',#4902,.T.);
#3475=FACE_OUTER_BOUND('',#4903,.T.);
#3476=FACE_OUTER_BOUND('',#4904,.T.);
#3477=FACE_OUTER_BOUND('',#4905,.T.);
#3478=FACE_OUTER_BOUND('',#4906,.T.);
#3479=FACE_OUTER_BOUND('',#4907,.T.);
#3480=FACE_OUTER_BOUND('',#4908,.T.);
#3481=FACE_OUTER_BOUND('',#4909,.T.);
#3482=FACE_OUTER_BOUND('',#4910,.T.);
#3483=FACE_OUTER_BOUND('',#4912,.T.);
#3484=FACE_OUTER_BOUND('',#4913,.T.);
#3485=FACE_OUTER_BOUND('',#4914,.T.);
#3486=FACE_OUTER_BOUND('',#4916,.T.);
#3487=FACE_OUTER_BOUND('',#4917,.T.);
#3488=FACE_OUTER_BOUND('',#4918,.T.);
#3489=FACE_OUTER_BOUND('',#4919,.T.);
#3490=FACE_OUTER_BOUND('',#4920,.T.);
#3491=FACE_OUTER_BOUND('',#4929,.T.);
#3492=FACE_OUTER_BOUND('',#4930,.T.);
#3493=FACE_OUTER_BOUND('',#4931,.T.);
#3494=FACE_OUTER_BOUND('',#4932,.T.);
#3495=FACE_OUTER_BOUND('',#4933,.T.);
#3496=FACE_OUTER_BOUND('',#4934,.T.);
#3497=FACE_OUTER_BOUND('',#4935,.T.);
#3498=FACE_OUTER_BOUND('',#4936,.T.);
#3499=FACE_OUTER_BOUND('',#4937,.T.);
#3500=FACE_OUTER_BOUND('',#4938,.T.);
#3501=FACE_OUTER_BOUND('',#4939,.T.);
#3502=FACE_OUTER_BOUND('',#4940,.T.);
#3503=FACE_OUTER_BOUND('',#4941,.T.);
#3504=FACE_OUTER_BOUND('',#4942,.T.);
#3505=FACE_OUTER_BOUND('',#4943,.T.);
#3506=FACE_OUTER_BOUND('',#4944,.T.);
#3507=FACE_OUTER_BOUND('',#4945,.T.);
#3508=FACE_OUTER_BOUND('',#4946,.T.);
#3509=FACE_OUTER_BOUND('',#4947,.T.);
#3510=FACE_OUTER_BOUND('',#4948,.T.);
#3511=FACE_OUTER_BOUND('',#4963,.T.);
#3512=FACE_OUTER_BOUND('',#4964,.T.);
#3513=FACE_OUTER_BOUND('',#4965,.T.);
#3514=FACE_OUTER_BOUND('',#4966,.T.);
#3515=FACE_OUTER_BOUND('',#4968,.T.);
#3516=FACE_OUTER_BOUND('',#4970,.T.);
#3517=FACE_OUTER_BOUND('',#4971,.T.);
#3518=FACE_OUTER_BOUND('',#4973,.T.);
#3519=FACE_OUTER_BOUND('',#4974,.T.);
#3520=FACE_OUTER_BOUND('',#4976,.T.);
#3521=FACE_OUTER_BOUND('',#4977,.T.);
#3522=FACE_OUTER_BOUND('',#4979,.T.);
#3523=FACE_OUTER_BOUND('',#4980,.T.);
#3524=FACE_OUTER_BOUND('',#4981,.T.);
#3525=FACE_OUTER_BOUND('',#4982,.T.);
#3526=FACE_OUTER_BOUND('',#4983,.T.);
#3527=FACE_OUTER_BOUND('',#4984,.T.);
#3528=FACE_OUTER_BOUND('',#4985,.T.);
#3529=FACE_OUTER_BOUND('',#4987,.T.);
#3530=FACE_OUTER_BOUND('',#4988,.T.);
#3531=FACE_OUTER_BOUND('',#4989,.T.);
#3532=FACE_OUTER_BOUND('',#4990,.T.);
#3533=FACE_OUTER_BOUND('',#4991,.T.);
#3534=FACE_OUTER_BOUND('',#4992,.T.);
#3535=FACE_OUTER_BOUND('',#4993,.T.);
#3536=FACE_OUTER_BOUND('',#4995,.T.);
#3537=FACE_OUTER_BOUND('',#4997,.T.);
#3538=FACE_OUTER_BOUND('',#4998,.T.);
#3539=FACE_OUTER_BOUND('',#4999,.T.);
#3540=FACE_OUTER_BOUND('',#5001,.T.);
#3541=FACE_OUTER_BOUND('',#5002,.T.);
#3542=FACE_OUTER_BOUND('',#5004,.T.);
#3543=FACE_OUTER_BOUND('',#5005,.T.);
#3544=FACE_OUTER_BOUND('',#5006,.T.);
#3545=FACE_OUTER_BOUND('',#5007,.T.);
#3546=FACE_OUTER_BOUND('',#5009,.T.);
#3547=FACE_OUTER_BOUND('',#5010,.T.);
#3548=FACE_OUTER_BOUND('',#5011,.T.);
#3549=FACE_OUTER_BOUND('',#5013,.T.);
#3550=FACE_OUTER_BOUND('',#5031,.T.);
#3551=FACE_OUTER_BOUND('',#5049,.T.);
#3552=FACE_OUTER_BOUND('',#5050,.T.);
#3553=FACE_OUTER_BOUND('',#5051,.T.);
#3554=FACE_OUTER_BOUND('',#5052,.T.);
#3555=FACE_OUTER_BOUND('',#5053,.T.);
#3556=FACE_OUTER_BOUND('',#5054,.T.);
#3557=FACE_OUTER_BOUND('',#5055,.T.);
#3558=FACE_OUTER_BOUND('',#5056,.T.);
#3559=FACE_OUTER_BOUND('',#5057,.T.);
#3560=FACE_OUTER_BOUND('',#5058,.T.);
#3561=FACE_OUTER_BOUND('',#5059,.T.);
#3562=FACE_OUTER_BOUND('',#5060,.T.);
#3563=FACE_OUTER_BOUND('',#5061,.T.);
#3564=FACE_OUTER_BOUND('',#5062,.T.);
#3565=FACE_OUTER_BOUND('',#5063,.T.);
#3566=FACE_OUTER_BOUND('',#5064,.T.);
#3567=FACE_OUTER_BOUND('',#5065,.T.);
#3568=FACE_OUTER_BOUND('',#5066,.T.);
#3569=FACE_OUTER_BOUND('',#5067,.T.);
#3570=FACE_OUTER_BOUND('',#5068,.T.);
#3571=FACE_OUTER_BOUND('',#5069,.T.);
#3572=FACE_OUTER_BOUND('',#5070,.T.);
#3573=FACE_OUTER_BOUND('',#5071,.T.);
#3574=FACE_OUTER_BOUND('',#5072,.T.);
#3575=FACE_OUTER_BOUND('',#5073,.T.);
#3576=FACE_OUTER_BOUND('',#5074,.T.);
#3577=FACE_OUTER_BOUND('',#5075,.T.);
#3578=FACE_OUTER_BOUND('',#5076,.T.);
#3579=FACE_OUTER_BOUND('',#5077,.T.);
#3580=FACE_OUTER_BOUND('',#5078,.T.);
#3581=FACE_OUTER_BOUND('',#5079,.T.);
#3582=FACE_OUTER_BOUND('',#5080,.T.);
#3583=FACE_OUTER_BOUND('',#5081,.T.);
#3584=FACE_OUTER_BOUND('',#5082,.T.);
#3585=FACE_OUTER_BOUND('',#5083,.T.);
#3586=FACE_OUTER_BOUND('',#5084,.T.);
#3587=FACE_OUTER_BOUND('',#5085,.T.);
#3588=FACE_OUTER_BOUND('',#5086,.T.);
#3589=FACE_OUTER_BOUND('',#5087,.T.);
#3590=FACE_OUTER_BOUND('',#5088,.T.);
#3591=FACE_OUTER_BOUND('',#5089,.T.);
#3592=FACE_OUTER_BOUND('',#5090,.T.);
#3593=FACE_OUTER_BOUND('',#5091,.T.);
#3594=FACE_OUTER_BOUND('',#5092,.T.);
#3595=FACE_OUTER_BOUND('',#5093,.T.);
#3596=FACE_OUTER_BOUND('',#5094,.T.);
#3597=FACE_OUTER_BOUND('',#5095,.T.);
#3598=FACE_OUTER_BOUND('',#5096,.T.);
#3599=FACE_OUTER_BOUND('',#5097,.T.);
#3600=FACE_OUTER_BOUND('',#5098,.T.);
#3601=FACE_OUTER_BOUND('',#5099,.T.);
#3602=FACE_OUTER_BOUND('',#5100,.T.);
#3603=FACE_OUTER_BOUND('',#5101,.T.);
#3604=FACE_OUTER_BOUND('',#5102,.T.);
#3605=FACE_OUTER_BOUND('',#5103,.T.);
#3606=FACE_OUTER_BOUND('',#5104,.T.);
#3607=FACE_OUTER_BOUND('',#5105,.T.);
#3608=FACE_OUTER_BOUND('',#5106,.T.);
#3609=FACE_OUTER_BOUND('',#5107,.T.);
#3610=FACE_OUTER_BOUND('',#5108,.T.);
#3611=FACE_OUTER_BOUND('',#5109,.T.);
#3612=FACE_OUTER_BOUND('',#5110,.T.);
#3613=FACE_OUTER_BOUND('',#5111,.T.);
#3614=FACE_OUTER_BOUND('',#5112,.T.);
#3615=FACE_OUTER_BOUND('',#5113,.T.);
#3616=FACE_OUTER_BOUND('',#5114,.T.);
#3617=FACE_OUTER_BOUND('',#5115,.T.);
#3618=FACE_OUTER_BOUND('',#5116,.T.);
#3619=FACE_OUTER_BOUND('',#5117,.T.);
#3620=FACE_OUTER_BOUND('',#5118,.T.);
#3621=FACE_OUTER_BOUND('',#5119,.T.);
#3622=FACE_OUTER_BOUND('',#5120,.T.);
#3623=FACE_OUTER_BOUND('',#5121,.T.);
#3624=FACE_OUTER_BOUND('',#5122,.T.);
#3625=FACE_OUTER_BOUND('',#5123,.T.);
#3626=FACE_OUTER_BOUND('',#5124,.T.);
#3627=FACE_OUTER_BOUND('',#5125,.T.);
#3628=FACE_OUTER_BOUND('',#5126,.T.);
#3629=FACE_OUTER_BOUND('',#5127,.T.);
#3630=FACE_OUTER_BOUND('',#5128,.T.);
#3631=FACE_OUTER_BOUND('',#5129,.T.);
#3632=FACE_OUTER_BOUND('',#5130,.T.);
#3633=FACE_OUTER_BOUND('',#5131,.T.);
#3634=FACE_OUTER_BOUND('',#5132,.T.);
#3635=FACE_OUTER_BOUND('',#5133,.T.);
#3636=FACE_OUTER_BOUND('',#5134,.T.);
#3637=FACE_OUTER_BOUND('',#5135,.T.);
#3638=FACE_OUTER_BOUND('',#5136,.T.);
#3639=FACE_OUTER_BOUND('',#5137,.T.);
#3640=FACE_OUTER_BOUND('',#5138,.T.);
#3641=FACE_OUTER_BOUND('',#5139,.T.);
#3642=FACE_OUTER_BOUND('',#5140,.T.);
#3643=FACE_OUTER_BOUND('',#5141,.T.);
#3644=FACE_OUTER_BOUND('',#5142,.T.);
#3645=FACE_OUTER_BOUND('',#5143,.T.);
#3646=FACE_OUTER_BOUND('',#5144,.T.);
#3647=FACE_OUTER_BOUND('',#5145,.T.);
#3648=FACE_OUTER_BOUND('',#5146,.T.);
#3649=FACE_OUTER_BOUND('',#5147,.T.);
#3650=FACE_OUTER_BOUND('',#5148,.T.);
#3651=FACE_OUTER_BOUND('',#5149,.T.);
#3652=FACE_OUTER_BOUND('',#5150,.T.);
#3653=FACE_OUTER_BOUND('',#5151,.T.);
#3654=FACE_OUTER_BOUND('',#5152,.T.);
#3655=FACE_OUTER_BOUND('',#5153,.T.);
#3656=FACE_OUTER_BOUND('',#5154,.T.);
#3657=FACE_OUTER_BOUND('',#5155,.T.);
#3658=FACE_OUTER_BOUND('',#5156,.T.);
#3659=FACE_OUTER_BOUND('',#5157,.T.);
#3660=FACE_OUTER_BOUND('',#5158,.T.);
#3661=FACE_OUTER_BOUND('',#5159,.T.);
#3662=FACE_OUTER_BOUND('',#5160,.T.);
#3663=FACE_OUTER_BOUND('',#5161,.T.);
#3664=FACE_OUTER_BOUND('',#5162,.T.);
#3665=FACE_OUTER_BOUND('',#5163,.T.);
#3666=FACE_OUTER_BOUND('',#5164,.T.);
#3667=FACE_OUTER_BOUND('',#5165,.T.);
#3668=FACE_OUTER_BOUND('',#5166,.T.);
#3669=FACE_OUTER_BOUND('',#5167,.T.);
#3670=FACE_OUTER_BOUND('',#5168,.T.);
#3671=FACE_OUTER_BOUND('',#5169,.T.);
#3672=FACE_OUTER_BOUND('',#5170,.T.);
#3673=FACE_OUTER_BOUND('',#5171,.T.);
#3674=FACE_OUTER_BOUND('',#5172,.T.);
#3675=FACE_OUTER_BOUND('',#5174,.T.);
#3676=FACE_OUTER_BOUND('',#5175,.T.);
#3677=FACE_OUTER_BOUND('',#5176,.T.);
#3678=FACE_OUTER_BOUND('',#5178,.T.);
#3679=FACE_OUTER_BOUND('',#5180,.T.);
#3680=FACE_OUTER_BOUND('',#5181,.T.);
#3681=FACE_OUTER_BOUND('',#5183,.T.);
#3682=FACE_OUTER_BOUND('',#5184,.T.);
#3683=FACE_OUTER_BOUND('',#5185,.T.);
#3684=FACE_OUTER_BOUND('',#5186,.T.);
#3685=FACE_OUTER_BOUND('',#5188,.T.);
#3686=FACE_OUTER_BOUND('',#5189,.T.);
#3687=FACE_OUTER_BOUND('',#5190,.T.);
#3688=FACE_OUTER_BOUND('',#5191,.T.);
#3689=FACE_OUTER_BOUND('',#5193,.T.);
#3690=FACE_OUTER_BOUND('',#5194,.T.);
#3691=FACE_OUTER_BOUND('',#5195,.T.);
#3692=FACE_OUTER_BOUND('',#5196,.T.);
#3693=FACE_OUTER_BOUND('',#5197,.T.);
#3694=FACE_OUTER_BOUND('',#5198,.T.);
#3695=FACE_OUTER_BOUND('',#5199,.T.);
#3696=FACE_OUTER_BOUND('',#5200,.T.);
#3697=FACE_OUTER_BOUND('',#5201,.T.);
#3698=FACE_OUTER_BOUND('',#5202,.T.);
#3699=FACE_OUTER_BOUND('',#5203,.T.);
#3700=FACE_OUTER_BOUND('',#5204,.T.);
#3701=FACE_OUTER_BOUND('',#5205,.T.);
#3702=FACE_OUTER_BOUND('',#5208,.T.);
#3703=FACE_OUTER_BOUND('',#5211,.T.);
#3704=FACE_OUTER_BOUND('',#5212,.T.);
#3705=FACE_OUTER_BOUND('',#5213,.T.);
#3706=FACE_OUTER_BOUND('',#5214,.T.);
#3707=FACE_OUTER_BOUND('',#5215,.T.);
#3708=FACE_OUTER_BOUND('',#5216,.T.);
#3709=FACE_OUTER_BOUND('',#5217,.T.);
#3710=FACE_OUTER_BOUND('',#5218,.T.);
#3711=FACE_OUTER_BOUND('',#5219,.T.);
#3712=FACE_OUTER_BOUND('',#5220,.T.);
#3713=FACE_OUTER_BOUND('',#5221,.T.);
#3714=FACE_OUTER_BOUND('',#5222,.T.);
#3715=FACE_OUTER_BOUND('',#5223,.T.);
#3716=FACE_OUTER_BOUND('',#5224,.T.);
#3717=FACE_OUTER_BOUND('',#5225,.T.);
#3718=FACE_OUTER_BOUND('',#5226,.T.);
#3719=FACE_OUTER_BOUND('',#5227,.T.);
#3720=FACE_OUTER_BOUND('',#5228,.T.);
#3721=FACE_OUTER_BOUND('',#5229,.T.);
#3722=FACE_OUTER_BOUND('',#5230,.T.);
#3723=FACE_OUTER_BOUND('',#5231,.T.);
#3724=FACE_OUTER_BOUND('',#5232,.T.);
#3725=FACE_OUTER_BOUND('',#5233,.T.);
#3726=FACE_OUTER_BOUND('',#5234,.T.);
#3727=FACE_OUTER_BOUND('',#5235,.T.);
#3728=FACE_OUTER_BOUND('',#5236,.T.);
#3729=FACE_OUTER_BOUND('',#5237,.T.);
#3730=FACE_OUTER_BOUND('',#5238,.T.);
#3731=FACE_OUTER_BOUND('',#5239,.T.);
#3732=FACE_OUTER_BOUND('',#5240,.T.);
#3733=FACE_OUTER_BOUND('',#5241,.T.);
#3734=FACE_OUTER_BOUND('',#5242,.T.);
#3735=FACE_OUTER_BOUND('',#5243,.T.);
#3736=FACE_OUTER_BOUND('',#5244,.T.);
#3737=FACE_OUTER_BOUND('',#5245,.T.);
#3738=FACE_OUTER_BOUND('',#5246,.T.);
#3739=FACE_OUTER_BOUND('',#5247,.T.);
#3740=FACE_OUTER_BOUND('',#5248,.T.);
#3741=FACE_OUTER_BOUND('',#5249,.T.);
#3742=FACE_OUTER_BOUND('',#5250,.T.);
#3743=FACE_OUTER_BOUND('',#5251,.T.);
#3744=FACE_OUTER_BOUND('',#5252,.T.);
#3745=FACE_OUTER_BOUND('',#5253,.T.);
#3746=FACE_OUTER_BOUND('',#5254,.T.);
#3747=FACE_OUTER_BOUND('',#5255,.T.);
#3748=FACE_OUTER_BOUND('',#5256,.T.);
#3749=FACE_OUTER_BOUND('',#5257,.T.);
#3750=FACE_OUTER_BOUND('',#5258,.T.);
#3751=FACE_OUTER_BOUND('',#5259,.T.);
#3752=FACE_OUTER_BOUND('',#5260,.T.);
#3753=FACE_OUTER_BOUND('',#5261,.T.);
#3754=FACE_OUTER_BOUND('',#5262,.T.);
#3755=FACE_OUTER_BOUND('',#5263,.T.);
#3756=FACE_OUTER_BOUND('',#5265,.T.);
#3757=FACE_OUTER_BOUND('',#5266,.T.);
#3758=FACE_OUTER_BOUND('',#5267,.T.);
#3759=FACE_OUTER_BOUND('',#5268,.T.);
#3760=FACE_OUTER_BOUND('',#5269,.T.);
#3761=FACE_OUTER_BOUND('',#5270,.T.);
#3762=FACE_OUTER_BOUND('',#5271,.T.);
#3763=FACE_OUTER_BOUND('',#5272,.T.);
#3764=FACE_OUTER_BOUND('',#5274,.T.);
#3765=FACE_OUTER_BOUND('',#5275,.T.);
#3766=FACE_OUTER_BOUND('',#5276,.T.);
#3767=FACE_OUTER_BOUND('',#5277,.T.);
#3768=FACE_OUTER_BOUND('',#5278,.T.);
#3769=FACE_OUTER_BOUND('',#5279,.T.);
#3770=FACE_OUTER_BOUND('',#5280,.T.);
#3771=FACE_OUTER_BOUND('',#5281,.T.);
#3772=FACE_OUTER_BOUND('',#5282,.T.);
#3773=FACE_OUTER_BOUND('',#5283,.T.);
#3774=FACE_OUTER_BOUND('',#5284,.T.);
#3775=FACE_OUTER_BOUND('',#5285,.T.);
#3776=FACE_OUTER_BOUND('',#5286,.T.);
#3777=FACE_OUTER_BOUND('',#5287,.T.);
#3778=FACE_OUTER_BOUND('',#5288,.T.);
#3779=FACE_OUTER_BOUND('',#5289,.T.);
#3780=FACE_OUTER_BOUND('',#5290,.T.);
#3781=FACE_OUTER_BOUND('',#5291,.T.);
#3782=FACE_OUTER_BOUND('',#5292,.T.);
#3783=FACE_OUTER_BOUND('',#5293,.T.);
#3784=FACE_OUTER_BOUND('',#5294,.T.);
#3785=FACE_OUTER_BOUND('',#5295,.T.);
#3786=FACE_OUTER_BOUND('',#5296,.T.);
#3787=FACE_OUTER_BOUND('',#5297,.T.);
#3788=FACE_OUTER_BOUND('',#5298,.T.);
#3789=FACE_OUTER_BOUND('',#5299,.T.);
#3790=FACE_OUTER_BOUND('',#5300,.T.);
#3791=FACE_OUTER_BOUND('',#5301,.T.);
#3792=FACE_OUTER_BOUND('',#5302,.T.);
#3793=FACE_OUTER_BOUND('',#5303,.T.);
#3794=FACE_OUTER_BOUND('',#5304,.T.);
#3795=FACE_OUTER_BOUND('',#5305,.T.);
#3796=FACE_OUTER_BOUND('',#5306,.T.);
#3797=FACE_OUTER_BOUND('',#5307,.T.);
#3798=FACE_OUTER_BOUND('',#5308,.T.);
#3799=FACE_OUTER_BOUND('',#5309,.T.);
#3800=FACE_OUTER_BOUND('',#5310,.T.);
#3801=FACE_OUTER_BOUND('',#5311,.T.);
#3802=FACE_OUTER_BOUND('',#5312,.T.);
#3803=FACE_OUTER_BOUND('',#5313,.T.);
#3804=FACE_OUTER_BOUND('',#5314,.T.);
#3805=FACE_OUTER_BOUND('',#5315,.T.);
#3806=FACE_OUTER_BOUND('',#5316,.T.);
#3807=FACE_OUTER_BOUND('',#5317,.T.);
#3808=FACE_OUTER_BOUND('',#5318,.T.);
#3809=FACE_OUTER_BOUND('',#5319,.T.);
#3810=FACE_OUTER_BOUND('',#5320,.T.);
#3811=FACE_OUTER_BOUND('',#5321,.T.);
#3812=FACE_OUTER_BOUND('',#5322,.T.);
#3813=FACE_OUTER_BOUND('',#5323,.T.);
#3814=FACE_OUTER_BOUND('',#5324,.T.);
#3815=FACE_OUTER_BOUND('',#5325,.T.);
#3816=FACE_OUTER_BOUND('',#5326,.T.);
#3817=FACE_OUTER_BOUND('',#5327,.T.);
#3818=FACE_OUTER_BOUND('',#5328,.T.);
#3819=FACE_OUTER_BOUND('',#5329,.T.);
#3820=FACE_OUTER_BOUND('',#5330,.T.);
#3821=FACE_OUTER_BOUND('',#5331,.T.);
#3822=FACE_OUTER_BOUND('',#5332,.T.);
#3823=FACE_OUTER_BOUND('',#5333,.T.);
#3824=FACE_OUTER_BOUND('',#5334,.T.);
#3825=FACE_OUTER_BOUND('',#5335,.T.);
#3826=FACE_OUTER_BOUND('',#5336,.T.);
#3827=FACE_OUTER_BOUND('',#5337,.T.);
#3828=FACE_OUTER_BOUND('',#5338,.T.);
#3829=FACE_OUTER_BOUND('',#5339,.T.);
#3830=FACE_OUTER_BOUND('',#5340,.T.);
#3831=FACE_OUTER_BOUND('',#5341,.T.);
#3832=FACE_OUTER_BOUND('',#5342,.T.);
#3833=FACE_OUTER_BOUND('',#5343,.T.);
#3834=FACE_OUTER_BOUND('',#5344,.T.);
#3835=FACE_OUTER_BOUND('',#5345,.T.);
#3836=FACE_OUTER_BOUND('',#5346,.T.);
#3837=FACE_OUTER_BOUND('',#5347,.T.);
#3838=FACE_OUTER_BOUND('',#5348,.T.);
#3839=FACE_OUTER_BOUND('',#5349,.T.);
#3840=FACE_OUTER_BOUND('',#5350,.T.);
#3841=FACE_OUTER_BOUND('',#5351,.T.);
#3842=FACE_OUTER_BOUND('',#5352,.T.);
#3843=FACE_OUTER_BOUND('',#5353,.T.);
#3844=FACE_OUTER_BOUND('',#5354,.T.);
#3845=FACE_OUTER_BOUND('',#5355,.T.);
#3846=FACE_OUTER_BOUND('',#5356,.T.);
#3847=FACE_OUTER_BOUND('',#5357,.T.);
#3848=FACE_OUTER_BOUND('',#5358,.T.);
#3849=FACE_OUTER_BOUND('',#5359,.T.);
#3850=FACE_OUTER_BOUND('',#5360,.T.);
#3851=FACE_OUTER_BOUND('',#5361,.T.);
#3852=FACE_OUTER_BOUND('',#5362,.T.);
#3853=FACE_OUTER_BOUND('',#5363,.T.);
#3854=FACE_OUTER_BOUND('',#5364,.T.);
#3855=FACE_OUTER_BOUND('',#5365,.T.);
#3856=FACE_OUTER_BOUND('',#5366,.T.);
#3857=FACE_OUTER_BOUND('',#5367,.T.);
#3858=FACE_OUTER_BOUND('',#5368,.T.);
#3859=FACE_OUTER_BOUND('',#5369,.T.);
#3860=FACE_OUTER_BOUND('',#5370,.T.);
#3861=FACE_OUTER_BOUND('',#5371,.T.);
#3862=FACE_OUTER_BOUND('',#5372,.T.);
#3863=FACE_OUTER_BOUND('',#5373,.T.);
#3864=FACE_OUTER_BOUND('',#5374,.T.);
#3865=FACE_OUTER_BOUND('',#5375,.T.);
#3866=FACE_OUTER_BOUND('',#5376,.T.);
#3867=FACE_OUTER_BOUND('',#5377,.T.);
#3868=FACE_OUTER_BOUND('',#5378,.T.);
#3869=FACE_OUTER_BOUND('',#5379,.T.);
#3870=FACE_OUTER_BOUND('',#5380,.T.);
#3871=FACE_OUTER_BOUND('',#5381,.T.);
#3872=FACE_OUTER_BOUND('',#5382,.T.);
#3873=FACE_OUTER_BOUND('',#5383,.T.);
#3874=FACE_OUTER_BOUND('',#5384,.T.);
#3875=FACE_OUTER_BOUND('',#5385,.T.);
#3876=FACE_OUTER_BOUND('',#5386,.T.);
#3877=FACE_OUTER_BOUND('',#5387,.T.);
#3878=FACE_OUTER_BOUND('',#5388,.T.);
#3879=FACE_OUTER_BOUND('',#5389,.T.);
#3880=FACE_OUTER_BOUND('',#5390,.T.);
#3881=FACE_OUTER_BOUND('',#5391,.T.);
#3882=FACE_OUTER_BOUND('',#5392,.T.);
#3883=FACE_OUTER_BOUND('',#5393,.T.);
#3884=FACE_OUTER_BOUND('',#5394,.T.);
#3885=FACE_OUTER_BOUND('',#5395,.T.);
#3886=FACE_OUTER_BOUND('',#5396,.T.);
#3887=FACE_OUTER_BOUND('',#5397,.T.);
#3888=FACE_OUTER_BOUND('',#5398,.T.);
#3889=FACE_OUTER_BOUND('',#5399,.T.);
#3890=FACE_OUTER_BOUND('',#5400,.T.);
#3891=FACE_OUTER_BOUND('',#5401,.T.);
#3892=FACE_OUTER_BOUND('',#5402,.T.);
#3893=FACE_OUTER_BOUND('',#5403,.T.);
#3894=FACE_OUTER_BOUND('',#5404,.T.);
#3895=FACE_OUTER_BOUND('',#5405,.T.);
#3896=FACE_OUTER_BOUND('',#5406,.T.);
#3897=FACE_OUTER_BOUND('',#5407,.T.);
#3898=FACE_OUTER_BOUND('',#5408,.T.);
#3899=FACE_OUTER_BOUND('',#5409,.T.);
#3900=FACE_OUTER_BOUND('',#5410,.T.);
#3901=FACE_OUTER_BOUND('',#5411,.T.);
#3902=FACE_OUTER_BOUND('',#5412,.T.);
#3903=FACE_OUTER_BOUND('',#5413,.T.);
#3904=FACE_OUTER_BOUND('',#5414,.T.);
#3905=FACE_OUTER_BOUND('',#5415,.T.);
#3906=FACE_OUTER_BOUND('',#5416,.T.);
#3907=FACE_OUTER_BOUND('',#5417,.T.);
#3908=FACE_OUTER_BOUND('',#5418,.T.);
#3909=FACE_OUTER_BOUND('',#5419,.T.);
#3910=FACE_OUTER_BOUND('',#5420,.T.);
#3911=FACE_OUTER_BOUND('',#5421,.T.);
#3912=FACE_OUTER_BOUND('',#5422,.T.);
#3913=FACE_OUTER_BOUND('',#5423,.T.);
#3914=FACE_OUTER_BOUND('',#5425,.T.);
#3915=FACE_OUTER_BOUND('',#5426,.T.);
#3916=FACE_OUTER_BOUND('',#5427,.T.);
#3917=FACE_OUTER_BOUND('',#5428,.T.);
#3918=FACE_OUTER_BOUND('',#5429,.T.);
#3919=FACE_OUTER_BOUND('',#5430,.T.);
#3920=FACE_OUTER_BOUND('',#5431,.T.);
#3921=FACE_OUTER_BOUND('',#5432,.T.);
#3922=FACE_OUTER_BOUND('',#5433,.T.);
#3923=FACE_OUTER_BOUND('',#5434,.T.);
#3924=FACE_OUTER_BOUND('',#5435,.T.);
#3925=FACE_OUTER_BOUND('',#5436,.T.);
#3926=FACE_OUTER_BOUND('',#5437,.T.);
#3927=FACE_OUTER_BOUND('',#5438,.T.);
#3928=FACE_OUTER_BOUND('',#5439,.T.);
#3929=FACE_OUTER_BOUND('',#5440,.T.);
#3930=FACE_OUTER_BOUND('',#5441,.T.);
#3931=FACE_OUTER_BOUND('',#5442,.T.);
#3932=FACE_OUTER_BOUND('',#5443,.T.);
#3933=FACE_OUTER_BOUND('',#5444,.T.);
#3934=FACE_OUTER_BOUND('',#5445,.T.);
#3935=FACE_OUTER_BOUND('',#5446,.T.);
#3936=FACE_OUTER_BOUND('',#5447,.T.);
#3937=FACE_OUTER_BOUND('',#5448,.T.);
#3938=FACE_OUTER_BOUND('',#5449,.T.);
#3939=FACE_OUTER_BOUND('',#5450,.T.);
#3940=FACE_OUTER_BOUND('',#5451,.T.);
#3941=FACE_OUTER_BOUND('',#5452,.T.);
#3942=FACE_OUTER_BOUND('',#5453,.T.);
#3943=FACE_OUTER_BOUND('',#5454,.T.);
#3944=FACE_OUTER_BOUND('',#5455,.T.);
#3945=FACE_OUTER_BOUND('',#5456,.T.);
#3946=FACE_OUTER_BOUND('',#5457,.T.);
#3947=FACE_OUTER_BOUND('',#5458,.T.);
#3948=FACE_OUTER_BOUND('',#5459,.T.);
#3949=FACE_OUTER_BOUND('',#5460,.T.);
#3950=FACE_OUTER_BOUND('',#5461,.T.);
#3951=FACE_OUTER_BOUND('',#5462,.T.);
#3952=FACE_OUTER_BOUND('',#5463,.T.);
#3953=FACE_OUTER_BOUND('',#5464,.T.);
#3954=FACE_OUTER_BOUND('',#5465,.T.);
#3955=FACE_OUTER_BOUND('',#5466,.T.);
#3956=FACE_OUTER_BOUND('',#5467,.T.);
#3957=FACE_OUTER_BOUND('',#5468,.T.);
#3958=FACE_OUTER_BOUND('',#5469,.T.);
#3959=FACE_OUTER_BOUND('',#5470,.T.);
#3960=FACE_OUTER_BOUND('',#5472,.T.);
#3961=FACE_OUTER_BOUND('',#5473,.T.);
#3962=FACE_OUTER_BOUND('',#5475,.T.);
#3963=FACE_OUTER_BOUND('',#5476,.T.);
#3964=FACE_OUTER_BOUND('',#5477,.T.);
#3965=FACE_OUTER_BOUND('',#5478,.T.);
#3966=FACE_OUTER_BOUND('',#5479,.T.);
#3967=FACE_OUTER_BOUND('',#5480,.T.);
#3968=FACE_OUTER_BOUND('',#5482,.T.);
#3969=FACE_OUTER_BOUND('',#5483,.T.);
#3970=FACE_OUTER_BOUND('',#5485,.T.);
#3971=FACE_OUTER_BOUND('',#5486,.T.);
#3972=FACE_OUTER_BOUND('',#5487,.T.);
#3973=FACE_OUTER_BOUND('',#5489,.T.);
#3974=EDGE_LOOP('',(#14662,#14663,#14664,#14665));
#3975=EDGE_LOOP('',(#14666,#14667,#14668,#14669));
#3976=EDGE_LOOP('',(#14670));
#3977=EDGE_LOOP('',(#14671));
#3978=EDGE_LOOP('',(#14672));
#3979=EDGE_LOOP('',(#14673));
#3980=EDGE_LOOP('',(#14674));
#3981=EDGE_LOOP('',(#14675));
#3982=EDGE_LOOP('',(#14676));
#3983=EDGE_LOOP('',(#14677));
#3984=EDGE_LOOP('',(#14678));
#3985=EDGE_LOOP('',(#14679));
#3986=EDGE_LOOP('',(#14680));
#3987=EDGE_LOOP('',(#14681,#14682,#14683,#14684));
#3988=EDGE_LOOP('',(#14685));
#3989=EDGE_LOOP('',(#14686));
#3990=EDGE_LOOP('',(#14687));
#3991=EDGE_LOOP('',(#14688));
#3992=EDGE_LOOP('',(#14689));
#3993=EDGE_LOOP('',(#14690));
#3994=EDGE_LOOP('',(#14691));
#3995=EDGE_LOOP('',(#14692));
#3996=EDGE_LOOP('',(#14693));
#3997=EDGE_LOOP('',(#14694));
#3998=EDGE_LOOP('',(#14695));
#3999=EDGE_LOOP('',(#14696,#14697,#14698,#14699));
#4000=EDGE_LOOP('',(#14700,#14701,#14702,#14703));
#4001=EDGE_LOOP('',(#14704,#14705,#14706,#14707));
#4002=EDGE_LOOP('',(#14708,#14709,#14710,#14711));
#4003=EDGE_LOOP('',(#14712,#14713,#14714,#14715));
#4004=EDGE_LOOP('',(#14716,#14717,#14718,#14719));
#4005=EDGE_LOOP('',(#14720,#14721,#14722,#14723));
#4006=EDGE_LOOP('',(#14724,#14725,#14726,#14727));
#4007=EDGE_LOOP('',(#14728,#14729,#14730,#14731));
#4008=EDGE_LOOP('',(#14732,#14733,#14734,#14735));
#4009=EDGE_LOOP('',(#14736,#14737,#14738,#14739));
#4010=EDGE_LOOP('',(#14740,#14741,#14742,#14743));
#4011=EDGE_LOOP('',(#14744,#14745,#14746,#14747));
#4012=EDGE_LOOP('',(#14748,#14749,#14750,#14751));
#4013=EDGE_LOOP('',(#14752,#14753,#14754,#14755));
#4014=EDGE_LOOP('',(#14756,#14757,#14758,#14759));
#4015=EDGE_LOOP('',(#14760,#14761,#14762,#14763));
#4016=EDGE_LOOP('',(#14764,#14765,#14766,#14767));
#4017=EDGE_LOOP('',(#14768,#14769,#14770,#14771));
#4018=EDGE_LOOP('',(#14772,#14773,#14774,#14775));
#4019=EDGE_LOOP('',(#14776,#14777,#14778,#14779));
#4020=EDGE_LOOP('',(#14780,#14781,#14782,#14783));
#4021=EDGE_LOOP('',(#14784,#14785,#14786,#14787));
#4022=EDGE_LOOP('',(#14788,#14789,#14790,#14791));
#4023=EDGE_LOOP('',(#14792,#14793,#14794,#14795));
#4024=EDGE_LOOP('',(#14796,#14797,#14798,#14799));
#4025=EDGE_LOOP('',(#14800,#14801,#14802,#14803));
#4026=EDGE_LOOP('',(#14804,#14805,#14806,#14807));
#4027=EDGE_LOOP('',(#14808,#14809,#14810,#14811));
#4028=EDGE_LOOP('',(#14812));
#4029=EDGE_LOOP('',(#14813));
#4030=EDGE_LOOP('',(#14814,#14815,#14816,#14817));
#4031=EDGE_LOOP('',(#14818,#14819,#14820,#14821));
#4032=EDGE_LOOP('',(#14822));
#4033=EDGE_LOOP('',(#14823));
#4034=EDGE_LOOP('',(#14824,#14825,#14826,#14827));
#4035=EDGE_LOOP('',(#14828,#14829,#14830,#14831));
#4036=EDGE_LOOP('',(#14832,#14833,#14834,#14835));
#4037=EDGE_LOOP('',(#14836));
#4038=EDGE_LOOP('',(#14837));
#4039=EDGE_LOOP('',(#14838,#14839,#14840,#14841));
#4040=EDGE_LOOP('',(#14842,#14843,#14844,#14845,#14846,#14847,#14848,#14849,
#14850));
#4041=EDGE_LOOP('',(#14851,#14852,#14853,#14854,#14855,#14856,#14857,#14858,
#14859));
#4042=EDGE_LOOP('',(#14860,#14861,#14862,#14863));
#4043=EDGE_LOOP('',(#14864,#14865,#14866,#14867));
#4044=EDGE_LOOP('',(#14868));
#4045=EDGE_LOOP('',(#14869,#14870,#14871,#14872));
#4046=EDGE_LOOP('',(#14873,#14874,#14875,#14876));
#4047=EDGE_LOOP('',(#14877,#14878,#14879,#14880,#14881));
#4048=EDGE_LOOP('',(#14882,#14883,#14884,#14885,#14886));
#4049=EDGE_LOOP('',(#14887,#14888,#14889,#14890));
#4050=EDGE_LOOP('',(#14891,#14892,#14893,#14894,#14895));
#4051=EDGE_LOOP('',(#14896));
#4052=EDGE_LOOP('',(#14897,#14898,#14899,#14900,#14901));
#4053=EDGE_LOOP('',(#14902,#14903,#14904,#14905));
#4054=EDGE_LOOP('',(#14906,#14907,#14908,#14909));
#4055=EDGE_LOOP('',(#14910,#14911,#14912,#14913));
#4056=EDGE_LOOP('',(#14914,#14915,#14916,#14917));
#4057=EDGE_LOOP('',(#14918,#14919));
#4058=EDGE_LOOP('',(#14920,#14921,#14922));
#4059=EDGE_LOOP('',(#14923,#14924,#14925));
#4060=EDGE_LOOP('',(#14926,#14927));
#4061=EDGE_LOOP('',(#14928,#14929,#14930,#14931,#14932,#14933,#14934,#14935));
#4062=EDGE_LOOP('',(#14936,#14937,#14938,#14939));
#4063=EDGE_LOOP('',(#14940,#14941,#14942,#14943));
#4064=EDGE_LOOP('',(#14944,#14945,#14946,#14947));
#4065=EDGE_LOOP('',(#14948,#14949,#14950,#14951));
#4066=EDGE_LOOP('',(#14952,#14953,#14954,#14955));
#4067=EDGE_LOOP('',(#14956,#14957,#14958,#14959));
#4068=EDGE_LOOP('',(#14960,#14961,#14962,#14963));
#4069=EDGE_LOOP('',(#14964,#14965,#14966,#14967));
#4070=EDGE_LOOP('',(#14968,#14969,#14970,#14971));
#4071=EDGE_LOOP('',(#14972,#14973,#14974,#14975));
#4072=EDGE_LOOP('',(#14976,#14977,#14978,#14979));
#4073=EDGE_LOOP('',(#14980,#14981,#14982,#14983));
#4074=EDGE_LOOP('',(#14984));
#4075=EDGE_LOOP('',(#14985));
#4076=EDGE_LOOP('',(#14986));
#4077=EDGE_LOOP('',(#14987));
#4078=EDGE_LOOP('',(#14988,#14989,#14990,#14991,#14992));
#4079=EDGE_LOOP('',(#14993,#14994,#14995,#14996,#14997,#14998));
#4080=EDGE_LOOP('',(#14999));
#4081=EDGE_LOOP('',(#15000));
#4082=EDGE_LOOP('',(#15001,#15002,#15003,#15004,#15005));
#4083=EDGE_LOOP('',(#15006));
#4084=EDGE_LOOP('',(#15007));
#4085=EDGE_LOOP('',(#15008,#15009,#15010,#15011));
#4086=EDGE_LOOP('',(#15012,#15013,#15014,#15015));
#4087=EDGE_LOOP('',(#15016,#15017,#15018,#15019));
#4088=EDGE_LOOP('',(#15020,#15021,#15022,#15023));
#4089=EDGE_LOOP('',(#15024,#15025,#15026,#15027));
#4090=EDGE_LOOP('',(#15028,#15029,#15030,#15031));
#4091=EDGE_LOOP('',(#15032,#15033,#15034,#15035));
#4092=EDGE_LOOP('',(#15036));
#4093=EDGE_LOOP('',(#15037));
#4094=EDGE_LOOP('',(#15038,#15039,#15040,#15041));
#4095=EDGE_LOOP('',(#15042,#15043,#15044,#15045));
#4096=EDGE_LOOP('',(#15046,#15047,#15048,#15049));
#4097=EDGE_LOOP('',(#15050,#15051,#15052,#15053));
#4098=EDGE_LOOP('',(#15054,#15055,#15056,#15057));
#4099=EDGE_LOOP('',(#15058,#15059,#15060,#15061));
#4100=EDGE_LOOP('',(#15062,#15063,#15064,#15065));
#4101=EDGE_LOOP('',(#15066,#15067,#15068,#15069,#15070));
#4102=EDGE_LOOP('',(#15071,#15072,#15073,#15074));
#4103=EDGE_LOOP('',(#15075,#15076,#15077,#15078));
#4104=EDGE_LOOP('',(#15079,#15080,#15081,#15082,#15083,#15084,#15085,#15086,
#15087,#15088,#15089,#15090));
#4105=EDGE_LOOP('',(#15091,#15092,#15093,#15094,#15095,#15096,#15097,#15098,
#15099,#15100));
#4106=EDGE_LOOP('',(#15101,#15102,#15103));
#4107=EDGE_LOOP('',(#15104,#15105,#15106,#15107,#15108,#15109,#15110,#15111,
#15112,#15113,#15114));
#4108=EDGE_LOOP('',(#15115,#15116,#15117,#15118));
#4109=EDGE_LOOP('',(#15119,#15120,#15121,#15122));
#4110=EDGE_LOOP('',(#15123,#15124,#15125,#15126));
#4111=EDGE_LOOP('',(#15127,#15128,#15129,#15130));
#4112=EDGE_LOOP('',(#15131,#15132,#15133,#15134));
#4113=EDGE_LOOP('',(#15135,#15136,#15137,#15138));
#4114=EDGE_LOOP('',(#15139,#15140,#15141,#15142));
#4115=EDGE_LOOP('',(#15143,#15144,#15145,#15146));
#4116=EDGE_LOOP('',(#15147,#15148,#15149,#15150,#15151,#15152));
#4117=EDGE_LOOP('',(#15153,#15154,#15155,#15156));
#4118=EDGE_LOOP('',(#15157,#15158,#15159));
#4119=EDGE_LOOP('',(#15160,#15161,#15162,#15163));
#4120=EDGE_LOOP('',(#15164,#15165,#15166));
#4121=EDGE_LOOP('',(#15167,#15168,#15169,#15170));
#4122=EDGE_LOOP('',(#15171,#15172,#15173));
#4123=EDGE_LOOP('',(#15174,#15175,#15176,#15177));
#4124=EDGE_LOOP('',(#15178,#15179,#15180));
#4125=EDGE_LOOP('',(#15181,#15182,#15183,#15184));
#4126=EDGE_LOOP('',(#15185,#15186,#15187));
#4127=EDGE_LOOP('',(#15188,#15189,#15190,#15191));
#4128=EDGE_LOOP('',(#15192,#15193,#15194));
#4129=EDGE_LOOP('',(#15195,#15196,#15197,#15198));
#4130=EDGE_LOOP('',(#15199,#15200,#15201));
#4131=EDGE_LOOP('',(#15202,#15203,#15204,#15205));
#4132=EDGE_LOOP('',(#15206,#15207,#15208));
#4133=EDGE_LOOP('',(#15209,#15210,#15211,#15212));
#4134=EDGE_LOOP('',(#15213,#15214,#15215));
#4135=EDGE_LOOP('',(#15216,#15217,#15218,#15219));
#4136=EDGE_LOOP('',(#15220,#15221,#15222));
#4137=EDGE_LOOP('',(#15223,#15224,#15225,#15226));
#4138=EDGE_LOOP('',(#15227,#15228,#15229));
#4139=EDGE_LOOP('',(#15230,#15231,#15232,#15233));
#4140=EDGE_LOOP('',(#15234,#15235,#15236));
#4141=EDGE_LOOP('',(#15237,#15238,#15239,#15240));
#4142=EDGE_LOOP('',(#15241,#15242,#15243));
#4143=EDGE_LOOP('',(#15244,#15245,#15246,#15247));
#4144=EDGE_LOOP('',(#15248,#15249,#15250));
#4145=EDGE_LOOP('',(#15251,#15252,#15253));
#4146=EDGE_LOOP('',(#15254,#15255,#15256,#15257));
#4147=EDGE_LOOP('',(#15258,#15259,#15260,#15261));
#4148=EDGE_LOOP('',(#15262,#15263,#15264));
#4149=EDGE_LOOP('',(#15265,#15266,#15267,#15268));
#4150=EDGE_LOOP('',(#15269,#15270,#15271));
#4151=EDGE_LOOP('',(#15272,#15273,#15274,#15275));
#4152=EDGE_LOOP('',(#15276,#15277,#15278));
#4153=EDGE_LOOP('',(#15279,#15280,#15281,#15282));
#4154=EDGE_LOOP('',(#15283,#15284,#15285));
#4155=EDGE_LOOP('',(#15286,#15287,#15288,#15289));
#4156=EDGE_LOOP('',(#15290,#15291,#15292));
#4157=EDGE_LOOP('',(#15293,#15294,#15295,#15296));
#4158=EDGE_LOOP('',(#15297,#15298,#15299));
#4159=EDGE_LOOP('',(#15300,#15301,#15302,#15303));
#4160=EDGE_LOOP('',(#15304,#15305,#15306));
#4161=EDGE_LOOP('',(#15307,#15308,#15309,#15310));
#4162=EDGE_LOOP('',(#15311,#15312,#15313));
#4163=EDGE_LOOP('',(#15314,#15315,#15316,#15317));
#4164=EDGE_LOOP('',(#15318,#15319,#15320));
#4165=EDGE_LOOP('',(#15321,#15322,#15323,#15324));
#4166=EDGE_LOOP('',(#15325,#15326,#15327));
#4167=EDGE_LOOP('',(#15328,#15329,#15330,#15331));
#4168=EDGE_LOOP('',(#15332,#15333,#15334));
#4169=EDGE_LOOP('',(#15335,#15336,#15337,#15338));
#4170=EDGE_LOOP('',(#15339,#15340,#15341));
#4171=EDGE_LOOP('',(#15342,#15343,#15344,#15345));
#4172=EDGE_LOOP('',(#15346,#15347,#15348));
#4173=EDGE_LOOP('',(#15349,#15350,#15351,#15352));
#4174=EDGE_LOOP('',(#15353,#15354,#15355));
#4175=EDGE_LOOP('',(#15356,#15357,#15358,#15359));
#4176=EDGE_LOOP('',(#15360,#15361,#15362));
#4177=EDGE_LOOP('',(#15363,#15364,#15365,#15366));
#4178=EDGE_LOOP('',(#15367,#15368,#15369));
#4179=EDGE_LOOP('',(#15370,#15371,#15372,#15373));
#4180=EDGE_LOOP('',(#15374,#15375,#15376));
#4181=EDGE_LOOP('',(#15377,#15378,#15379,#15380));
#4182=EDGE_LOOP('',(#15381,#15382,#15383));
#4183=EDGE_LOOP('',(#15384,#15385,#15386,#15387));
#4184=EDGE_LOOP('',(#15388,#15389,#15390));
#4185=EDGE_LOOP('',(#15391,#15392,#15393,#15394));
#4186=EDGE_LOOP('',(#15395,#15396,#15397));
#4187=EDGE_LOOP('',(#15398,#15399,#15400,#15401));
#4188=EDGE_LOOP('',(#15402,#15403,#15404));
#4189=EDGE_LOOP('',(#15405,#15406,#15407,#15408));
#4190=EDGE_LOOP('',(#15409,#15410,#15411));
#4191=EDGE_LOOP('',(#15412,#15413,#15414,#15415));
#4192=EDGE_LOOP('',(#15416,#15417,#15418));
#4193=EDGE_LOOP('',(#15419,#15420,#15421,#15422));
#4194=EDGE_LOOP('',(#15423,#15424,#15425));
#4195=EDGE_LOOP('',(#15426,#15427,#15428,#15429));
#4196=EDGE_LOOP('',(#15430,#15431,#15432));
#4197=EDGE_LOOP('',(#15433,#15434,#15435,#15436));
#4198=EDGE_LOOP('',(#15437,#15438,#15439));
#4199=EDGE_LOOP('',(#15440,#15441,#15442,#15443));
#4200=EDGE_LOOP('',(#15444,#15445,#15446));
#4201=EDGE_LOOP('',(#15447,#15448,#15449,#15450));
#4202=EDGE_LOOP('',(#15451,#15452,#15453));
#4203=EDGE_LOOP('',(#15454,#15455,#15456,#15457));
#4204=EDGE_LOOP('',(#15458,#15459,#15460));
#4205=EDGE_LOOP('',(#15461,#15462,#15463,#15464));
#4206=EDGE_LOOP('',(#15465,#15466,#15467,#15468));
#4207=EDGE_LOOP('',(#15469,#15470,#15471,#15472));
#4208=EDGE_LOOP('',(#15473,#15474,#15475,#15476));
#4209=EDGE_LOOP('',(#15477,#15478,#15479,#15480));
#4210=EDGE_LOOP('',(#15481,#15482,#15483));
#4211=EDGE_LOOP('',(#15484,#15485,#15486,#15487));
#4212=EDGE_LOOP('',(#15488,#15489,#15490));
#4213=EDGE_LOOP('',(#15491,#15492,#15493,#15494));
#4214=EDGE_LOOP('',(#15495,#15496,#15497));
#4215=EDGE_LOOP('',(#15498,#15499,#15500,#15501));
#4216=EDGE_LOOP('',(#15502,#15503,#15504));
#4217=EDGE_LOOP('',(#15505,#15506,#15507,#15508));
#4218=EDGE_LOOP('',(#15509,#15510,#15511));
#4219=EDGE_LOOP('',(#15512,#15513,#15514,#15515));
#4220=EDGE_LOOP('',(#15516,#15517,#15518));
#4221=EDGE_LOOP('',(#15519,#15520,#15521,#15522));
#4222=EDGE_LOOP('',(#15523,#15524,#15525));
#4223=EDGE_LOOP('',(#15526,#15527,#15528,#15529));
#4224=EDGE_LOOP('',(#15530,#15531,#15532));
#4225=EDGE_LOOP('',(#15533,#15534,#15535,#15536));
#4226=EDGE_LOOP('',(#15537,#15538,#15539));
#4227=EDGE_LOOP('',(#15540,#15541,#15542,#15543));
#4228=EDGE_LOOP('',(#15544,#15545,#15546));
#4229=EDGE_LOOP('',(#15547,#15548,#15549,#15550));
#4230=EDGE_LOOP('',(#15551,#15552,#15553));
#4231=EDGE_LOOP('',(#15554,#15555,#15556,#15557));
#4232=EDGE_LOOP('',(#15558,#15559,#15560));
#4233=EDGE_LOOP('',(#15561,#15562,#15563,#15564));
#4234=EDGE_LOOP('',(#15565,#15566,#15567));
#4235=EDGE_LOOP('',(#15568,#15569,#15570,#15571));
#4236=EDGE_LOOP('',(#15572,#15573,#15574));
#4237=EDGE_LOOP('',(#15575,#15576,#15577,#15578,#15579,#15580,#15581,#15582,
#15583,#15584));
#4238=EDGE_LOOP('',(#15585,#15586,#15587,#15588));
#4239=EDGE_LOOP('',(#15589,#15590,#15591,#15592));
#4240=EDGE_LOOP('',(#15593,#15594,#15595,#15596));
#4241=EDGE_LOOP('',(#15597,#15598,#15599,#15600,#15601,#15602,#15603,#15604,
#15605,#15606));
#4242=EDGE_LOOP('',(#15607,#15608,#15609,#15610));
#4243=EDGE_LOOP('',(#15611));
#4244=EDGE_LOOP('',(#15612));
#4245=EDGE_LOOP('',(#15613));
#4246=EDGE_LOOP('',(#15614));
#4247=EDGE_LOOP('',(#15615,#15616,#15617,#15618));
#4248=EDGE_LOOP('',(#15619,#15620,#15621,#15622,#15623,#15624));
#4249=EDGE_LOOP('',(#15625,#15626,#15627,#15628));
#4250=EDGE_LOOP('',(#15629,#15630,#15631));
#4251=EDGE_LOOP('',(#15632));
#4252=EDGE_LOOP('',(#15633));
#4253=EDGE_LOOP('',(#15634,#15635,#15636,#15637,#15638));
#4254=EDGE_LOOP('',(#15639,#15640,#15641,#15642,#15643,#15644,#15645));
#4255=EDGE_LOOP('',(#15646));
#4256=EDGE_LOOP('',(#15647,#15648,#15649,#15650));
#4257=EDGE_LOOP('',(#15651,#15652,#15653,#15654,#15655,#15656,#15657,#15658,
#15659,#15660,#15661,#15662,#15663,#15664,#15665,#15666,#15667,#15668,#15669,
#15670,#15671,#15672,#15673,#15674,#15675,#15676,#15677,#15678,#15679,#15680,
#15681,#15682,#15683,#15684,#15685,#15686,#15687,#15688,#15689,#15690,#15691,
#15692,#15693,#15694,#15695,#15696,#15697,#15698,#15699,#15700,#15701,#15702,
#15703,#15704,#15705,#15706,#15707,#15708,#15709,#15710,#15711,#15712,#15713,
#15714,#15715,#15716,#15717,#15718,#15719,#15720,#15721,#15722,#15723,#15724,
#15725,#15726,#15727,#15728,#15729,#15730,#15731,#15732,#15733,#15734,#15735,
#15736,#15737,#15738,#15739,#15740,#15741,#15742,#15743,#15744,#15745,#15746,
#15747,#15748,#15749,#15750,#15751,#15752,#15753,#15754,#15755,#15756,#15757,
#15758,#15759,#15760,#15761,#15762,#15763,#15764,#15765,#15766,#15767,#15768,
#15769,#15770,#15771,#15772,#15773,#15774));
#4258=EDGE_LOOP('',(#15775,#15776,#15777,#15778,#15779,#15780,#15781,#15782,
#15783,#15784,#15785,#15786,#15787,#15788,#15789,#15790,#15791,#15792,#15793,
#15794,#15795,#15796,#15797,#15798,#15799,#15800,#15801,#15802,#15803,#15804,
#15805,#15806,#15807,#15808,#15809,#15810,#15811,#15812,#15813,#15814,#15815,
#15816,#15817,#15818,#15819,#15820,#15821,#15822,#15823,#15824,#15825,#15826,
#15827,#15828,#15829,#15830,#15831,#15832,#15833,#15834,#15835,#15836,#15837,
#15838));
#4259=EDGE_LOOP('',(#15839));
#4260=EDGE_LOOP('',(#15840,#15841,#15842,#15843,#15844,#15845));
#4261=EDGE_LOOP('',(#15846,#15847,#15848,#15849));
#4262=EDGE_LOOP('',(#15850,#15851,#15852,#15853));
#4263=EDGE_LOOP('',(#15854,#15855,#15856,#15857));
#4264=EDGE_LOOP('',(#15858,#15859,#15860,#15861));
#4265=EDGE_LOOP('',(#15862,#15863,#15864,#15865,#15866));
#4266=EDGE_LOOP('',(#15867,#15868,#15869,#15870));
#4267=EDGE_LOOP('',(#15871,#15872,#15873,#15874));
#4268=EDGE_LOOP('',(#15875,#15876,#15877,#15878));
#4269=EDGE_LOOP('',(#15879,#15880,#15881,#15882));
#4270=EDGE_LOOP('',(#15883,#15884,#15885,#15886));
#4271=EDGE_LOOP('',(#15887,#15888,#15889,#15890));
#4272=EDGE_LOOP('',(#15891,#15892,#15893,#15894));
#4273=EDGE_LOOP('',(#15895,#15896,#15897,#15898));
#4274=EDGE_LOOP('',(#15899,#15900,#15901,#15902));
#4275=EDGE_LOOP('',(#15903,#15904,#15905,#15906));
#4276=EDGE_LOOP('',(#15907,#15908,#15909,#15910));
#4277=EDGE_LOOP('',(#15911,#15912,#15913,#15914));
#4278=EDGE_LOOP('',(#15915,#15916,#15917,#15918));
#4279=EDGE_LOOP('',(#15919,#15920,#15921,#15922));
#4280=EDGE_LOOP('',(#15923,#15924,#15925,#15926,#15927));
#4281=EDGE_LOOP('',(#15928,#15929,#15930,#15931,#15932,#15933,#15934,#15935,
#15936,#15937,#15938,#15939,#15940,#15941,#15942,#15943,#15944,#15945));
#4282=EDGE_LOOP('',(#15946,#15947,#15948,#15949));
#4283=EDGE_LOOP('',(#15950,#15951,#15952,#15953,#15954,#15955,#15956,#15957,
#15958,#15959,#15960,#15961,#15962,#15963,#15964,#15965,#15966,#15967));
#4284=EDGE_LOOP('',(#15968,#15969,#15970,#15971));
#4285=EDGE_LOOP('',(#15972,#15973,#15974,#15975));
#4286=EDGE_LOOP('',(#15976,#15977,#15978,#15979));
#4287=EDGE_LOOP('',(#15980,#15981,#15982,#15983,#15984,#15985,#15986,#15987,
#15988));
#4288=EDGE_LOOP('',(#15989,#15990,#15991,#15992,#15993,#15994,#15995,#15996,
#15997,#15998));
#4289=EDGE_LOOP('',(#15999,#16000,#16001));
#4290=EDGE_LOOP('',(#16002,#16003,#16004,#16005,#16006,#16007,#16008,#16009));
#4291=EDGE_LOOP('',(#16010,#16011,#16012,#16013));
#4292=EDGE_LOOP('',(#16014,#16015,#16016,#16017));
#4293=EDGE_LOOP('',(#16018,#16019,#16020,#16021,#16022,#16023,#16024,#16025,
#16026,#16027));
#4294=EDGE_LOOP('',(#16028,#16029,#16030,#16031));
#4295=EDGE_LOOP('',(#16032,#16033,#16034,#16035));
#4296=EDGE_LOOP('',(#16036,#16037,#16038,#16039));
#4297=EDGE_LOOP('',(#16040,#16041,#16042,#16043,#16044,#16045,#16046,#16047,
#16048,#16049));
#4298=EDGE_LOOP('',(#16050,#16051,#16052,#16053));
#4299=EDGE_LOOP('',(#16054));
#4300=EDGE_LOOP('',(#16055,#16056,#16057,#16058));
#4301=EDGE_LOOP('',(#16059));
#4302=EDGE_LOOP('',(#16060));
#4303=EDGE_LOOP('',(#16061));
#4304=EDGE_LOOP('',(#16062));
#4305=EDGE_LOOP('',(#16063,#16064,#16065,#16066));
#4306=EDGE_LOOP('',(#16067,#16068,#16069,#16070,#16071,#16072));
#4307=EDGE_LOOP('',(#16073,#16074,#16075,#16076));
#4308=EDGE_LOOP('',(#16077,#16078,#16079,#16080));
#4309=EDGE_LOOP('',(#16081));
#4310=EDGE_LOOP('',(#16082));
#4311=EDGE_LOOP('',(#16083,#16084,#16085,#16086,#16087));
#4312=EDGE_LOOP('',(#16088,#16089,#16090,#16091,#16092,#16093,#16094));
#4313=EDGE_LOOP('',(#16095));
#4314=EDGE_LOOP('',(#16096,#16097,#16098,#16099));
#4315=EDGE_LOOP('',(#16100,#16101,#16102,#16103,#16104,#16105));
#4316=EDGE_LOOP('',(#16106));
#4317=EDGE_LOOP('',(#16107));
#4318=EDGE_LOOP('',(#16108,#16109,#16110,#16111));
#4319=EDGE_LOOP('',(#16112,#16113,#16114,#16115));
#4320=EDGE_LOOP('',(#16116,#16117,#16118));
#4321=EDGE_LOOP('',(#16119,#16120,#16121,#16122));
#4322=EDGE_LOOP('',(#16123,#16124,#16125,#16126));
#4323=EDGE_LOOP('',(#16127,#16128,#16129,#16130));
#4324=EDGE_LOOP('',(#16131,#16132,#16133,#16134));
#4325=EDGE_LOOP('',(#16135,#16136,#16137,#16138));
#4326=EDGE_LOOP('',(#16139,#16140,#16141,#16142));
#4327=EDGE_LOOP('',(#16143,#16144,#16145,#16146));
#4328=EDGE_LOOP('',(#16147,#16148,#16149,#16150));
#4329=EDGE_LOOP('',(#16151,#16152,#16153,#16154));
#4330=EDGE_LOOP('',(#16155,#16156,#16157,#16158));
#4331=EDGE_LOOP('',(#16159));
#4332=EDGE_LOOP('',(#16160));
#4333=EDGE_LOOP('',(#16161,#16162,#16163,#16164));
#4334=EDGE_LOOP('',(#16165,#16166,#16167,#16168));
#4335=EDGE_LOOP('',(#16169,#16170,#16171,#16172));
#4336=EDGE_LOOP('',(#16173));
#4337=EDGE_LOOP('',(#16174));
#4338=EDGE_LOOP('',(#16175,#16176,#16177,#16178));
#4339=EDGE_LOOP('',(#16179,#16180,#16181,#16182));
#4340=EDGE_LOOP('',(#16183));
#4341=EDGE_LOOP('',(#16184));
#4342=EDGE_LOOP('',(#16185,#16186,#16187,#16188));
#4343=EDGE_LOOP('',(#16189));
#4344=EDGE_LOOP('',(#16190));
#4345=EDGE_LOOP('',(#16191,#16192,#16193,#16194));
#4346=EDGE_LOOP('',(#16195,#16196,#16197,#16198));
#4347=EDGE_LOOP('',(#16199));
#4348=EDGE_LOOP('',(#16200));
#4349=EDGE_LOOP('',(#16201,#16202,#16203,#16204));
#4350=EDGE_LOOP('',(#16205));
#4351=EDGE_LOOP('',(#16206));
#4352=EDGE_LOOP('',(#16207,#16208,#16209,#16210));
#4353=EDGE_LOOP('',(#16211,#16212,#16213,#16214));
#4354=EDGE_LOOP('',(#16215));
#4355=EDGE_LOOP('',(#16216));
#4356=EDGE_LOOP('',(#16217));
#4357=EDGE_LOOP('',(#16218,#16219,#16220,#16221));
#4358=EDGE_LOOP('',(#16222));
#4359=EDGE_LOOP('',(#16223));
#4360=EDGE_LOOP('',(#16224,#16225,#16226,#16227));
#4361=EDGE_LOOP('',(#16228,#16229,#16230,#16231));
#4362=EDGE_LOOP('',(#16232,#16233,#16234,#16235));
#4363=EDGE_LOOP('',(#16236,#16237,#16238,#16239));
#4364=EDGE_LOOP('',(#16240));
#4365=EDGE_LOOP('',(#16241,#16242,#16243,#16244));
#4366=EDGE_LOOP('',(#16245,#16246,#16247,#16248));
#4367=EDGE_LOOP('',(#16249,#16250,#16251,#16252));
#4368=EDGE_LOOP('',(#16253,#16254,#16255,#16256));
#4369=EDGE_LOOP('',(#16257,#16258,#16259,#16260));
#4370=EDGE_LOOP('',(#16261,#16262,#16263,#16264));
#4371=EDGE_LOOP('',(#16265,#16266,#16267,#16268));
#4372=EDGE_LOOP('',(#16269,#16270,#16271,#16272));
#4373=EDGE_LOOP('',(#16273,#16274,#16275,#16276));
#4374=EDGE_LOOP('',(#16277,#16278,#16279,#16280));
#4375=EDGE_LOOP('',(#16281,#16282,#16283,#16284,#16285,#16286));
#4376=EDGE_LOOP('',(#16287));
#4377=EDGE_LOOP('',(#16288));
#4378=EDGE_LOOP('',(#16289,#16290,#16291,#16292,#16293,#16294));
#4379=EDGE_LOOP('',(#16295));
#4380=EDGE_LOOP('',(#16296));
#4381=EDGE_LOOP('',(#16297,#16298,#16299,#16300,#16301,#16302));
#4382=EDGE_LOOP('',(#16303));
#4383=EDGE_LOOP('',(#16304));
#4384=EDGE_LOOP('',(#16305,#16306,#16307,#16308,#16309,#16310));
#4385=EDGE_LOOP('',(#16311));
#4386=EDGE_LOOP('',(#16312));
#4387=EDGE_LOOP('',(#16313,#16314,#16315,#16316,#16317,#16318));
#4388=EDGE_LOOP('',(#16319));
#4389=EDGE_LOOP('',(#16320));
#4390=EDGE_LOOP('',(#16321,#16322,#16323,#16324,#16325,#16326));
#4391=EDGE_LOOP('',(#16327));
#4392=EDGE_LOOP('',(#16328));
#4393=EDGE_LOOP('',(#16329,#16330,#16331,#16332,#16333,#16334));
#4394=EDGE_LOOP('',(#16335));
#4395=EDGE_LOOP('',(#16336));
#4396=EDGE_LOOP('',(#16337,#16338,#16339,#16340,#16341,#16342));
#4397=EDGE_LOOP('',(#16343));
#4398=EDGE_LOOP('',(#16344));
#4399=EDGE_LOOP('',(#16345,#16346,#16347,#16348,#16349,#16350));
#4400=EDGE_LOOP('',(#16351));
#4401=EDGE_LOOP('',(#16352));
#4402=EDGE_LOOP('',(#16353,#16354,#16355,#16356,#16357,#16358,#16359,#16360,
#16361,#16362,#16363,#16364,#16365,#16366,#16367,#16368,#16369,#16370,#16371,
#16372,#16373,#16374,#16375,#16376,#16377,#16378,#16379,#16380));
#4403=EDGE_LOOP('',(#16381));
#4404=EDGE_LOOP('',(#16382,#16383,#16384,#16385));
#4405=EDGE_LOOP('',(#16386,#16387,#16388,#16389));
#4406=EDGE_LOOP('',(#16390,#16391,#16392,#16393,#16394,#16395,#16396,#16397,
#16398,#16399,#16400,#16401,#16402,#16403,#16404,#16405,#16406,#16407,#16408,
#16409,#16410,#16411));
#4407=EDGE_LOOP('',(#16412,#16413,#16414,#16415));
#4408=EDGE_LOOP('',(#16416,#16417,#16418,#16419));
#4409=EDGE_LOOP('',(#16420));
#4410=EDGE_LOOP('',(#16421));
#4411=EDGE_LOOP('',(#16422));
#4412=EDGE_LOOP('',(#16423));
#4413=EDGE_LOOP('',(#16424));
#4414=EDGE_LOOP('',(#16425));
#4415=EDGE_LOOP('',(#16426));
#4416=EDGE_LOOP('',(#16427));
#4417=EDGE_LOOP('',(#16428));
#4418=EDGE_LOOP('',(#16429));
#4419=EDGE_LOOP('',(#16430,#16431,#16432,#16433));
#4420=EDGE_LOOP('',(#16434,#16435,#16436,#16437));
#4421=EDGE_LOOP('',(#16438,#16439,#16440,#16441));
#4422=EDGE_LOOP('',(#16442,#16443,#16444,#16445));
#4423=EDGE_LOOP('',(#16446,#16447,#16448,#16449));
#4424=EDGE_LOOP('',(#16450,#16451,#16452,#16453));
#4425=EDGE_LOOP('',(#16454,#16455,#16456,#16457));
#4426=EDGE_LOOP('',(#16458,#16459,#16460,#16461));
#4427=EDGE_LOOP('',(#16462,#16463,#16464,#16465));
#4428=EDGE_LOOP('',(#16466,#16467,#16468,#16469,#16470,#16471,#16472));
#4429=EDGE_LOOP('',(#16473,#16474,#16475,#16476,#16477));
#4430=EDGE_LOOP('',(#16478));
#4431=EDGE_LOOP('',(#16479));
#4432=EDGE_LOOP('',(#16480,#16481,#16482,#16483,#16484));
#4433=EDGE_LOOP('',(#16485,#16486,#16487,#16488,#16489));
#4434=EDGE_LOOP('',(#16490));
#4435=EDGE_LOOP('',(#16491));
#4436=EDGE_LOOP('',(#16492,#16493,#16494,#16495,#16496));
#4437=EDGE_LOOP('',(#16497,#16498,#16499,#16500,#16501));
#4438=EDGE_LOOP('',(#16502));
#4439=EDGE_LOOP('',(#16503));
#4440=EDGE_LOOP('',(#16504,#16505,#16506,#16507,#16508));
#4441=EDGE_LOOP('',(#16509,#16510,#16511,#16512,#16513));
#4442=EDGE_LOOP('',(#16514));
#4443=EDGE_LOOP('',(#16515));
#4444=EDGE_LOOP('',(#16516,#16517,#16518,#16519,#16520));
#4445=EDGE_LOOP('',(#16521,#16522,#16523,#16524,#16525));
#4446=EDGE_LOOP('',(#16526));
#4447=EDGE_LOOP('',(#16527));
#4448=EDGE_LOOP('',(#16528,#16529,#16530,#16531,#16532));
#4449=EDGE_LOOP('',(#16533,#16534,#16535,#16536,#16537));
#4450=EDGE_LOOP('',(#16538));
#4451=EDGE_LOOP('',(#16539));
#4452=EDGE_LOOP('',(#16540,#16541,#16542,#16543,#16544));
#4453=EDGE_LOOP('',(#16545,#16546,#16547,#16548,#16549,#16550));
#4454=EDGE_LOOP('',(#16551,#16552,#16553,#16554,#16555,#16556,#16557,#16558,
#16559,#16560,#16561,#16562,#16563,#16564,#16565,#16566,#16567));
#4455=EDGE_LOOP('',(#16568,#16569,#16570,#16571,#16572,#16573));
#4456=EDGE_LOOP('',(#16574));
#4457=EDGE_LOOP('',(#16575,#16576,#16577,#16578,#16579,#16580,#16581,#16582,
#16583,#16584,#16585,#16586,#16587,#16588,#16589,#16590,#16591));
#4458=EDGE_LOOP('',(#16592,#16593,#16594,#16595,#16596,#16597,#16598));
#4459=EDGE_LOOP('',(#16599,#16600,#16601,#16602,#16603,#16604));
#4460=EDGE_LOOP('',(#16605,#16606,#16607,#16608,#16609,#16610));
#4461=EDGE_LOOP('',(#16611,#16612,#16613,#16614,#16615,#16616));
#4462=EDGE_LOOP('',(#16617,#16618,#16619,#16620));
#4463=EDGE_LOOP('',(#16621,#16622,#16623,#16624,#16625));
#4464=EDGE_LOOP('',(#16626));
#4465=EDGE_LOOP('',(#16627));
#4466=EDGE_LOOP('',(#16628,#16629,#16630,#16631));
#4467=EDGE_LOOP('',(#16632,#16633,#16634,#16635,#16636));
#4468=EDGE_LOOP('',(#16637,#16638,#16639,#16640,#16641));
#4469=EDGE_LOOP('',(#16642));
#4470=EDGE_LOOP('',(#16643));
#4471=EDGE_LOOP('',(#16644));
#4472=EDGE_LOOP('',(#16645));
#4473=EDGE_LOOP('',(#16646));
#4474=EDGE_LOOP('',(#16647));
#4475=EDGE_LOOP('',(#16648));
#4476=EDGE_LOOP('',(#16649));
#4477=EDGE_LOOP('',(#16650,#16651,#16652,#16653,#16654));
#4478=EDGE_LOOP('',(#16655,#16656));
#4479=EDGE_LOOP('',(#16657,#16658,#16659,#16660,#16661));
#4480=EDGE_LOOP('',(#16662,#16663,#16664,#16665,#16666));
#4481=EDGE_LOOP('',(#16667));
#4482=EDGE_LOOP('',(#16668,#16669,#16670,#16671,#16672,#16673,#16674));
#4483=EDGE_LOOP('',(#16675));
#4484=EDGE_LOOP('',(#16676,#16677,#16678,#16679));
#4485=EDGE_LOOP('',(#16680,#16681,#16682,#16683));
#4486=EDGE_LOOP('',(#16684,#16685));
#4487=EDGE_LOOP('',(#16686,#16687,#16688,#16689));
#4488=EDGE_LOOP('',(#16690,#16691,#16692,#16693));
#4489=EDGE_LOOP('',(#16694,#16695,#16696,#16697));
#4490=EDGE_LOOP('',(#16698,#16699,#16700,#16701));
#4491=EDGE_LOOP('',(#16702,#16703,#16704,#16705));
#4492=EDGE_LOOP('',(#16706,#16707,#16708,#16709));
#4493=EDGE_LOOP('',(#16710));
#4494=EDGE_LOOP('',(#16711));
#4495=EDGE_LOOP('',(#16712,#16713,#16714,#16715));
#4496=EDGE_LOOP('',(#16716));
#4497=EDGE_LOOP('',(#16717));
#4498=EDGE_LOOP('',(#16718,#16719,#16720,#16721));
#4499=EDGE_LOOP('',(#16722));
#4500=EDGE_LOOP('',(#16723));
#4501=EDGE_LOOP('',(#16724,#16725,#16726,#16727));
#4502=EDGE_LOOP('',(#16728));
#4503=EDGE_LOOP('',(#16729));
#4504=EDGE_LOOP('',(#16730,#16731,#16732,#16733));
#4505=EDGE_LOOP('',(#16734));
#4506=EDGE_LOOP('',(#16735));
#4507=EDGE_LOOP('',(#16736,#16737,#16738,#16739));
#4508=EDGE_LOOP('',(#16740,#16741,#16742,#16743));
#4509=EDGE_LOOP('',(#16744,#16745,#16746,#16747));
#4510=EDGE_LOOP('',(#16748));
#4511=EDGE_LOOP('',(#16749));
#4512=EDGE_LOOP('',(#16750));
#4513=EDGE_LOOP('',(#16751));
#4514=EDGE_LOOP('',(#16752));
#4515=EDGE_LOOP('',(#16753));
#4516=EDGE_LOOP('',(#16754));
#4517=EDGE_LOOP('',(#16755));
#4518=EDGE_LOOP('',(#16756,#16757,#16758,#16759));
#4519=EDGE_LOOP('',(#16760,#16761,#16762,#16763));
#4520=EDGE_LOOP('',(#16764));
#4521=EDGE_LOOP('',(#16765));
#4522=EDGE_LOOP('',(#16766));
#4523=EDGE_LOOP('',(#16767,#16768,#16769,#16770));
#4524=EDGE_LOOP('',(#16771,#16772,#16773,#16774));
#4525=EDGE_LOOP('',(#16775));
#4526=EDGE_LOOP('',(#16776));
#4527=EDGE_LOOP('',(#16777));
#4528=EDGE_LOOP('',(#16778));
#4529=EDGE_LOOP('',(#16779,#16780,#16781,#16782));
#4530=EDGE_LOOP('',(#16783,#16784,#16785,#16786));
#4531=EDGE_LOOP('',(#16787,#16788,#16789,#16790));
#4532=EDGE_LOOP('',(#16791,#16792,#16793,#16794));
#4533=EDGE_LOOP('',(#16795,#16796,#16797,#16798));
#4534=EDGE_LOOP('',(#16799,#16800,#16801,#16802));
#4535=EDGE_LOOP('',(#16803,#16804,#16805,#16806));
#4536=EDGE_LOOP('',(#16807,#16808,#16809,#16810));
#4537=EDGE_LOOP('',(#16811,#16812,#16813,#16814));
#4538=EDGE_LOOP('',(#16815,#16816,#16817,#16818));
#4539=EDGE_LOOP('',(#16819,#16820,#16821,#16822));
#4540=EDGE_LOOP('',(#16823,#16824,#16825,#16826));
#4541=EDGE_LOOP('',(#16827,#16828,#16829,#16830));
#4542=EDGE_LOOP('',(#16831,#16832,#16833,#16834));
#4543=EDGE_LOOP('',(#16835,#16836,#16837,#16838));
#4544=EDGE_LOOP('',(#16839,#16840,#16841,#16842,#16843));
#4545=EDGE_LOOP('',(#16844,#16845,#16846,#16847));
#4546=EDGE_LOOP('',(#16848,#16849,#16850,#16851));
#4547=EDGE_LOOP('',(#16852,#16853,#16854,#16855,#16856,#16857,#16858,#16859));
#4548=EDGE_LOOP('',(#16860));
#4549=EDGE_LOOP('',(#16861,#16862,#16863,#16864));
#4550=EDGE_LOOP('',(#16865,#16866,#16867,#16868));
#4551=EDGE_LOOP('',(#16869,#16870,#16871,#16872,#16873,#16874,#16875,#16876));
#4552=EDGE_LOOP('',(#16877));
#4553=EDGE_LOOP('',(#16878,#16879,#16880,#16881,#16882,#16883,#16884,#16885));
#4554=EDGE_LOOP('',(#16886,#16887,#16888));
#4555=EDGE_LOOP('',(#16889));
#4556=EDGE_LOOP('',(#16890));
#4557=EDGE_LOOP('',(#16891,#16892,#16893,#16894,#16895,#16896,#16897,#16898,
#16899));
#4558=EDGE_LOOP('',(#16900,#16901,#16902,#16903,#16904,#16905,#16906,#16907));
#4559=EDGE_LOOP('',(#16908,#16909,#16910,#16911,#16912));
#4560=EDGE_LOOP('',(#16913,#16914,#16915,#16916));
#4561=EDGE_LOOP('',(#16917,#16918,#16919,#16920));
#4562=EDGE_LOOP('',(#16921,#16922,#16923,#16924));
#4563=EDGE_LOOP('',(#16925,#16926,#16927,#16928,#16929,#16930,#16931,#16932));
#4564=EDGE_LOOP('',(#16933,#16934));
#4565=EDGE_LOOP('',(#16935,#16936,#16937));
#4566=EDGE_LOOP('',(#16938,#16939,#16940,#16941,#16942,#16943,#16944,#16945,
#16946));
#4567=EDGE_LOOP('',(#16947));
#4568=EDGE_LOOP('',(#16948));
#4569=EDGE_LOOP('',(#16949,#16950,#16951,#16952,#16953,#16954,#16955,#16956));
#4570=EDGE_LOOP('',(#16957,#16958,#16959,#16960,#16961));
#4571=EDGE_LOOP('',(#16962,#16963,#16964,#16965));
#4572=EDGE_LOOP('',(#16966,#16967,#16968,#16969,#16970,#16971,#16972));
#4573=EDGE_LOOP('',(#16973,#16974,#16975,#16976));
#4574=EDGE_LOOP('',(#16977,#16978,#16979,#16980,#16981));
#4575=EDGE_LOOP('',(#16982,#16983,#16984,#16985));
#4576=EDGE_LOOP('',(#16986,#16987,#16988,#16989,#16990,#16991,#16992));
#4577=EDGE_LOOP('',(#16993,#16994,#16995,#16996));
#4578=EDGE_LOOP('',(#16997,#16998,#16999,#17000,#17001));
#4579=EDGE_LOOP('',(#17002,#17003,#17004,#17005,#17006));
#4580=EDGE_LOOP('',(#17007,#17008,#17009,#17010,#17011,#17012));
#4581=EDGE_LOOP('',(#17013,#17014,#17015,#17016,#17017));
#4582=EDGE_LOOP('',(#17018,#17019,#17020,#17021));
#4583=EDGE_LOOP('',(#17022,#17023,#17024,#17025));
#4584=EDGE_LOOP('',(#17026,#17027,#17028,#17029));
#4585=EDGE_LOOP('',(#17030,#17031,#17032,#17033));
#4586=EDGE_LOOP('',(#17034,#17035,#17036,#17037));
#4587=EDGE_LOOP('',(#17038,#17039,#17040,#17041));
#4588=EDGE_LOOP('',(#17042,#17043,#17044,#17045));
#4589=EDGE_LOOP('',(#17046,#17047,#17048,#17049));
#4590=EDGE_LOOP('',(#17050,#17051,#17052,#17053));
#4591=EDGE_LOOP('',(#17054,#17055,#17056,#17057));
#4592=EDGE_LOOP('',(#17058,#17059,#17060,#17061));
#4593=EDGE_LOOP('',(#17062,#17063,#17064,#17065));
#4594=EDGE_LOOP('',(#17066,#17067,#17068,#17069));
#4595=EDGE_LOOP('',(#17070,#17071,#17072,#17073));
#4596=EDGE_LOOP('',(#17074,#17075,#17076,#17077));
#4597=EDGE_LOOP('',(#17078,#17079,#17080,#17081));
#4598=EDGE_LOOP('',(#17082,#17083,#17084,#17085));
#4599=EDGE_LOOP('',(#17086,#17087,#17088,#17089));
#4600=EDGE_LOOP('',(#17090,#17091,#17092,#17093));
#4601=EDGE_LOOP('',(#17094,#17095,#17096,#17097));
#4602=EDGE_LOOP('',(#17098,#17099,#17100,#17101));
#4603=EDGE_LOOP('',(#17102,#17103,#17104,#17105));
#4604=EDGE_LOOP('',(#17106,#17107,#17108,#17109));
#4605=EDGE_LOOP('',(#17110,#17111,#17112,#17113));
#4606=EDGE_LOOP('',(#17114,#17115,#17116,#17117));
#4607=EDGE_LOOP('',(#17118,#17119,#17120,#17121));
#4608=EDGE_LOOP('',(#17122,#17123,#17124,#17125));
#4609=EDGE_LOOP('',(#17126,#17127,#17128,#17129));
#4610=EDGE_LOOP('',(#17130,#17131,#17132,#17133));
#4611=EDGE_LOOP('',(#17134,#17135,#17136,#17137));
#4612=EDGE_LOOP('',(#17138,#17139,#17140,#17141));
#4613=EDGE_LOOP('',(#17142,#17143,#17144,#17145));
#4614=EDGE_LOOP('',(#17146,#17147,#17148,#17149));
#4615=EDGE_LOOP('',(#17150,#17151,#17152,#17153));
#4616=EDGE_LOOP('',(#17154,#17155,#17156,#17157));
#4617=EDGE_LOOP('',(#17158,#17159,#17160,#17161));
#4618=EDGE_LOOP('',(#17162,#17163,#17164,#17165));
#4619=EDGE_LOOP('',(#17166,#17167,#17168,#17169));
#4620=EDGE_LOOP('',(#17170,#17171,#17172,#17173));
#4621=EDGE_LOOP('',(#17174,#17175,#17176,#17177));
#4622=EDGE_LOOP('',(#17178,#17179,#17180,#17181,#17182,#17183,#17184,#17185,
#17186,#17187,#17188,#17189,#17190,#17191,#17192,#17193,#17194,#17195,#17196,
#17197,#17198,#17199,#17200,#17201,#17202,#17203,#17204));
#4623=EDGE_LOOP('',(#17205,#17206,#17207,#17208,#17209,#17210,#17211,#17212,
#17213,#17214));
#4624=EDGE_LOOP('',(#17215,#17216,#17217,#17218));
#4625=EDGE_LOOP('',(#17219,#17220,#17221,#17222));
#4626=EDGE_LOOP('',(#17223,#17224,#17225,#17226));
#4627=EDGE_LOOP('',(#17227,#17228,#17229,#17230));
#4628=EDGE_LOOP('',(#17231,#17232,#17233,#17234));
#4629=EDGE_LOOP('',(#17235,#17236,#17237,#17238));
#4630=EDGE_LOOP('',(#17239,#17240,#17241,#17242));
#4631=EDGE_LOOP('',(#17243,#17244,#17245,#17246));
#4632=EDGE_LOOP('',(#17247,#17248,#17249,#17250));
#4633=EDGE_LOOP('',(#17251,#17252,#17253,#17254));
#4634=EDGE_LOOP('',(#17255,#17256,#17257,#17258));
#4635=EDGE_LOOP('',(#17259,#17260,#17261,#17262));
#4636=EDGE_LOOP('',(#17263,#17264,#17265,#17266));
#4637=EDGE_LOOP('',(#17267,#17268,#17269,#17270));
#4638=EDGE_LOOP('',(#17271,#17272,#17273,#17274));
#4639=EDGE_LOOP('',(#17275,#17276,#17277,#17278));
#4640=EDGE_LOOP('',(#17279,#17280,#17281,#17282));
#4641=EDGE_LOOP('',(#17283,#17284,#17285,#17286));
#4642=EDGE_LOOP('',(#17287,#17288,#17289,#17290));
#4643=EDGE_LOOP('',(#17291,#17292,#17293,#17294));
#4644=EDGE_LOOP('',(#17295,#17296,#17297,#17298,#17299,#17300,#17301,#17302,
#17303,#17304,#17305,#17306));
#4645=EDGE_LOOP('',(#17307,#17308,#17309,#17310,#17311,#17312,#17313,#17314));
#4646=EDGE_LOOP('',(#17315,#17316,#17317,#17318));
#4647=EDGE_LOOP('',(#17319,#17320,#17321,#17322));
#4648=EDGE_LOOP('',(#17323,#17324,#17325,#17326));
#4649=EDGE_LOOP('',(#17327,#17328,#17329,#17330));
#4650=EDGE_LOOP('',(#17331,#17332,#17333,#17334));
#4651=EDGE_LOOP('',(#17335,#17336,#17337,#17338));
#4652=EDGE_LOOP('',(#17339,#17340,#17341,#17342));
#4653=EDGE_LOOP('',(#17343,#17344,#17345,#17346));
#4654=EDGE_LOOP('',(#17347,#17348,#17349,#17350));
#4655=EDGE_LOOP('',(#17351,#17352,#17353,#17354,#17355,#17356,#17357,#17358,
#17359));
#4656=EDGE_LOOP('',(#17360,#17361,#17362,#17363));
#4657=EDGE_LOOP('',(#17364,#17365,#17366,#17367));
#4658=EDGE_LOOP('',(#17368,#17369,#17370,#17371));
#4659=EDGE_LOOP('',(#17372,#17373,#17374,#17375));
#4660=EDGE_LOOP('',(#17376,#17377,#17378,#17379));
#4661=EDGE_LOOP('',(#17380,#17381,#17382,#17383));
#4662=EDGE_LOOP('',(#17384,#17385,#17386,#17387));
#4663=EDGE_LOOP('',(#17388,#17389,#17390,#17391));
#4664=EDGE_LOOP('',(#17392,#17393,#17394,#17395));
#4665=EDGE_LOOP('',(#17396,#17397,#17398,#17399));
#4666=EDGE_LOOP('',(#17400,#17401,#17402,#17403));
#4667=EDGE_LOOP('',(#17404,#17405,#17406,#17407));
#4668=EDGE_LOOP('',(#17408,#17409,#17410,#17411));
#4669=EDGE_LOOP('',(#17412,#17413,#17414,#17415));
#4670=EDGE_LOOP('',(#17416,#17417,#17418,#17419));
#4671=EDGE_LOOP('',(#17420,#17421,#17422,#17423,#17424,#17425,#17426,#17427,
#17428,#17429,#17430,#17431,#17432,#17433,#17434));
#4672=EDGE_LOOP('',(#17435,#17436,#17437,#17438));
#4673=EDGE_LOOP('',(#17439,#17440,#17441,#17442));
#4674=EDGE_LOOP('',(#17443,#17444,#17445,#17446));
#4675=EDGE_LOOP('',(#17447,#17448,#17449,#17450));
#4676=EDGE_LOOP('',(#17451,#17452,#17453,#17454));
#4677=EDGE_LOOP('',(#17455,#17456,#17457,#17458));
#4678=EDGE_LOOP('',(#17459,#17460,#17461,#17462));
#4679=EDGE_LOOP('',(#17463,#17464,#17465,#17466));
#4680=EDGE_LOOP('',(#17467,#17468,#17469,#17470));
#4681=EDGE_LOOP('',(#17471,#17472,#17473,#17474));
#4682=EDGE_LOOP('',(#17475,#17476,#17477,#17478));
#4683=EDGE_LOOP('',(#17479,#17480,#17481,#17482));
#4684=EDGE_LOOP('',(#17483,#17484,#17485,#17486));
#4685=EDGE_LOOP('',(#17487,#17488,#17489,#17490));
#4686=EDGE_LOOP('',(#17491,#17492,#17493,#17494));
#4687=EDGE_LOOP('',(#17495,#17496,#17497,#17498));
#4688=EDGE_LOOP('',(#17499,#17500,#17501,#17502));
#4689=EDGE_LOOP('',(#17503,#17504,#17505,#17506));
#4690=EDGE_LOOP('',(#17507,#17508,#17509,#17510));
#4691=EDGE_LOOP('',(#17511,#17512,#17513,#17514));
#4692=EDGE_LOOP('',(#17515,#17516,#17517,#17518));
#4693=EDGE_LOOP('',(#17519,#17520,#17521,#17522));
#4694=EDGE_LOOP('',(#17523,#17524,#17525,#17526));
#4695=EDGE_LOOP('',(#17527,#17528,#17529,#17530));
#4696=EDGE_LOOP('',(#17531,#17532,#17533,#17534));
#4697=EDGE_LOOP('',(#17535,#17536,#17537,#17538));
#4698=EDGE_LOOP('',(#17539,#17540,#17541,#17542));
#4699=EDGE_LOOP('',(#17543,#17544,#17545,#17546));
#4700=EDGE_LOOP('',(#17547,#17548,#17549,#17550));
#4701=EDGE_LOOP('',(#17551,#17552,#17553,#17554));
#4702=EDGE_LOOP('',(#17555,#17556,#17557,#17558,#17559,#17560,#17561,#17562,
#17563,#17564,#17565,#17566,#17567,#17568,#17569,#17570,#17571,#17572,#17573,
#17574,#17575,#17576,#17577,#17578,#17579,#17580,#17581,#17582,#17583,#17584));
#4703=EDGE_LOOP('',(#17585,#17586,#17587,#17588));
#4704=EDGE_LOOP('',(#17589,#17590,#17591,#17592));
#4705=EDGE_LOOP('',(#17593,#17594,#17595,#17596));
#4706=EDGE_LOOP('',(#17597,#17598,#17599,#17600));
#4707=EDGE_LOOP('',(#17601,#17602,#17603,#17604));
#4708=EDGE_LOOP('',(#17605,#17606,#17607,#17608));
#4709=EDGE_LOOP('',(#17609,#17610,#17611,#17612));
#4710=EDGE_LOOP('',(#17613,#17614,#17615,#17616));
#4711=EDGE_LOOP('',(#17617,#17618,#17619,#17620));
#4712=EDGE_LOOP('',(#17621,#17622,#17623,#17624));
#4713=EDGE_LOOP('',(#17625,#17626,#17627,#17628));
#4714=EDGE_LOOP('',(#17629,#17630,#17631,#17632));
#4715=EDGE_LOOP('',(#17633,#17634,#17635,#17636));
#4716=EDGE_LOOP('',(#17637,#17638,#17639,#17640));
#4717=EDGE_LOOP('',(#17641,#17642,#17643,#17644));
#4718=EDGE_LOOP('',(#17645,#17646,#17647,#17648));
#4719=EDGE_LOOP('',(#17649,#17650,#17651,#17652));
#4720=EDGE_LOOP('',(#17653,#17654,#17655,#17656));
#4721=EDGE_LOOP('',(#17657,#17658,#17659,#17660,#17661,#17662,#17663,#17664));
#4722=EDGE_LOOP('',(#17665,#17666,#17667,#17668,#17669));
#4723=EDGE_LOOP('',(#17670,#17671,#17672,#17673));
#4724=EDGE_LOOP('',(#17674,#17675,#17676,#17677));
#4725=EDGE_LOOP('',(#17678,#17679,#17680,#17681));
#4726=EDGE_LOOP('',(#17682,#17683,#17684,#17685));
#4727=EDGE_LOOP('',(#17686,#17687,#17688,#17689));
#4728=EDGE_LOOP('',(#17690,#17691,#17692,#17693));
#4729=EDGE_LOOP('',(#17694,#17695,#17696,#17697));
#4730=EDGE_LOOP('',(#17698,#17699,#17700,#17701));
#4731=EDGE_LOOP('',(#17702,#17703,#17704,#17705));
#4732=EDGE_LOOP('',(#17706,#17707,#17708,#17709));
#4733=EDGE_LOOP('',(#17710,#17711,#17712,#17713));
#4734=EDGE_LOOP('',(#17714,#17715,#17716,#17717));
#4735=EDGE_LOOP('',(#17718,#17719,#17720,#17721));
#4736=EDGE_LOOP('',(#17722,#17723,#17724,#17725));
#4737=EDGE_LOOP('',(#17726,#17727,#17728,#17729));
#4738=EDGE_LOOP('',(#17730,#17731,#17732,#17733));
#4739=EDGE_LOOP('',(#17734,#17735,#17736,#17737));
#4740=EDGE_LOOP('',(#17738,#17739,#17740,#17741));
#4741=EDGE_LOOP('',(#17742,#17743,#17744,#17745));
#4742=EDGE_LOOP('',(#17746,#17747,#17748,#17749));
#4743=EDGE_LOOP('',(#17750,#17751,#17752,#17753));
#4744=EDGE_LOOP('',(#17754,#17755,#17756,#17757));
#4745=EDGE_LOOP('',(#17758,#17759,#17760,#17761));
#4746=EDGE_LOOP('',(#17762,#17763,#17764,#17765));
#4747=EDGE_LOOP('',(#17766,#17767,#17768,#17769));
#4748=EDGE_LOOP('',(#17770,#17771,#17772,#17773));
#4749=EDGE_LOOP('',(#17774,#17775,#17776,#17777));
#4750=EDGE_LOOP('',(#17778,#17779,#17780,#17781));
#4751=EDGE_LOOP('',(#17782,#17783,#17784,#17785));
#4752=EDGE_LOOP('',(#17786,#17787,#17788,#17789));
#4753=EDGE_LOOP('',(#17790,#17791,#17792,#17793));
#4754=EDGE_LOOP('',(#17794,#17795,#17796,#17797));
#4755=EDGE_LOOP('',(#17798,#17799,#17800,#17801));
#4756=EDGE_LOOP('',(#17802,#17803,#17804,#17805));
#4757=EDGE_LOOP('',(#17806,#17807,#17808,#17809));
#4758=EDGE_LOOP('',(#17810,#17811,#17812,#17813,#17814,#17815,#17816,#17817,
#17818,#17819,#17820,#17821,#17822,#17823,#17824,#17825,#17826,#17827,#17828,
#17829,#17830,#17831,#17832,#17833,#17834,#17835,#17836,#17837,#17838,#17839,
#17840,#17841,#17842,#17843,#17844));
#4759=EDGE_LOOP('',(#17845,#17846,#17847,#17848));
#4760=EDGE_LOOP('',(#17849,#17850,#17851,#17852));
#4761=EDGE_LOOP('',(#17853,#17854,#17855,#17856));
#4762=EDGE_LOOP('',(#17857,#17858,#17859,#17860));
#4763=EDGE_LOOP('',(#17861,#17862,#17863,#17864));
#4764=EDGE_LOOP('',(#17865,#17866,#17867,#17868));
#4765=EDGE_LOOP('',(#17869,#17870,#17871,#17872));
#4766=EDGE_LOOP('',(#17873,#17874,#17875,#17876));
#4767=EDGE_LOOP('',(#17877,#17878,#17879,#17880));
#4768=EDGE_LOOP('',(#17881,#17882,#17883,#17884));
#4769=EDGE_LOOP('',(#17885,#17886,#17887,#17888));
#4770=EDGE_LOOP('',(#17889,#17890,#17891,#17892));
#4771=EDGE_LOOP('',(#17893,#17894,#17895,#17896));
#4772=EDGE_LOOP('',(#17897,#17898,#17899,#17900));
#4773=EDGE_LOOP('',(#17901,#17902,#17903,#17904));
#4774=EDGE_LOOP('',(#17905,#17906,#17907,#17908));
#4775=EDGE_LOOP('',(#17909,#17910,#17911,#17912));
#4776=EDGE_LOOP('',(#17913,#17914,#17915,#17916));
#4777=EDGE_LOOP('',(#17917,#17918,#17919,#17920));
#4778=EDGE_LOOP('',(#17921,#17922,#17923,#17924));
#4779=EDGE_LOOP('',(#17925,#17926,#17927,#17928));
#4780=EDGE_LOOP('',(#17929,#17930,#17931,#17932));
#4781=EDGE_LOOP('',(#17933,#17934,#17935,#17936));
#4782=EDGE_LOOP('',(#17937,#17938,#17939,#17940));
#4783=EDGE_LOOP('',(#17941,#17942,#17943,#17944));
#4784=EDGE_LOOP('',(#17945,#17946,#17947,#17948));
#4785=EDGE_LOOP('',(#17949,#17950,#17951,#17952));
#4786=EDGE_LOOP('',(#17953,#17954,#17955,#17956));
#4787=EDGE_LOOP('',(#17957,#17958,#17959,#17960));
#4788=EDGE_LOOP('',(#17961,#17962,#17963,#17964));
#4789=EDGE_LOOP('',(#17965,#17966,#17967,#17968,#17969,#17970,#17971,#17972,
#17973,#17974,#17975,#17976,#17977,#17978,#17979,#17980,#17981,#17982,#17983,
#17984,#17985,#17986,#17987,#17988,#17989,#17990,#17991,#17992,#17993,#17994));
#4790=EDGE_LOOP('',(#17995,#17996,#17997,#17998));
#4791=EDGE_LOOP('',(#17999,#18000,#18001,#18002));
#4792=EDGE_LOOP('',(#18003,#18004,#18005,#18006));
#4793=EDGE_LOOP('',(#18007,#18008,#18009,#18010));
#4794=EDGE_LOOP('',(#18011,#18012,#18013,#18014));
#4795=EDGE_LOOP('',(#18015,#18016,#18017,#18018));
#4796=EDGE_LOOP('',(#18019,#18020,#18021,#18022));
#4797=EDGE_LOOP('',(#18023,#18024,#18025,#18026));
#4798=EDGE_LOOP('',(#18027,#18028,#18029,#18030));
#4799=EDGE_LOOP('',(#18031,#18032,#18033,#18034));
#4800=EDGE_LOOP('',(#18035,#18036,#18037,#18038));
#4801=EDGE_LOOP('',(#18039,#18040,#18041,#18042));
#4802=EDGE_LOOP('',(#18043,#18044,#18045,#18046));
#4803=EDGE_LOOP('',(#18047,#18048,#18049,#18050));
#4804=EDGE_LOOP('',(#18051,#18052,#18053,#18054));
#4805=EDGE_LOOP('',(#18055,#18056,#18057,#18058));
#4806=EDGE_LOOP('',(#18059,#18060,#18061,#18062));
#4807=EDGE_LOOP('',(#18063,#18064,#18065,#18066));
#4808=EDGE_LOOP('',(#18067,#18068,#18069,#18070));
#4809=EDGE_LOOP('',(#18071,#18072,#18073,#18074));
#4810=EDGE_LOOP('',(#18075,#18076,#18077,#18078));
#4811=EDGE_LOOP('',(#18079,#18080,#18081,#18082));
#4812=EDGE_LOOP('',(#18083,#18084,#18085,#18086,#18087,#18088,#18089,#18090,
#18091,#18092,#18093,#18094,#18095,#18096,#18097,#18098,#18099,#18100,#18101,
#18102,#18103,#18104));
#4813=EDGE_LOOP('',(#18105,#18106,#18107,#18108));
#4814=EDGE_LOOP('',(#18109,#18110,#18111,#18112));
#4815=EDGE_LOOP('',(#18113,#18114,#18115,#18116));
#4816=EDGE_LOOP('',(#18117,#18118,#18119,#18120));
#4817=EDGE_LOOP('',(#18121,#18122,#18123,#18124));
#4818=EDGE_LOOP('',(#18125,#18126,#18127,#18128));
#4819=EDGE_LOOP('',(#18129,#18130,#18131,#18132));
#4820=EDGE_LOOP('',(#18133,#18134,#18135,#18136));
#4821=EDGE_LOOP('',(#18137,#18138,#18139,#18140));
#4822=EDGE_LOOP('',(#18141,#18142,#18143,#18144));
#4823=EDGE_LOOP('',(#18145,#18146,#18147,#18148));
#4824=EDGE_LOOP('',(#18149,#18150,#18151,#18152));
#4825=EDGE_LOOP('',(#18153,#18154,#18155,#18156));
#4826=EDGE_LOOP('',(#18157,#18158,#18159,#18160));
#4827=EDGE_LOOP('',(#18161,#18162,#18163,#18164));
#4828=EDGE_LOOP('',(#18165,#18166,#18167,#18168));
#4829=EDGE_LOOP('',(#18169,#18170,#18171,#18172));
#4830=EDGE_LOOP('',(#18173,#18174,#18175,#18176));
#4831=EDGE_LOOP('',(#18177,#18178,#18179,#18180));
#4832=EDGE_LOOP('',(#18181,#18182,#18183,#18184,#18185,#18186,#18187,#18188,
#18189,#18190,#18191));
#4833=EDGE_LOOP('',(#18192,#18193,#18194,#18195,#18196,#18197,#18198,#18199));
#4834=EDGE_LOOP('',(#18200,#18201,#18202,#18203));
#4835=EDGE_LOOP('',(#18204,#18205,#18206,#18207));
#4836=EDGE_LOOP('',(#18208,#18209,#18210,#18211));
#4837=EDGE_LOOP('',(#18212,#18213,#18214,#18215));
#4838=EDGE_LOOP('',(#18216,#18217,#18218,#18219));
#4839=EDGE_LOOP('',(#18220,#18221,#18222,#18223));
#4840=EDGE_LOOP('',(#18224,#18225,#18226,#18227));
#4841=EDGE_LOOP('',(#18228,#18229,#18230,#18231));
#4842=EDGE_LOOP('',(#18232,#18233,#18234,#18235));
#4843=EDGE_LOOP('',(#18236,#18237,#18238,#18239));
#4844=EDGE_LOOP('',(#18240,#18241,#18242,#18243));
#4845=EDGE_LOOP('',(#18244,#18245,#18246,#18247));
#4846=EDGE_LOOP('',(#18248,#18249,#18250,#18251));
#4847=EDGE_LOOP('',(#18252,#18253,#18254,#18255));
#4848=EDGE_LOOP('',(#18256,#18257,#18258,#18259));
#4849=EDGE_LOOP('',(#18260,#18261,#18262,#18263));
#4850=EDGE_LOOP('',(#18264,#18265,#18266,#18267));
#4851=EDGE_LOOP('',(#18268,#18269,#18270,#18271));
#4852=EDGE_LOOP('',(#18272,#18273,#18274,#18275));
#4853=EDGE_LOOP('',(#18276,#18277,#18278,#18279));
#4854=EDGE_LOOP('',(#18280,#18281,#18282,#18283));
#4855=EDGE_LOOP('',(#18284,#18285,#18286,#18287));
#4856=EDGE_LOOP('',(#18288,#18289,#18290,#18291));
#4857=EDGE_LOOP('',(#18292,#18293,#18294,#18295));
#4858=EDGE_LOOP('',(#18296,#18297,#18298,#18299));
#4859=EDGE_LOOP('',(#18300,#18301,#18302,#18303));
#4860=EDGE_LOOP('',(#18304,#18305,#18306,#18307));
#4861=EDGE_LOOP('',(#18308,#18309,#18310,#18311));
#4862=EDGE_LOOP('',(#18312,#18313,#18314,#18315,#18316,#18317,#18318,#18319,
#18320,#18321,#18322,#18323,#18324,#18325,#18326,#18327,#18328,#18329,#18330));
#4863=EDGE_LOOP('',(#18331,#18332,#18333,#18334,#18335,#18336,#18337,#18338,
#18339));
#4864=EDGE_LOOP('',(#18340,#18341,#18342,#18343));
#4865=EDGE_LOOP('',(#18344,#18345,#18346,#18347));
#4866=EDGE_LOOP('',(#18348,#18349,#18350,#18351));
#4867=EDGE_LOOP('',(#18352,#18353,#18354,#18355));
#4868=EDGE_LOOP('',(#18356,#18357,#18358,#18359));
#4869=EDGE_LOOP('',(#18360,#18361,#18362,#18363));
#4870=EDGE_LOOP('',(#18364,#18365,#18366,#18367));
#4871=EDGE_LOOP('',(#18368,#18369,#18370,#18371));
#4872=EDGE_LOOP('',(#18372,#18373,#18374,#18375));
#4873=EDGE_LOOP('',(#18376,#18377,#18378,#18379));
#4874=EDGE_LOOP('',(#18380,#18381,#18382,#18383));
#4875=EDGE_LOOP('',(#18384,#18385,#18386,#18387));
#4876=EDGE_LOOP('',(#18388,#18389,#18390,#18391));
#4877=EDGE_LOOP('',(#18392,#18393,#18394,#18395));
#4878=EDGE_LOOP('',(#18396,#18397,#18398,#18399));
#4879=EDGE_LOOP('',(#18400,#18401,#18402,#18403));
#4880=EDGE_LOOP('',(#18404,#18405,#18406,#18407));
#4881=EDGE_LOOP('',(#18408,#18409,#18410,#18411));
#4882=EDGE_LOOP('',(#18412,#18413,#18414,#18415));
#4883=EDGE_LOOP('',(#18416,#18417,#18418,#18419));
#4884=EDGE_LOOP('',(#18420,#18421,#18422,#18423));
#4885=EDGE_LOOP('',(#18424,#18425,#18426,#18427,#18428,#18429,#18430,#18431,
#18432,#18433,#18434,#18435,#18436));
#4886=EDGE_LOOP('',(#18437,#18438,#18439,#18440,#18441,#18442,#18443,#18444));
#4887=EDGE_LOOP('',(#18445,#18446,#18447,#18448));
#4888=EDGE_LOOP('',(#18449,#18450,#18451,#18452));
#4889=EDGE_LOOP('',(#18453,#18454,#18455,#18456));
#4890=EDGE_LOOP('',(#18457,#18458,#18459,#18460));
#4891=EDGE_LOOP('',(#18461,#18462,#18463,#18464));
#4892=EDGE_LOOP('',(#18465,#18466,#18467,#18468));
#4893=EDGE_LOOP('',(#18469,#18470,#18471,#18472));
#4894=EDGE_LOOP('',(#18473,#18474,#18475,#18476));
#4895=EDGE_LOOP('',(#18477,#18478,#18479,#18480));
#4896=EDGE_LOOP('',(#18481,#18482,#18483,#18484));
#4897=EDGE_LOOP('',(#18485,#18486,#18487,#18488));
#4898=EDGE_LOOP('',(#18489,#18490,#18491,#18492));
#4899=EDGE_LOOP('',(#18493,#18494,#18495,#18496));
#4900=EDGE_LOOP('',(#18497,#18498,#18499,#18500,#18501,#18502,#18503,#18504,
#18505,#18506,#18507,#18508,#18509));
#4901=EDGE_LOOP('',(#18510,#18511,#18512,#18513,#18514,#18515,#18516,#18517));
#4902=EDGE_LOOP('',(#18518,#18519,#18520,#18521,#18522,#18523,#18524,#18525,
#18526));
#4903=EDGE_LOOP('',(#18527,#18528,#18529,#18530,#18531,#18532,#18533,#18534));
#4904=EDGE_LOOP('',(#18535,#18536,#18537,#18538,#18539));
#4905=EDGE_LOOP('',(#18540,#18541,#18542,#18543,#18544,#18545,#18546,#18547));
#4906=EDGE_LOOP('',(#18548,#18549,#18550,#18551,#18552,#18553,#18554,#18555,
#18556,#18557));
#4907=EDGE_LOOP('',(#18558,#18559,#18560,#18561,#18562,#18563,#18564));
#4908=EDGE_LOOP('',(#18565,#18566,#18567,#18568));
#4909=EDGE_LOOP('',(#18569,#18570,#18571,#18572));
#4910=EDGE_LOOP('',(#18573,#18574,#18575,#18576));
#4911=EDGE_LOOP('',(#18577));
#4912=EDGE_LOOP('',(#18578,#18579,#18580));
#4913=EDGE_LOOP('',(#18581,#18582,#18583,#18584,#18585,#18586,#18587,#18588,
#18589,#18590));
#4914=EDGE_LOOP('',(#18591));
#4915=EDGE_LOOP('',(#18592));
#4916=EDGE_LOOP('',(#18593,#18594));
#4917=EDGE_LOOP('',(#18595,#18596,#18597,#18598,#18599,#18600,#18601,#18602));
#4918=EDGE_LOOP('',(#18603,#18604,#18605,#18606,#18607,#18608));
#4919=EDGE_LOOP('',(#18609,#18610,#18611,#18612));
#4920=EDGE_LOOP('',(#18613));
#4921=EDGE_LOOP('',(#18614));
#4922=EDGE_LOOP('',(#18615));
#4923=EDGE_LOOP('',(#18616));
#4924=EDGE_LOOP('',(#18617));
#4925=EDGE_LOOP('',(#18618));
#4926=EDGE_LOOP('',(#18619));
#4927=EDGE_LOOP('',(#18620));
#4928=EDGE_LOOP('',(#18621));
#4929=EDGE_LOOP('',(#18622,#18623,#18624,#18625));
#4930=EDGE_LOOP('',(#18626,#18627,#18628,#18629));
#4931=EDGE_LOOP('',(#18630,#18631,#18632,#18633));
#4932=EDGE_LOOP('',(#18634,#18635,#18636,#18637));
#4933=EDGE_LOOP('',(#18638,#18639,#18640,#18641));
#4934=EDGE_LOOP('',(#18642,#18643,#18644,#18645));
#4935=EDGE_LOOP('',(#18646,#18647,#18648,#18649));
#4936=EDGE_LOOP('',(#18650,#18651,#18652,#18653));
#4937=EDGE_LOOP('',(#18654,#18655,#18656,#18657));
#4938=EDGE_LOOP('',(#18658,#18659,#18660,#18661));
#4939=EDGE_LOOP('',(#18662,#18663,#18664,#18665));
#4940=EDGE_LOOP('',(#18666,#18667,#18668));
#4941=EDGE_LOOP('',(#18669,#18670,#18671));
#4942=EDGE_LOOP('',(#18672,#18673,#18674));
#4943=EDGE_LOOP('',(#18675,#18676,#18677));
#4944=EDGE_LOOP('',(#18678,#18679,#18680));
#4945=EDGE_LOOP('',(#18681,#18682,#18683));
#4946=EDGE_LOOP('',(#18684,#18685,#18686,#18687,#18688));
#4947=EDGE_LOOP('',(#18689,#18690,#18691,#18692,#18693));
#4948=EDGE_LOOP('',(#18694));
#4949=EDGE_LOOP('',(#18695,#18696,#18697,#18698,#18699,#18700,#18701,#18702,
#18703,#18704,#18705,#18706,#18707));
#4950=EDGE_LOOP('',(#18708,#18709,#18710,#18711,#18712,#18713,#18714,#18715,
#18716,#18717,#18718,#18719,#18720));
#4951=EDGE_LOOP('',(#18721,#18722,#18723,#18724,#18725,#18726,#18727,#18728,
#18729,#18730,#18731,#18732,#18733,#18734,#18735,#18736,#18737,#18738,#18739));
#4952=EDGE_LOOP('',(#18740,#18741,#18742,#18743,#18744,#18745,#18746,#18747,
#18748,#18749,#18750));
#4953=EDGE_LOOP('',(#18751,#18752,#18753,#18754,#18755,#18756,#18757,#18758,
#18759,#18760,#18761,#18762,#18763,#18764,#18765,#18766,#18767,#18768,#18769,
#18770,#18771,#18772));
#4954=EDGE_LOOP('',(#18773,#18774,#18775,#18776,#18777,#18778,#18779,#18780,
#18781,#18782,#18783,#18784,#18785,#18786,#18787,#18788,#18789,#18790,#18791,
#18792,#18793,#18794,#18795,#18796,#18797,#18798,#18799,#18800,#18801,#18802));
#4955=EDGE_LOOP('',(#18803,#18804,#18805,#18806,#18807,#18808,#18809,#18810,
#18811,#18812,#18813,#18814,#18815,#18816,#18817,#18818,#18819,#18820,#18821,
#18822,#18823,#18824,#18825,#18826,#18827,#18828,#18829,#18830,#18831,#18832,
#18833,#18834,#18835,#18836,#18837));
#4956=EDGE_LOOP('',(#18838,#18839,#18840,#18841,#18842,#18843,#18844,#18845));
#4957=EDGE_LOOP('',(#18846,#18847,#18848,#18849));
#4958=EDGE_LOOP('',(#18850,#18851,#18852,#18853,#18854,#18855,#18856,#18857,
#18858,#18859,#18860,#18861,#18862,#18863,#18864,#18865,#18866,#18867,#18868,
#18869,#18870,#18871,#18872,#18873,#18874,#18875,#18876,#18877,#18878,#18879));
#4959=EDGE_LOOP('',(#18880,#18881,#18882,#18883,#18884,#18885,#18886,#18887,
#18888,#18889,#18890,#18891,#18892,#18893,#18894));
#4960=EDGE_LOOP('',(#18895,#18896,#18897,#18898,#18899,#18900,#18901,#18902,
#18903));
#4961=EDGE_LOOP('',(#18904,#18905,#18906,#18907,#18908,#18909,#18910,#18911,
#18912,#18913,#18914,#18915));
#4962=EDGE_LOOP('',(#18916,#18917,#18918,#18919,#18920,#18921,#18922,#18923,
#18924,#18925,#18926,#18927,#18928,#18929,#18930,#18931,#18932,#18933,#18934,
#18935,#18936,#18937,#18938,#18939,#18940,#18941,#18942));
#4963=EDGE_LOOP('',(#18943,#18944,#18945,#18946));
#4964=EDGE_LOOP('',(#18947));
#4965=EDGE_LOOP('',(#18948,#18949,#18950,#18951));
#4966=EDGE_LOOP('',(#18952));
#4967=EDGE_LOOP('',(#18953));
#4968=EDGE_LOOP('',(#18954));
#4969=EDGE_LOOP('',(#18955));
#4970=EDGE_LOOP('',(#18956,#18957,#18958,#18959));
#4971=EDGE_LOOP('',(#18960));
#4972=EDGE_LOOP('',(#18961));
#4973=EDGE_LOOP('',(#18962,#18963,#18964,#18965));
#4974=EDGE_LOOP('',(#18966));
#4975=EDGE_LOOP('',(#18967));
#4976=EDGE_LOOP('',(#18968,#18969,#18970,#18971));
#4977=EDGE_LOOP('',(#18972));
#4978=EDGE_LOOP('',(#18973));
#4979=EDGE_LOOP('',(#18974,#18975,#18976,#18977));
#4980=EDGE_LOOP('',(#18978,#18979,#18980,#18981));
#4981=EDGE_LOOP('',(#18982,#18983,#18984,#18985));
#4982=EDGE_LOOP('',(#18986,#18987,#18988,#18989));
#4983=EDGE_LOOP('',(#18990,#18991,#18992,#18993));
#4984=EDGE_LOOP('',(#18994,#18995,#18996,#18997));
#4985=EDGE_LOOP('',(#18998));
#4986=EDGE_LOOP('',(#18999));
#4987=EDGE_LOOP('',(#19000,#19001,#19002,#19003));
#4988=EDGE_LOOP('',(#19004,#19005,#19006,#19007));
#4989=EDGE_LOOP('',(#19008,#19009,#19010,#19011));
#4990=EDGE_LOOP('',(#19012,#19013,#19014,#19015));
#4991=EDGE_LOOP('',(#19016,#19017,#19018,#19019));
#4992=EDGE_LOOP('',(#19020,#19021,#19022,#19023));
#4993=EDGE_LOOP('',(#19024));
#4994=EDGE_LOOP('',(#19025));
#4995=EDGE_LOOP('',(#19026));
#4996=EDGE_LOOP('',(#19027));
#4997=EDGE_LOOP('',(#19028,#19029,#19030,#19031));
#4998=EDGE_LOOP('',(#19032,#19033,#19034,#19035));
#4999=EDGE_LOOP('',(#19036));
#5000=EDGE_LOOP('',(#19037));
#5001=EDGE_LOOP('',(#19038,#19039,#19040,#19041));
#5002=EDGE_LOOP('',(#19042));
#5003=EDGE_LOOP('',(#19043));
#5004=EDGE_LOOP('',(#19044,#19045,#19046,#19047));
#5005=EDGE_LOOP('',(#19048,#19049,#19050,#19051));
#5006=EDGE_LOOP('',(#19052,#19053,#19054,#19055));
#5007=EDGE_LOOP('',(#19056));
#5008=EDGE_LOOP('',(#19057));
#5009=EDGE_LOOP('',(#19058,#19059,#19060,#19061));
#5010=EDGE_LOOP('',(#19062,#19063,#19064,#19065));
#5011=EDGE_LOOP('',(#19066));
#5012=EDGE_LOOP('',(#19067));
#5013=EDGE_LOOP('',(#19068,#19069,#19070,#19071));
#5014=EDGE_LOOP('',(#19072,#19073,#19074,#19075));
#5015=EDGE_LOOP('',(#19076,#19077,#19078,#19079));
#5016=EDGE_LOOP('',(#19080,#19081,#19082,#19083));
#5017=EDGE_LOOP('',(#19084,#19085,#19086,#19087));
#5018=EDGE_LOOP('',(#19088,#19089,#19090,#19091));
#5019=EDGE_LOOP('',(#19092,#19093,#19094,#19095));
#5020=EDGE_LOOP('',(#19096,#19097,#19098,#19099));
#5021=EDGE_LOOP('',(#19100,#19101,#19102,#19103));
#5022=EDGE_LOOP('',(#19104,#19105,#19106,#19107));
#5023=EDGE_LOOP('',(#19108,#19109,#19110,#19111));
#5024=EDGE_LOOP('',(#19112,#19113,#19114,#19115));
#5025=EDGE_LOOP('',(#19116,#19117,#19118,#19119));
#5026=EDGE_LOOP('',(#19120,#19121,#19122,#19123));
#5027=EDGE_LOOP('',(#19124,#19125,#19126,#19127));
#5028=EDGE_LOOP('',(#19128,#19129,#19130,#19131));
#5029=EDGE_LOOP('',(#19132,#19133,#19134,#19135));
#5030=EDGE_LOOP('',(#19136,#19137,#19138,#19139));
#5031=EDGE_LOOP('',(#19140,#19141,#19142,#19143));
#5032=EDGE_LOOP('',(#19144,#19145,#19146,#19147));
#5033=EDGE_LOOP('',(#19148,#19149,#19150,#19151));
#5034=EDGE_LOOP('',(#19152,#19153,#19154,#19155));
#5035=EDGE_LOOP('',(#19156,#19157,#19158,#19159));
#5036=EDGE_LOOP('',(#19160,#19161,#19162,#19163));
#5037=EDGE_LOOP('',(#19164,#19165,#19166,#19167));
#5038=EDGE_LOOP('',(#19168,#19169,#19170,#19171));
#5039=EDGE_LOOP('',(#19172,#19173,#19174,#19175));
#5040=EDGE_LOOP('',(#19176,#19177,#19178,#19179));
#5041=EDGE_LOOP('',(#19180,#19181,#19182,#19183));
#5042=EDGE_LOOP('',(#19184,#19185,#19186,#19187));
#5043=EDGE_LOOP('',(#19188,#19189,#19190,#19191));
#5044=EDGE_LOOP('',(#19192,#19193,#19194,#19195));
#5045=EDGE_LOOP('',(#19196,#19197,#19198,#19199));
#5046=EDGE_LOOP('',(#19200,#19201,#19202,#19203));
#5047=EDGE_LOOP('',(#19204,#19205,#19206,#19207));
#5048=EDGE_LOOP('',(#19208,#19209,#19210,#19211));
#5049=EDGE_LOOP('',(#19212,#19213,#19214,#19215));
#5050=EDGE_LOOP('',(#19216,#19217,#19218,#19219));
#5051=EDGE_LOOP('',(#19220,#19221));
#5052=EDGE_LOOP('',(#19222,#19223,#19224,#19225));
#5053=EDGE_LOOP('',(#19226,#19227,#19228,#19229));
#5054=EDGE_LOOP('',(#19230,#19231,#19232,#19233,#19234));
#5055=EDGE_LOOP('',(#19235,#19236));
#5056=EDGE_LOOP('',(#19237,#19238));
#5057=EDGE_LOOP('',(#19239,#19240,#19241,#19242));
#5058=EDGE_LOOP('',(#19243,#19244,#19245,#19246));
#5059=EDGE_LOOP('',(#19247,#19248,#19249,#19250,#19251));
#5060=EDGE_LOOP('',(#19252,#19253));
#5061=EDGE_LOOP('',(#19254,#19255));
#5062=EDGE_LOOP('',(#19256,#19257,#19258,#19259));
#5063=EDGE_LOOP('',(#19260,#19261,#19262,#19263));
#5064=EDGE_LOOP('',(#19264,#19265,#19266,#19267,#19268));
#5065=EDGE_LOOP('',(#19269,#19270));
#5066=EDGE_LOOP('',(#19271,#19272));
#5067=EDGE_LOOP('',(#19273,#19274,#19275,#19276));
#5068=EDGE_LOOP('',(#19277,#19278,#19279,#19280));
#5069=EDGE_LOOP('',(#19281,#19282,#19283,#19284,#19285));
#5070=EDGE_LOOP('',(#19286,#19287));
#5071=EDGE_LOOP('',(#19288,#19289));
#5072=EDGE_LOOP('',(#19290,#19291,#19292,#19293));
#5073=EDGE_LOOP('',(#19294,#19295,#19296,#19297));
#5074=EDGE_LOOP('',(#19298,#19299,#19300,#19301,#19302));
#5075=EDGE_LOOP('',(#19303,#19304));
#5076=EDGE_LOOP('',(#19305,#19306));
#5077=EDGE_LOOP('',(#19307,#19308,#19309,#19310));
#5078=EDGE_LOOP('',(#19311,#19312,#19313,#19314));
#5079=EDGE_LOOP('',(#19315,#19316,#19317,#19318,#19319));
#5080=EDGE_LOOP('',(#19320,#19321));
#5081=EDGE_LOOP('',(#19322,#19323));
#5082=EDGE_LOOP('',(#19324,#19325,#19326,#19327));
#5083=EDGE_LOOP('',(#19328,#19329,#19330,#19331));
#5084=EDGE_LOOP('',(#19332,#19333,#19334,#19335,#19336));
#5085=EDGE_LOOP('',(#19337,#19338));
#5086=EDGE_LOOP('',(#19339,#19340));
#5087=EDGE_LOOP('',(#19341,#19342,#19343,#19344));
#5088=EDGE_LOOP('',(#19345,#19346,#19347,#19348));
#5089=EDGE_LOOP('',(#19349,#19350,#19351,#19352,#19353));
#5090=EDGE_LOOP('',(#19354,#19355));
#5091=EDGE_LOOP('',(#19356,#19357));
#5092=EDGE_LOOP('',(#19358,#19359,#19360,#19361));
#5093=EDGE_LOOP('',(#19362,#19363,#19364,#19365));
#5094=EDGE_LOOP('',(#19366,#19367,#19368,#19369,#19370));
#5095=EDGE_LOOP('',(#19371,#19372));
#5096=EDGE_LOOP('',(#19373,#19374));
#5097=EDGE_LOOP('',(#19375,#19376,#19377,#19378));
#5098=EDGE_LOOP('',(#19379,#19380,#19381,#19382));
#5099=EDGE_LOOP('',(#19383,#19384,#19385,#19386,#19387));
#5100=EDGE_LOOP('',(#19388,#19389));
#5101=EDGE_LOOP('',(#19390,#19391));
#5102=EDGE_LOOP('',(#19392,#19393,#19394,#19395));
#5103=EDGE_LOOP('',(#19396,#19397,#19398,#19399));
#5104=EDGE_LOOP('',(#19400,#19401,#19402,#19403,#19404));
#5105=EDGE_LOOP('',(#19405,#19406));
#5106=EDGE_LOOP('',(#19407,#19408));
#5107=EDGE_LOOP('',(#19409,#19410,#19411,#19412));
#5108=EDGE_LOOP('',(#19413,#19414,#19415,#19416));
#5109=EDGE_LOOP('',(#19417,#19418,#19419,#19420,#19421));
#5110=EDGE_LOOP('',(#19422,#19423));
#5111=EDGE_LOOP('',(#19424,#19425));
#5112=EDGE_LOOP('',(#19426,#19427,#19428,#19429));
#5113=EDGE_LOOP('',(#19430,#19431,#19432,#19433));
#5114=EDGE_LOOP('',(#19434,#19435,#19436,#19437,#19438));
#5115=EDGE_LOOP('',(#19439,#19440));
#5116=EDGE_LOOP('',(#19441,#19442));
#5117=EDGE_LOOP('',(#19443,#19444,#19445,#19446));
#5118=EDGE_LOOP('',(#19447,#19448,#19449,#19450));
#5119=EDGE_LOOP('',(#19451,#19452,#19453,#19454,#19455));
#5120=EDGE_LOOP('',(#19456,#19457));
#5121=EDGE_LOOP('',(#19458,#19459));
#5122=EDGE_LOOP('',(#19460,#19461,#19462,#19463));
#5123=EDGE_LOOP('',(#19464,#19465,#19466,#19467));
#5124=EDGE_LOOP('',(#19468,#19469,#19470,#19471,#19472));
#5125=EDGE_LOOP('',(#19473,#19474));
#5126=EDGE_LOOP('',(#19475,#19476));
#5127=EDGE_LOOP('',(#19477,#19478,#19479,#19480));
#5128=EDGE_LOOP('',(#19481,#19482,#19483,#19484));
#5129=EDGE_LOOP('',(#19485,#19486,#19487,#19488,#19489));
#5130=EDGE_LOOP('',(#19490,#19491));
#5131=EDGE_LOOP('',(#19492,#19493));
#5132=EDGE_LOOP('',(#19494,#19495));
#5133=EDGE_LOOP('',(#19496,#19497,#19498,#19499));
#5134=EDGE_LOOP('',(#19500,#19501,#19502,#19503));
#5135=EDGE_LOOP('',(#19504,#19505,#19506,#19507,#19508));
#5136=EDGE_LOOP('',(#19509,#19510,#19511,#19512));
#5137=EDGE_LOOP('',(#19513,#19514,#19515,#19516,#19517));
#5138=EDGE_LOOP('',(#19518,#19519,#19520,#19521,#19522,#19523,#19524,#19525,
#19526,#19527,#19528,#19529,#19530,#19531,#19532,#19533,#19534,#19535,#19536,
#19537,#19538,#19539,#19540,#19541,#19542,#19543,#19544,#19545,#19546,#19547,
#19548,#19549,#19550,#19551,#19552,#19553,#19554,#19555,#19556,#19557,#19558,
#19559,#19560,#19561,#19562,#19563,#19564,#19565,#19566,#19567,#19568,#19569,
#19570,#19571,#19572,#19573,#19574,#19575,#19576,#19577,#19578,#19579,#19580,
#19581,#19582,#19583,#19584,#19585,#19586,#19587,#19588,#19589));
#5139=EDGE_LOOP('',(#19590,#19591,#19592,#19593));
#5140=EDGE_LOOP('',(#19594,#19595,#19596,#19597,#19598));
#5141=EDGE_LOOP('',(#19599,#19600,#19601,#19602));
#5142=EDGE_LOOP('',(#19603,#19604,#19605,#19606,#19607));
#5143=EDGE_LOOP('',(#19608,#19609,#19610,#19611));
#5144=EDGE_LOOP('',(#19612,#19613,#19614,#19615,#19616));
#5145=EDGE_LOOP('',(#19617,#19618,#19619,#19620));
#5146=EDGE_LOOP('',(#19621,#19622,#19623,#19624,#19625));
#5147=EDGE_LOOP('',(#19626,#19627,#19628,#19629));
#5148=EDGE_LOOP('',(#19630,#19631,#19632,#19633,#19634));
#5149=EDGE_LOOP('',(#19635,#19636,#19637,#19638));
#5150=EDGE_LOOP('',(#19639,#19640,#19641,#19642,#19643));
#5151=EDGE_LOOP('',(#19644,#19645,#19646,#19647));
#5152=EDGE_LOOP('',(#19648,#19649,#19650,#19651,#19652));
#5153=EDGE_LOOP('',(#19653,#19654,#19655,#19656));
#5154=EDGE_LOOP('',(#19657,#19658,#19659,#19660,#19661));
#5155=EDGE_LOOP('',(#19662,#19663,#19664,#19665));
#5156=EDGE_LOOP('',(#19666,#19667,#19668,#19669,#19670));
#5157=EDGE_LOOP('',(#19671,#19672,#19673,#19674));
#5158=EDGE_LOOP('',(#19675,#19676,#19677,#19678,#19679));
#5159=EDGE_LOOP('',(#19680,#19681,#19682,#19683));
#5160=EDGE_LOOP('',(#19684,#19685,#19686,#19687,#19688));
#5161=EDGE_LOOP('',(#19689,#19690,#19691,#19692));
#5162=EDGE_LOOP('',(#19693,#19694,#19695,#19696,#19697));
#5163=EDGE_LOOP('',(#19698,#19699,#19700,#19701));
#5164=EDGE_LOOP('',(#19702,#19703,#19704,#19705,#19706));
#5165=EDGE_LOOP('',(#19707,#19708,#19709,#19710));
#5166=EDGE_LOOP('',(#19711,#19712,#19713,#19714,#19715));
#5167=EDGE_LOOP('',(#19716,#19717,#19718,#19719));
#5168=EDGE_LOOP('',(#19720,#19721,#19722,#19723,#19724));
#5169=EDGE_LOOP('',(#19725,#19726,#19727,#19728,#19729));
#5170=EDGE_LOOP('',(#19730,#19731,#19732,#19733));
#5171=EDGE_LOOP('',(#19734,#19735,#19736,#19737));
#5172=EDGE_LOOP('',(#19738));
#5173=EDGE_LOOP('',(#19739));
#5174=EDGE_LOOP('',(#19740,#19741,#19742,#19743));
#5175=EDGE_LOOP('',(#19744,#19745,#19746,#19747));
#5176=EDGE_LOOP('',(#19748));
#5177=EDGE_LOOP('',(#19749,#19750,#19751,#19752,#19753,#19754,#19755,#19756,
#19757,#19758,#19759,#19760,#19761,#19762,#19763,#19764,#19765,#19766,#19767,
#19768,#19769,#19770,#19771,#19772,#19773,#19774,#19775,#19776,#19777,#19778,
#19779,#19780,#19781,#19782,#19783,#19784,#19785,#19786,#19787,#19788,#19789,
#19790,#19791,#19792,#19793,#19794,#19795,#19796,#19797,#19798,#19799,#19800,
#19801,#19802,#19803,#19804,#19805,#19806,#19807,#19808,#19809,#19810,#19811,
#19812,#19813,#19814,#19815,#19816,#19817));
#5178=EDGE_LOOP('',(#19818));
#5179=EDGE_LOOP('',(#19819));
#5180=EDGE_LOOP('',(#19820,#19821,#19822,#19823));
#5181=EDGE_LOOP('',(#19824));
#5182=EDGE_LOOP('',(#19825));
#5183=EDGE_LOOP('',(#19826,#19827,#19828,#19829));
#5184=EDGE_LOOP('',(#19830,#19831,#19832,#19833));
#5185=EDGE_LOOP('',(#19834,#19835,#19836,#19837));
#5186=EDGE_LOOP('',(#19838));
#5187=EDGE_LOOP('',(#19839));
#5188=EDGE_LOOP('',(#19840,#19841,#19842,#19843));
#5189=EDGE_LOOP('',(#19844,#19845,#19846,#19847));
#5190=EDGE_LOOP('',(#19848,#19849,#19850,#19851));
#5191=EDGE_LOOP('',(#19852));
#5192=EDGE_LOOP('',(#19853));
#5193=EDGE_LOOP('',(#19854,#19855,#19856,#19857));
#5194=EDGE_LOOP('',(#19858,#19859,#19860,#19861));
#5195=EDGE_LOOP('',(#19862,#19863,#19864,#19865));
#5196=EDGE_LOOP('',(#19866,#19867,#19868,#19869));
#5197=EDGE_LOOP('',(#19870,#19871,#19872,#19873));
#5198=EDGE_LOOP('',(#19874,#19875,#19876,#19877));
#5199=EDGE_LOOP('',(#19878,#19879,#19880,#19881));
#5200=EDGE_LOOP('',(#19882,#19883,#19884,#19885));
#5201=EDGE_LOOP('',(#19886,#19887,#19888,#19889));
#5202=EDGE_LOOP('',(#19890,#19891,#19892,#19893));
#5203=EDGE_LOOP('',(#19894,#19895,#19896,#19897));
#5204=EDGE_LOOP('',(#19898,#19899,#19900,#19901));
#5205=EDGE_LOOP('',(#19902,#19903,#19904,#19905,#19906,#19907,#19908,#19909));
#5206=EDGE_LOOP('',(#19910));
#5207=EDGE_LOOP('',(#19911));
#5208=EDGE_LOOP('',(#19912,#19913,#19914,#19915,#19916,#19917,#19918,#19919));
#5209=EDGE_LOOP('',(#19920));
#5210=EDGE_LOOP('',(#19921));
#5211=EDGE_LOOP('',(#19922,#19923,#19924,#19925,#19926,#19927,#19928,#19929));
#5212=EDGE_LOOP('',(#19930,#19931,#19932,#19933));
#5213=EDGE_LOOP('',(#19934,#19935,#19936,#19937));
#5214=EDGE_LOOP('',(#19938,#19939,#19940,#19941));
#5215=EDGE_LOOP('',(#19942,#19943,#19944,#19945));
#5216=EDGE_LOOP('',(#19946,#19947,#19948,#19949));
#5217=EDGE_LOOP('',(#19950,#19951,#19952,#19953));
#5218=EDGE_LOOP('',(#19954,#19955,#19956,#19957));
#5219=EDGE_LOOP('',(#19958,#19959,#19960,#19961));
#5220=EDGE_LOOP('',(#19962,#19963,#19964,#19965));
#5221=EDGE_LOOP('',(#19966,#19967,#19968,#19969));
#5222=EDGE_LOOP('',(#19970,#19971,#19972,#19973));
#5223=EDGE_LOOP('',(#19974,#19975,#19976,#19977));
#5224=EDGE_LOOP('',(#19978,#19979,#19980,#19981));
#5225=EDGE_LOOP('',(#19982,#19983,#19984,#19985));
#5226=EDGE_LOOP('',(#19986,#19987,#19988,#19989));
#5227=EDGE_LOOP('',(#19990,#19991,#19992,#19993));
#5228=EDGE_LOOP('',(#19994,#19995,#19996,#19997));
#5229=EDGE_LOOP('',(#19998,#19999,#20000,#20001));
#5230=EDGE_LOOP('',(#20002,#20003,#20004,#20005));
#5231=EDGE_LOOP('',(#20006,#20007,#20008,#20009));
#5232=EDGE_LOOP('',(#20010,#20011,#20012,#20013));
#5233=EDGE_LOOP('',(#20014,#20015,#20016,#20017,#20018));
#5234=EDGE_LOOP('',(#20019,#20020,#20021,#20022));
#5235=EDGE_LOOP('',(#20023,#20024,#20025,#20026));
#5236=EDGE_LOOP('',(#20027,#20028,#20029,#20030));
#5237=EDGE_LOOP('',(#20031,#20032,#20033,#20034));
#5238=EDGE_LOOP('',(#20035,#20036,#20037,#20038));
#5239=EDGE_LOOP('',(#20039,#20040,#20041,#20042));
#5240=EDGE_LOOP('',(#20043,#20044,#20045,#20046));
#5241=EDGE_LOOP('',(#20047,#20048,#20049,#20050));
#5242=EDGE_LOOP('',(#20051,#20052,#20053,#20054));
#5243=EDGE_LOOP('',(#20055,#20056,#20057,#20058));
#5244=EDGE_LOOP('',(#20059,#20060,#20061,#20062));
#5245=EDGE_LOOP('',(#20063,#20064,#20065,#20066));
#5246=EDGE_LOOP('',(#20067,#20068,#20069,#20070));
#5247=EDGE_LOOP('',(#20071,#20072,#20073,#20074));
#5248=EDGE_LOOP('',(#20075,#20076,#20077,#20078));
#5249=EDGE_LOOP('',(#20079,#20080,#20081,#20082));
#5250=EDGE_LOOP('',(#20083,#20084,#20085,#20086));
#5251=EDGE_LOOP('',(#20087,#20088,#20089,#20090));
#5252=EDGE_LOOP('',(#20091,#20092,#20093,#20094));
#5253=EDGE_LOOP('',(#20095,#20096,#20097,#20098));
#5254=EDGE_LOOP('',(#20099,#20100,#20101,#20102));
#5255=EDGE_LOOP('',(#20103,#20104,#20105,#20106));
#5256=EDGE_LOOP('',(#20107,#20108,#20109,#20110));
#5257=EDGE_LOOP('',(#20111,#20112,#20113,#20114,#20115,#20116,#20117,#20118,
#20119,#20120,#20121,#20122,#20123,#20124,#20125,#20126,#20127,#20128,#20129,
#20130,#20131,#20132,#20133,#20134,#20135,#20136,#20137,#20138,#20139,#20140,
#20141,#20142,#20143,#20144,#20145,#20146,#20147,#20148,#20149,#20150,#20151,
#20152,#20153,#20154,#20155,#20156,#20157,#20158,#20159));
#5258=EDGE_LOOP('',(#20160,#20161,#20162,#20163,#20164));
#5259=EDGE_LOOP('',(#20165,#20166,#20167,#20168));
#5260=EDGE_LOOP('',(#20169,#20170,#20171,#20172,#20173,#20174,#20175,#20176,
#20177,#20178,#20179,#20180,#20181,#20182,#20183,#20184,#20185,#20186,#20187,
#20188,#20189,#20190,#20191,#20192,#20193,#20194,#20195,#20196,#20197,#20198,
#20199,#20200,#20201,#20202,#20203,#20204,#20205,#20206,#20207,#20208,#20209,
#20210,#20211,#20212,#20213,#20214,#20215,#20216));
#5261=EDGE_LOOP('',(#20217,#20218,#20219));
#5262=EDGE_LOOP('',(#20220,#20221,#20222,#20223,#20224,#20225));
#5263=EDGE_LOOP('',(#20226));
#5264=EDGE_LOOP('',(#20227));
#5265=EDGE_LOOP('',(#20228,#20229,#20230));
#5266=EDGE_LOOP('',(#20231,#20232,#20233,#20234));
#5267=EDGE_LOOP('',(#20235,#20236,#20237,#20238));
#5268=EDGE_LOOP('',(#20239,#20240,#20241,#20242));
#5269=EDGE_LOOP('',(#20243,#20244,#20245,#20246));
#5270=EDGE_LOOP('',(#20247,#20248,#20249,#20250));
#5271=EDGE_LOOP('',(#20251,#20252,#20253,#20254));
#5272=EDGE_LOOP('',(#20255,#20256,#20257,#20258,#20259,#20260));
#5273=EDGE_LOOP('',(#20261));
#5274=EDGE_LOOP('',(#20262,#20263,#20264,#20265));
#5275=EDGE_LOOP('',(#20266,#20267,#20268));
#5276=EDGE_LOOP('',(#20269,#20270,#20271,#20272));
#5277=EDGE_LOOP('',(#20273,#20274,#20275));
#5278=EDGE_LOOP('',(#20276,#20277,#20278,#20279));
#5279=EDGE_LOOP('',(#20280,#20281,#20282));
#5280=EDGE_LOOP('',(#20283,#20284,#20285,#20286));
#5281=EDGE_LOOP('',(#20287,#20288,#20289));
#5282=EDGE_LOOP('',(#20290,#20291,#20292,#20293));
#5283=EDGE_LOOP('',(#20294,#20295,#20296));
#5284=EDGE_LOOP('',(#20297,#20298,#20299,#20300));
#5285=EDGE_LOOP('',(#20301,#20302,#20303));
#5286=EDGE_LOOP('',(#20304,#20305,#20306,#20307));
#5287=EDGE_LOOP('',(#20308,#20309,#20310));
#5288=EDGE_LOOP('',(#20311,#20312,#20313,#20314));
#5289=EDGE_LOOP('',(#20315,#20316,#20317));
#5290=EDGE_LOOP('',(#20318,#20319,#20320,#20321));
#5291=EDGE_LOOP('',(#20322,#20323,#20324));
#5292=EDGE_LOOP('',(#20325,#20326,#20327,#20328));
#5293=EDGE_LOOP('',(#20329,#20330,#20331));
#5294=EDGE_LOOP('',(#20332,#20333,#20334,#20335));
#5295=EDGE_LOOP('',(#20336,#20337,#20338));
#5296=EDGE_LOOP('',(#20339,#20340,#20341,#20342));
#5297=EDGE_LOOP('',(#20343,#20344,#20345));
#5298=EDGE_LOOP('',(#20346,#20347,#20348,#20349));
#5299=EDGE_LOOP('',(#20350,#20351,#20352));
#5300=EDGE_LOOP('',(#20353,#20354,#20355,#20356));
#5301=EDGE_LOOP('',(#20357,#20358,#20359));
#5302=EDGE_LOOP('',(#20360,#20361,#20362,#20363));
#5303=EDGE_LOOP('',(#20364,#20365,#20366));
#5304=EDGE_LOOP('',(#20367,#20368,#20369,#20370));
#5305=EDGE_LOOP('',(#20371,#20372,#20373));
#5306=EDGE_LOOP('',(#20374,#20375,#20376,#20377));
#5307=EDGE_LOOP('',(#20378,#20379,#20380,#20381));
#5308=EDGE_LOOP('',(#20382,#20383,#20384,#20385));
#5309=EDGE_LOOP('',(#20386,#20387,#20388,#20389));
#5310=EDGE_LOOP('',(#20390,#20391,#20392,#20393));
#5311=EDGE_LOOP('',(#20394,#20395,#20396));
#5312=EDGE_LOOP('',(#20397,#20398,#20399,#20400));
#5313=EDGE_LOOP('',(#20401,#20402,#20403));
#5314=EDGE_LOOP('',(#20404,#20405,#20406,#20407));
#5315=EDGE_LOOP('',(#20408,#20409,#20410));
#5316=EDGE_LOOP('',(#20411,#20412,#20413,#20414));
#5317=EDGE_LOOP('',(#20415,#20416,#20417));
#5318=EDGE_LOOP('',(#20418,#20419,#20420,#20421));
#5319=EDGE_LOOP('',(#20422,#20423,#20424));
#5320=EDGE_LOOP('',(#20425,#20426,#20427,#20428));
#5321=EDGE_LOOP('',(#20429,#20430,#20431));
#5322=EDGE_LOOP('',(#20432,#20433,#20434,#20435));
#5323=EDGE_LOOP('',(#20436,#20437,#20438));
#5324=EDGE_LOOP('',(#20439,#20440,#20441,#20442));
#5325=EDGE_LOOP('',(#20443,#20444,#20445));
#5326=EDGE_LOOP('',(#20446,#20447,#20448,#20449));
#5327=EDGE_LOOP('',(#20450,#20451,#20452));
#5328=EDGE_LOOP('',(#20453,#20454,#20455,#20456));
#5329=EDGE_LOOP('',(#20457,#20458,#20459));
#5330=EDGE_LOOP('',(#20460,#20461,#20462,#20463));
#5331=EDGE_LOOP('',(#20464,#20465,#20466));
#5332=EDGE_LOOP('',(#20467,#20468,#20469,#20470));
#5333=EDGE_LOOP('',(#20471,#20472,#20473));
#5334=EDGE_LOOP('',(#20474,#20475,#20476,#20477));
#5335=EDGE_LOOP('',(#20478,#20479,#20480));
#5336=EDGE_LOOP('',(#20481,#20482,#20483,#20484));
#5337=EDGE_LOOP('',(#20485,#20486,#20487));
#5338=EDGE_LOOP('',(#20488,#20489,#20490,#20491));
#5339=EDGE_LOOP('',(#20492,#20493,#20494));
#5340=EDGE_LOOP('',(#20495,#20496,#20497,#20498));
#5341=EDGE_LOOP('',(#20499,#20500,#20501));
#5342=EDGE_LOOP('',(#20502,#20503,#20504,#20505));
#5343=EDGE_LOOP('',(#20506,#20507,#20508));
#5344=EDGE_LOOP('',(#20509,#20510,#20511,#20512));
#5345=EDGE_LOOP('',(#20513,#20514,#20515));
#5346=EDGE_LOOP('',(#20516,#20517,#20518,#20519));
#5347=EDGE_LOOP('',(#20520,#20521,#20522));
#5348=EDGE_LOOP('',(#20523,#20524,#20525,#20526));
#5349=EDGE_LOOP('',(#20527,#20528,#20529));
#5350=EDGE_LOOP('',(#20530,#20531,#20532,#20533));
#5351=EDGE_LOOP('',(#20534,#20535,#20536));
#5352=EDGE_LOOP('',(#20537,#20538,#20539,#20540));
#5353=EDGE_LOOP('',(#20541,#20542,#20543));
#5354=EDGE_LOOP('',(#20544,#20545,#20546,#20547));
#5355=EDGE_LOOP('',(#20548,#20549,#20550));
#5356=EDGE_LOOP('',(#20551,#20552,#20553,#20554));
#5357=EDGE_LOOP('',(#20555,#20556,#20557));
#5358=EDGE_LOOP('',(#20558,#20559,#20560,#20561));
#5359=EDGE_LOOP('',(#20562,#20563,#20564));
#5360=EDGE_LOOP('',(#20565,#20566,#20567,#20568));
#5361=EDGE_LOOP('',(#20569,#20570,#20571));
#5362=EDGE_LOOP('',(#20572,#20573,#20574,#20575));
#5363=EDGE_LOOP('',(#20576,#20577,#20578));
#5364=EDGE_LOOP('',(#20579,#20580,#20581,#20582));
#5365=EDGE_LOOP('',(#20583,#20584,#20585));
#5366=EDGE_LOOP('',(#20586,#20587,#20588,#20589));
#5367=EDGE_LOOP('',(#20590,#20591,#20592));
#5368=EDGE_LOOP('',(#20593,#20594,#20595,#20596));
#5369=EDGE_LOOP('',(#20597,#20598,#20599));
#5370=EDGE_LOOP('',(#20600,#20601,#20602,#20603));
#5371=EDGE_LOOP('',(#20604,#20605,#20606));
#5372=EDGE_LOOP('',(#20607,#20608,#20609,#20610));
#5373=EDGE_LOOP('',(#20611,#20612,#20613));
#5374=EDGE_LOOP('',(#20614,#20615,#20616,#20617));
#5375=EDGE_LOOP('',(#20618,#20619,#20620));
#5376=EDGE_LOOP('',(#20621,#20622,#20623,#20624));
#5377=EDGE_LOOP('',(#20625,#20626,#20627));
#5378=EDGE_LOOP('',(#20628,#20629,#20630));
#5379=EDGE_LOOP('',(#20631,#20632,#20633,#20634));
#5380=EDGE_LOOP('',(#20635,#20636,#20637,#20638));
#5381=EDGE_LOOP('',(#20639,#20640,#20641));
#5382=EDGE_LOOP('',(#20642,#20643,#20644,#20645));
#5383=EDGE_LOOP('',(#20646,#20647,#20648));
#5384=EDGE_LOOP('',(#20649,#20650,#20651,#20652));
#5385=EDGE_LOOP('',(#20653,#20654,#20655));
#5386=EDGE_LOOP('',(#20656,#20657,#20658,#20659));
#5387=EDGE_LOOP('',(#20660,#20661,#20662));
#5388=EDGE_LOOP('',(#20663,#20664,#20665,#20666));
#5389=EDGE_LOOP('',(#20667,#20668,#20669));
#5390=EDGE_LOOP('',(#20670,#20671,#20672,#20673));
#5391=EDGE_LOOP('',(#20674,#20675,#20676));
#5392=EDGE_LOOP('',(#20677,#20678,#20679,#20680));
#5393=EDGE_LOOP('',(#20681,#20682,#20683));
#5394=EDGE_LOOP('',(#20684,#20685,#20686,#20687));
#5395=EDGE_LOOP('',(#20688,#20689,#20690));
#5396=EDGE_LOOP('',(#20691,#20692,#20693,#20694));
#5397=EDGE_LOOP('',(#20695,#20696,#20697));
#5398=EDGE_LOOP('',(#20698,#20699,#20700,#20701));
#5399=EDGE_LOOP('',(#20702,#20703,#20704));
#5400=EDGE_LOOP('',(#20705,#20706,#20707,#20708));
#5401=EDGE_LOOP('',(#20709,#20710,#20711));
#5402=EDGE_LOOP('',(#20712,#20713,#20714,#20715));
#5403=EDGE_LOOP('',(#20716,#20717,#20718));
#5404=EDGE_LOOP('',(#20719,#20720,#20721,#20722));
#5405=EDGE_LOOP('',(#20723,#20724,#20725));
#5406=EDGE_LOOP('',(#20726,#20727,#20728,#20729));
#5407=EDGE_LOOP('',(#20730,#20731,#20732));
#5408=EDGE_LOOP('',(#20733,#20734,#20735,#20736));
#5409=EDGE_LOOP('',(#20737,#20738,#20739));
#5410=EDGE_LOOP('',(#20740,#20741,#20742,#20743));
#5411=EDGE_LOOP('',(#20744,#20745,#20746));
#5412=EDGE_LOOP('',(#20747,#20748,#20749,#20750));
#5413=EDGE_LOOP('',(#20751,#20752,#20753));
#5414=EDGE_LOOP('',(#20754,#20755,#20756,#20757));
#5415=EDGE_LOOP('',(#20758,#20759,#20760));
#5416=EDGE_LOOP('',(#20761,#20762,#20763,#20764));
#5417=EDGE_LOOP('',(#20765,#20766,#20767));
#5418=EDGE_LOOP('',(#20768));
#5419=EDGE_LOOP('',(#20769,#20770,#20771,#20772));
#5420=EDGE_LOOP('',(#20773,#20774,#20775,#20776));
#5421=EDGE_LOOP('',(#20777,#20778,#20779,#20780,#20781,#20782,#20783,#20784,
#20785,#20786,#20787,#20788,#20789,#20790,#20791,#20792,#20793,#20794,#20795,
#20796,#20797,#20798,#20799,#20800,#20801,#20802,#20803,#20804,#20805,#20806,
#20807,#20808,#20809,#20810,#20811,#20812,#20813,#20814,#20815,#20816,#20817,
#20818,#20819,#20820,#20821,#20822,#20823,#20824,#20825,#20826,#20827,#20828,
#20829,#20830,#20831,#20832,#20833,#20834,#20835,#20836,#20837,#20838,#20839,
#20840,#20841,#20842,#20843,#20844,#20845,#20846,#20847,#20848,#20849,#20850,
#20851,#20852,#20853,#20854,#20855,#20856,#20857,#20858,#20859,#20860,#20861,
#20862,#20863,#20864,#20865,#20866,#20867,#20868,#20869,#20870,#20871,#20872,
#20873,#20874,#20875,#20876,#20877,#20878,#20879,#20880,#20881,#20882,#20883,
#20884,#20885,#20886,#20887,#20888,#20889,#20890,#20891,#20892,#20893,#20894,
#20895,#20896,#20897,#20898,#20899,#20900,#20901,#20902,#20903,#20904,#20905,
#20906,#20907,#20908,#20909,#20910,#20911,#20912,#20913,#20914,#20915,#20916,
#20917,#20918,#20919,#20920,#20921,#20922,#20923,#20924));
#5422=EDGE_LOOP('',(#20925,#20926,#20927,#20928,#20929,#20930,#20931,#20932,
#20933,#20934,#20935,#20936,#20937,#20938,#20939,#20940,#20941,#20942,#20943,
#20944,#20945,#20946,#20947,#20948,#20949,#20950,#20951,#20952,#20953,#20954,
#20955,#20956,#20957,#20958,#20959,#20960,#20961,#20962,#20963,#20964,#20965,
#20966,#20967,#20968,#20969,#20970,#20971,#20972,#20973,#20974,#20975,#20976,
#20977,#20978,#20979,#20980,#20981,#20982,#20983,#20984,#20985,#20986,#20987,
#20988,#20989,#20990,#20991,#20992,#20993,#20994,#20995,#20996,#20997,#20998,
#20999,#21000));
#5423=EDGE_LOOP('',(#21001));
#5424=EDGE_LOOP('',(#21002,#21003,#21004,#21005,#21006,#21007));
#5425=EDGE_LOOP('',(#21008,#21009,#21010,#21011));
#5426=EDGE_LOOP('',(#21012,#21013,#21014,#21015));
#5427=EDGE_LOOP('',(#21016,#21017,#21018,#21019));
#5428=EDGE_LOOP('',(#21020,#21021,#21022,#21023));
#5429=EDGE_LOOP('',(#21024,#21025,#21026,#21027));
#5430=EDGE_LOOP('',(#21028,#21029,#21030,#21031));
#5431=EDGE_LOOP('',(#21032,#21033,#21034,#21035));
#5432=EDGE_LOOP('',(#21036,#21037,#21038,#21039,#21040));
#5433=EDGE_LOOP('',(#21041,#21042,#21043,#21044));
#5434=EDGE_LOOP('',(#21045,#21046,#21047,#21048));
#5435=EDGE_LOOP('',(#21049,#21050,#21051,#21052));
#5436=EDGE_LOOP('',(#21053,#21054,#21055,#21056));
#5437=EDGE_LOOP('',(#21057,#21058,#21059,#21060));
#5438=EDGE_LOOP('',(#21061,#21062,#21063,#21064));
#5439=EDGE_LOOP('',(#21065,#21066,#21067,#21068));
#5440=EDGE_LOOP('',(#21069,#21070,#21071,#21072));
#5441=EDGE_LOOP('',(#21073,#21074,#21075,#21076));
#5442=EDGE_LOOP('',(#21077,#21078,#21079,#21080));
#5443=EDGE_LOOP('',(#21081,#21082,#21083,#21084));
#5444=EDGE_LOOP('',(#21085,#21086,#21087,#21088));
#5445=EDGE_LOOP('',(#21089,#21090,#21091,#21092));
#5446=EDGE_LOOP('',(#21093,#21094,#21095,#21096));
#5447=EDGE_LOOP('',(#21097,#21098,#21099,#21100));
#5448=EDGE_LOOP('',(#21101,#21102,#21103,#21104));
#5449=EDGE_LOOP('',(#21105,#21106,#21107,#21108));
#5450=EDGE_LOOP('',(#21109,#21110,#21111,#21112));
#5451=EDGE_LOOP('',(#21113,#21114,#21115,#21116,#21117));
#5452=EDGE_LOOP('',(#21118,#21119,#21120,#21121,#21122,#21123,#21124,#21125,
#21126,#21127,#21128,#21129,#21130,#21131,#21132,#21133,#21134,#21135,#21136,
#21137,#21138,#21139));
#5453=EDGE_LOOP('',(#21140,#21141,#21142,#21143));
#5454=EDGE_LOOP('',(#21144,#21145,#21146,#21147,#21148,#21149,#21150,#21151,
#21152,#21153,#21154,#21155,#21156,#21157,#21158,#21159,#21160,#21161,#21162,
#21163,#21164,#21165));
#5455=EDGE_LOOP('',(#21166,#21167,#21168,#21169));
#5456=EDGE_LOOP('',(#21170,#21171,#21172,#21173));
#5457=EDGE_LOOP('',(#21174,#21175,#21176,#21177));
#5458=EDGE_LOOP('',(#21178,#21179,#21180,#21181,#21182,#21183,#21184,#21185,
#21186,#21187,#21188,#21189));
#5459=EDGE_LOOP('',(#21190,#21191,#21192,#21193,#21194,#21195,#21196,#21197,
#21198,#21199));
#5460=EDGE_LOOP('',(#21200,#21201,#21202));
#5461=EDGE_LOOP('',(#21203,#21204,#21205,#21206,#21207,#21208,#21209,#21210,
#21211,#21212,#21213));
#5462=EDGE_LOOP('',(#21214,#21215,#21216,#21217));
#5463=EDGE_LOOP('',(#21218,#21219,#21220,#21221));
#5464=EDGE_LOOP('',(#21222,#21223,#21224,#21225,#21226,#21227,#21228,#21229,
#21230,#21231));
#5465=EDGE_LOOP('',(#21232,#21233,#21234,#21235));
#5466=EDGE_LOOP('',(#21236,#21237,#21238,#21239));
#5467=EDGE_LOOP('',(#21240,#21241,#21242,#21243));
#5468=EDGE_LOOP('',(#21244,#21245,#21246,#21247,#21248,#21249,#21250,#21251,
#21252,#21253));
#5469=EDGE_LOOP('',(#21254,#21255,#21256,#21257));
#5470=EDGE_LOOP('',(#21258));
#5471=EDGE_LOOP('',(#21259,#21260,#21261,#21262));
#5472=EDGE_LOOP('',(#21263));
#5473=EDGE_LOOP('',(#21264));
#5474=EDGE_LOOP('',(#21265));
#5475=EDGE_LOOP('',(#21266));
#5476=EDGE_LOOP('',(#21267,#21268,#21269,#21270));
#5477=EDGE_LOOP('',(#21271,#21272,#21273,#21274,#21275,#21276));
#5478=EDGE_LOOP('',(#21277,#21278,#21279,#21280));
#5479=EDGE_LOOP('',(#21281,#21282,#21283,#21284));
#5480=EDGE_LOOP('',(#21285));
#5481=EDGE_LOOP('',(#21286));
#5482=EDGE_LOOP('',(#21287,#21288,#21289,#21290,#21291));
#5483=EDGE_LOOP('',(#21292,#21293,#21294,#21295,#21296,#21297,#21298));
#5484=EDGE_LOOP('',(#21299));
#5485=EDGE_LOOP('',(#21300,#21301,#21302,#21303));
#5486=EDGE_LOOP('',(#21304,#21305,#21306,#21307,#21308,#21309));
#5487=EDGE_LOOP('',(#21310));
#5488=EDGE_LOOP('',(#21311));
#5489=EDGE_LOOP('',(#21312,#21313,#21314,#21315));
#5490=LINE('',#30697,#6923);
#5491=LINE('',#30701,#6924);
#5492=LINE('',#30727,#6925);
#5493=LINE('',#30751,#6926);
#5494=LINE('',#30755,#6927);
#5495=LINE('',#30758,#6928);
#5496=LINE('',#30761,#6929);
#5497=LINE('',#30765,#6930);
#5498=LINE('',#30768,#6931);
#5499=LINE('',#30771,#6932);
#5500=LINE('',#30775,#6933);
#5501=LINE('',#30778,#6934);
#5502=LINE('',#30781,#6935);
#5503=LINE('',#30785,#6936);
#5504=LINE('',#30788,#6937);
#5505=LINE('',#30791,#6938);
#5506=LINE('',#30795,#6939);
#5507=LINE('',#30798,#6940);
#5508=LINE('',#30801,#6941);
#5509=LINE('',#30805,#6942);
#5510=LINE('',#30808,#6943);
#5511=LINE('',#30811,#6944);
#5512=LINE('',#30815,#6945);
#5513=LINE('',#30818,#6946);
#5514=LINE('',#30821,#6947);
#5515=LINE('',#30825,#6948);
#5516=LINE('',#30828,#6949);
#5517=LINE('',#30834,#6950);
#5518=LINE('',#30838,#6951);
#5519=LINE('',#30840,#6952);
#5520=LINE('',#30846,#6953);
#5521=LINE('',#30854,#6954);
#5522=LINE('',#30858,#6955);
#5523=LINE('',#30864,#6956);
#5524=LINE('',#30868,#6957);
#5525=LINE('',#30872,#6958);
#5526=LINE('',#30887,#6959);
#5527=LINE('',#30889,#6960);
#5528=LINE('',#30891,#6961);
#5529=LINE('',#30900,#6962);
#5530=LINE('',#30902,#6963);
#5531=LINE('',#30904,#6964);
#5532=LINE('',#30905,#6965);
#5533=LINE('',#30913,#6966);
#5534=LINE('',#30915,#6967);
#5535=LINE('',#30917,#6968);
#5536=LINE('',#30919,#6969);
#5537=LINE('',#30928,#6970);
#5538=LINE('',#30930,#6971);
#5539=LINE('',#30931,#6972);
#5540=LINE('',#30933,#6973);
#5541=LINE('',#30934,#6974);
#5542=LINE('',#30993,#6975);
#5543=LINE('',#31006,#6976);
#5544=LINE('',#31029,#6977);
#5545=LINE('',#31179,#6978);
#5546=LINE('',#31225,#6979);
#5547=LINE('',#31250,#6980);
#5548=LINE('',#32189,#6981);
#5549=LINE('',#32191,#6982);
#5550=LINE('',#32193,#6983);
#5551=LINE('',#32194,#6984);
#5552=LINE('',#32198,#6985);
#5553=LINE('',#32204,#6986);
#5554=LINE('',#32205,#6987);
#5555=LINE('',#32206,#6988);
#5556=LINE('',#32212,#6989);
#5557=LINE('',#32215,#6990);
#5558=LINE('',#32218,#6991);
#5559=LINE('',#32219,#6992);
#5560=LINE('',#32223,#6993);
#5561=LINE('',#32226,#6994);
#5562=LINE('',#32233,#6995);
#5563=LINE('',#32239,#6996);
#5564=LINE('',#32249,#6997);
#5565=LINE('',#32255,#6998);
#5566=LINE('',#32262,#6999);
#5567=LINE('',#32270,#7000);
#5568=LINE('',#32273,#7001);
#5569=LINE('',#32277,#7002);
#5570=LINE('',#32281,#7003);
#5571=LINE('',#32285,#7004);
#5572=LINE('',#32289,#7005);
#5573=LINE('',#32293,#7006);
#5574=LINE('',#32300,#7007);
#5575=LINE('',#32328,#7008);
#5576=LINE('',#32366,#7009);
#5577=LINE('',#32404,#7010);
#5578=LINE('',#32441,#7011);
#5579=LINE('',#32478,#7012);
#5580=LINE('',#32516,#7013);
#5581=LINE('',#32554,#7014);
#5582=LINE('',#36394,#7015);
#5583=LINE('',#36396,#7016);
#5584=LINE('',#36398,#7017);
#5585=LINE('',#36399,#7018);
#5586=LINE('',#36402,#7019);
#5587=LINE('',#36404,#7020);
#5588=LINE('',#36405,#7021);
#5589=LINE('',#36408,#7022);
#5590=LINE('',#36410,#7023);
#5591=LINE('',#36411,#7024);
#5592=LINE('',#36414,#7025);
#5593=LINE('',#36416,#7026);
#5594=LINE('',#36417,#7027);
#5595=LINE('',#36420,#7028);
#5596=LINE('',#36422,#7029);
#5597=LINE('',#36423,#7030);
#5598=LINE('',#36425,#7031);
#5599=LINE('',#36426,#7032);
#5600=LINE('',#36431,#7033);
#5601=LINE('',#36433,#7034);
#5602=LINE('',#36435,#7035);
#5603=LINE('',#36436,#7036);
#5604=LINE('',#36440,#7037);
#5605=LINE('',#36443,#7038);
#5606=LINE('',#36444,#7039);
#5607=LINE('',#36450,#7040);
#5608=LINE('',#36452,#7041);
#5609=LINE('',#36454,#7042);
#5610=LINE('',#36455,#7043);
#5611=LINE('',#36459,#7044);
#5612=LINE('',#36462,#7045);
#5613=LINE('',#36463,#7046);
#5614=LINE('',#36469,#7047);
#5615=LINE('',#36471,#7048);
#5616=LINE('',#36473,#7049);
#5617=LINE('',#36474,#7050);
#5618=LINE('',#36478,#7051);
#5619=LINE('',#36481,#7052);
#5620=LINE('',#36482,#7053);
#5621=LINE('',#36488,#7054);
#5622=LINE('',#36490,#7055);
#5623=LINE('',#36492,#7056);
#5624=LINE('',#36493,#7057);
#5625=LINE('',#36497,#7058);
#5626=LINE('',#36500,#7059);
#5627=LINE('',#36501,#7060);
#5628=LINE('',#36507,#7061);
#5629=LINE('',#36509,#7062);
#5630=LINE('',#36511,#7063);
#5631=LINE('',#36512,#7064);
#5632=LINE('',#36516,#7065);
#5633=LINE('',#36519,#7066);
#5634=LINE('',#36520,#7067);
#5635=LINE('',#36526,#7068);
#5636=LINE('',#36528,#7069);
#5637=LINE('',#36530,#7070);
#5638=LINE('',#36531,#7071);
#5639=LINE('',#36535,#7072);
#5640=LINE('',#36538,#7073);
#5641=LINE('',#36539,#7074);
#5642=LINE('',#36545,#7075);
#5643=LINE('',#36547,#7076);
#5644=LINE('',#36549,#7077);
#5645=LINE('',#36550,#7078);
#5646=LINE('',#36554,#7079);
#5647=LINE('',#36557,#7080);
#5648=LINE('',#36558,#7081);
#5649=LINE('',#36566,#7082);
#5650=LINE('',#36567,#7083);
#5651=LINE('',#36570,#7084);
#5652=LINE('',#36572,#7085);
#5653=LINE('',#36573,#7086);
#5654=LINE('',#36576,#7087);
#5655=LINE('',#36577,#7088);
#5656=LINE('',#36583,#7089);
#5657=LINE('',#36585,#7090);
#5658=LINE('',#36587,#7091);
#5659=LINE('',#36588,#7092);
#5660=LINE('',#36592,#7093);
#5661=LINE('',#36595,#7094);
#5662=LINE('',#36596,#7095);
#5663=LINE('',#36602,#7096);
#5664=LINE('',#36604,#7097);
#5665=LINE('',#36606,#7098);
#5666=LINE('',#36607,#7099);
#5667=LINE('',#36611,#7100);
#5668=LINE('',#36614,#7101);
#5669=LINE('',#36615,#7102);
#5670=LINE('',#36621,#7103);
#5671=LINE('',#36623,#7104);
#5672=LINE('',#36625,#7105);
#5673=LINE('',#36626,#7106);
#5674=LINE('',#36630,#7107);
#5675=LINE('',#36633,#7108);
#5676=LINE('',#36634,#7109);
#5677=LINE('',#36640,#7110);
#5678=LINE('',#36642,#7111);
#5679=LINE('',#36644,#7112);
#5680=LINE('',#36645,#7113);
#5681=LINE('',#36649,#7114);
#5682=LINE('',#36652,#7115);
#5683=LINE('',#36653,#7116);
#5684=LINE('',#36659,#7117);
#5685=LINE('',#36661,#7118);
#5686=LINE('',#36663,#7119);
#5687=LINE('',#36664,#7120);
#5688=LINE('',#36668,#7121);
#5689=LINE('',#36671,#7122);
#5690=LINE('',#36672,#7123);
#5691=LINE('',#36678,#7124);
#5692=LINE('',#36680,#7125);
#5693=LINE('',#36682,#7126);
#5694=LINE('',#36683,#7127);
#5695=LINE('',#36687,#7128);
#5696=LINE('',#36690,#7129);
#5697=LINE('',#36691,#7130);
#5698=LINE('',#36697,#7131);
#5699=LINE('',#36699,#7132);
#5700=LINE('',#36701,#7133);
#5701=LINE('',#36702,#7134);
#5702=LINE('',#36706,#7135);
#5703=LINE('',#36709,#7136);
#5704=LINE('',#36710,#7137);
#5705=LINE('',#36716,#7138);
#5706=LINE('',#36718,#7139);
#5707=LINE('',#36720,#7140);
#5708=LINE('',#36721,#7141);
#5709=LINE('',#36725,#7142);
#5710=LINE('',#36728,#7143);
#5711=LINE('',#36729,#7144);
#5712=LINE('',#36735,#7145);
#5713=LINE('',#36737,#7146);
#5714=LINE('',#36739,#7147);
#5715=LINE('',#36740,#7148);
#5716=LINE('',#36744,#7149);
#5717=LINE('',#36747,#7150);
#5718=LINE('',#36748,#7151);
#5719=LINE('',#36754,#7152);
#5720=LINE('',#36756,#7153);
#5721=LINE('',#36758,#7154);
#5722=LINE('',#36759,#7155);
#5723=LINE('',#36763,#7156);
#5724=LINE('',#36766,#7157);
#5725=LINE('',#36767,#7158);
#5726=LINE('',#36773,#7159);
#5727=LINE('',#36775,#7160);
#5728=LINE('',#36777,#7161);
#5729=LINE('',#36778,#7162);
#5730=LINE('',#36782,#7163);
#5731=LINE('',#36785,#7164);
#5732=LINE('',#36786,#7165);
#5733=LINE('',#36792,#7166);
#5734=LINE('',#36794,#7167);
#5735=LINE('',#36796,#7168);
#5736=LINE('',#36797,#7169);
#5737=LINE('',#36801,#7170);
#5738=LINE('',#36804,#7171);
#5739=LINE('',#36805,#7172);
#5740=LINE('',#36811,#7173);
#5741=LINE('',#36813,#7174);
#5742=LINE('',#36815,#7175);
#5743=LINE('',#36816,#7176);
#5744=LINE('',#36820,#7177);
#5745=LINE('',#36823,#7178);
#5746=LINE('',#36824,#7179);
#5747=LINE('',#36830,#7180);
#5748=LINE('',#36832,#7181);
#5749=LINE('',#36834,#7182);
#5750=LINE('',#36835,#7183);
#5751=LINE('',#36839,#7184);
#5752=LINE('',#36842,#7185);
#5753=LINE('',#36843,#7186);
#5754=LINE('',#36849,#7187);
#5755=LINE('',#36851,#7188);
#5756=LINE('',#36853,#7189);
#5757=LINE('',#36854,#7190);
#5758=LINE('',#36859,#7191);
#5759=LINE('',#36863,#7192);
#5760=LINE('',#36864,#7193);
#5761=LINE('',#36872,#7194);
#5762=LINE('',#36874,#7195);
#5763=LINE('',#36876,#7196);
#5764=LINE('',#36877,#7197);
#5765=LINE('',#36881,#7198);
#5766=LINE('',#36884,#7199);
#5767=LINE('',#36885,#7200);
#5768=LINE('',#36891,#7201);
#5769=LINE('',#36893,#7202);
#5770=LINE('',#36895,#7203);
#5771=LINE('',#36896,#7204);
#5772=LINE('',#36900,#7205);
#5773=LINE('',#36903,#7206);
#5774=LINE('',#36904,#7207);
#5775=LINE('',#36910,#7208);
#5776=LINE('',#36912,#7209);
#5777=LINE('',#36914,#7210);
#5778=LINE('',#36915,#7211);
#5779=LINE('',#36919,#7212);
#5780=LINE('',#36922,#7213);
#5781=LINE('',#36923,#7214);
#5782=LINE('',#36929,#7215);
#5783=LINE('',#36931,#7216);
#5784=LINE('',#36933,#7217);
#5785=LINE('',#36934,#7218);
#5786=LINE('',#36938,#7219);
#5787=LINE('',#36941,#7220);
#5788=LINE('',#36942,#7221);
#5789=LINE('',#36948,#7222);
#5790=LINE('',#36950,#7223);
#5791=LINE('',#36952,#7224);
#5792=LINE('',#36953,#7225);
#5793=LINE('',#36957,#7226);
#5794=LINE('',#36960,#7227);
#5795=LINE('',#36961,#7228);
#5796=LINE('',#36967,#7229);
#5797=LINE('',#36969,#7230);
#5798=LINE('',#36971,#7231);
#5799=LINE('',#36972,#7232);
#5800=LINE('',#36976,#7233);
#5801=LINE('',#36979,#7234);
#5802=LINE('',#36980,#7235);
#5803=LINE('',#36986,#7236);
#5804=LINE('',#36988,#7237);
#5805=LINE('',#36990,#7238);
#5806=LINE('',#36991,#7239);
#5807=LINE('',#36995,#7240);
#5808=LINE('',#36998,#7241);
#5809=LINE('',#36999,#7242);
#5810=LINE('',#37006,#7243);
#5811=LINE('',#37036,#7244);
#5812=LINE('',#37041,#7245);
#5813=LINE('',#37044,#7246);
#5814=LINE('',#37050,#7247);
#5815=LINE('',#37064,#7248);
#5816=LINE('',#37074,#7249);
#5817=LINE('',#37082,#7250);
#5818=LINE('',#37088,#7251);
#5819=LINE('',#37092,#7252);
#5820=LINE('',#37097,#7253);
#5821=LINE('',#37102,#7254);
#5822=LINE('',#37117,#7255);
#5823=LINE('',#37138,#7256);
#5824=LINE('',#37144,#7257);
#5825=LINE('',#37172,#7258);
#5826=LINE('',#37210,#7259);
#5827=LINE('',#37248,#7260);
#5828=LINE('',#37286,#7261);
#5829=LINE('',#37325,#7262);
#5830=LINE('',#37358,#7263);
#5831=LINE('',#37442,#7264);
#5832=LINE('',#37532,#7265);
#5833=LINE('',#37616,#7266);
#5834=LINE('',#37706,#7267);
#5835=LINE('',#37796,#7268);
#5836=LINE('',#37880,#7269);
#5837=LINE('',#37900,#7270);
#5838=LINE('',#37937,#7271);
#5839=LINE('',#37974,#7272);
#5840=LINE('',#38012,#7273);
#5841=LINE('',#38049,#7274);
#5842=LINE('',#38086,#7275);
#5843=LINE('',#41738,#7276);
#5844=LINE('',#41768,#7277);
#5845=LINE('',#41773,#7278);
#5846=LINE('',#41776,#7279);
#5847=LINE('',#41782,#7280);
#5848=LINE('',#41796,#7281);
#5849=LINE('',#41806,#7282);
#5850=LINE('',#41818,#7283);
#5851=LINE('',#41822,#7284);
#5852=LINE('',#41827,#7285);
#5853=LINE('',#41832,#7286);
#5854=LINE('',#41837,#7287);
#5855=LINE('',#41841,#7288);
#5856=LINE('',#41846,#7289);
#5857=LINE('',#41852,#7290);
#5858=LINE('',#41856,#7291);
#5859=LINE('',#41860,#7292);
#5860=LINE('',#41862,#7293);
#5861=LINE('',#41864,#7294);
#5862=LINE('',#41865,#7295);
#5863=LINE('',#41888,#7296);
#5864=LINE('',#41891,#7297);
#5865=LINE('',#41893,#7298);
#5866=LINE('',#41894,#7299);
#5867=LINE('',#41919,#7300);
#5868=LINE('',#41921,#7301);
#5869=LINE('',#41923,#7302);
#5870=LINE('',#41924,#7303);
#5871=LINE('',#41947,#7304);
#5872=LINE('',#41950,#7305);
#5873=LINE('',#41952,#7306);
#5874=LINE('',#41953,#7307);
#5875=LINE('',#41981,#7308);
#5876=LINE('',#41985,#7309);
#5877=LINE('',#41992,#7310);
#5878=LINE('',#41996,#7311);
#5879=LINE('',#42003,#7312);
#5880=LINE('',#42010,#7313);
#5881=LINE('',#42017,#7314);
#5882=LINE('',#42024,#7315);
#5883=LINE('',#42028,#7316);
#5884=LINE('',#42039,#7317);
#5885=LINE('',#42045,#7318);
#5886=LINE('',#42050,#7319);
#5887=LINE('',#42052,#7320);
#5888=LINE('',#42054,#7321);
#5889=LINE('',#42055,#7322);
#5890=LINE('',#42058,#7323);
#5891=LINE('',#42060,#7324);
#5892=LINE('',#42061,#7325);
#5893=LINE('',#42065,#7326);
#5894=LINE('',#42066,#7327);
#5895=LINE('',#42067,#7328);
#5896=LINE('',#42076,#7329);
#5897=LINE('',#42082,#7330);
#5898=LINE('',#42088,#7331);
#5899=LINE('',#42094,#7332);
#5900=LINE('',#42100,#7333);
#5901=LINE('',#42106,#7334);
#5902=LINE('',#42112,#7335);
#5903=LINE('',#42118,#7336);
#5904=LINE('',#42124,#7337);
#5905=LINE('',#42138,#7338);
#5906=LINE('',#42154,#7339);
#5907=LINE('',#42170,#7340);
#5908=LINE('',#42186,#7341);
#5909=LINE('',#42202,#7342);
#5910=LINE('',#42218,#7343);
#5911=LINE('',#42234,#7344);
#5912=LINE('',#42250,#7345);
#5913=LINE('',#42266,#7346);
#5914=LINE('',#42286,#7347);
#5915=LINE('',#42289,#7348);
#5916=LINE('',#42291,#7349);
#5917=LINE('',#42295,#7350);
#5918=LINE('',#42299,#7351);
#5919=LINE('',#42307,#7352);
#5920=LINE('',#42309,#7353);
#5921=LINE('',#42311,#7354);
#5922=LINE('',#42312,#7355);
#5923=LINE('',#42315,#7356);
#5924=LINE('',#42317,#7357);
#5925=LINE('',#42318,#7358);
#5926=LINE('',#42321,#7359);
#5927=LINE('',#42323,#7360);
#5928=LINE('',#42324,#7361);
#5929=LINE('',#42327,#7362);
#5930=LINE('',#42329,#7363);
#5931=LINE('',#42330,#7364);
#5932=LINE('',#42335,#7365);
#5933=LINE('',#42339,#7366);
#5934=LINE('',#42341,#7367);
#5935=LINE('',#42342,#7368);
#5936=LINE('',#42351,#7369);
#5937=LINE('',#42360,#7370);
#5938=LINE('',#42366,#7371);
#5939=LINE('',#42375,#7372);
#5940=LINE('',#42381,#7373);
#5941=LINE('',#42390,#7374);
#5942=LINE('',#42396,#7375);
#5943=LINE('',#42405,#7376);
#5944=LINE('',#42411,#7377);
#5945=LINE('',#42420,#7378);
#5946=LINE('',#42426,#7379);
#5947=LINE('',#42435,#7380);
#5948=LINE('',#42459,#7381);
#5949=LINE('',#42573,#7382);
#5950=LINE('',#42589,#7383);
#5951=LINE('',#42591,#7384);
#5952=LINE('',#42593,#7385);
#5953=LINE('',#42595,#7386);
#5954=LINE('',#42600,#7387);
#5955=LINE('',#42604,#7388);
#5956=LINE('',#42647,#7389);
#5957=LINE('',#42651,#7390);
#5958=LINE('',#42695,#7391);
#5959=LINE('',#42702,#7392);
#5960=LINE('',#42708,#7393);
#5961=LINE('',#42715,#7394);
#5962=LINE('',#42726,#7395);
#5963=LINE('',#42729,#7396);
#5964=LINE('',#42734,#7397);
#5965=LINE('',#42736,#7398);
#5966=LINE('',#42740,#7399);
#5967=LINE('',#42744,#7400);
#5968=LINE('',#42746,#7401);
#5969=LINE('',#42752,#7402);
#5970=LINE('',#42759,#7403);
#5971=LINE('',#42766,#7404);
#5972=LINE('',#42773,#7405);
#5973=LINE('',#42781,#7406);
#5974=LINE('',#42786,#7407);
#5975=LINE('',#42790,#7408);
#5976=LINE('',#42794,#7409);
#5977=LINE('',#42813,#7410);
#5978=LINE('',#42817,#7411);
#5979=LINE('',#42821,#7412);
#5980=LINE('',#42853,#7413);
#5981=LINE('',#42858,#7414);
#5982=LINE('',#42860,#7415);
#5983=LINE('',#42863,#7416);
#5984=LINE('',#42868,#7417);
#5985=LINE('',#42870,#7418);
#5986=LINE('',#42873,#7419);
#5987=LINE('',#42878,#7420);
#5988=LINE('',#42880,#7421);
#5989=LINE('',#42883,#7422);
#5990=LINE('',#42888,#7423);
#5991=LINE('',#42890,#7424);
#5992=LINE('',#42893,#7425);
#5993=LINE('',#42898,#7426);
#5994=LINE('',#42900,#7427);
#5995=LINE('',#42940,#7428);
#5996=LINE('',#42945,#7429);
#5997=LINE('',#42950,#7430);
#5998=LINE('',#42957,#7431);
#5999=LINE('',#42966,#7432);
#6000=LINE('',#42974,#7433);
#6001=LINE('',#42978,#7434);
#6002=LINE('',#42986,#7435);
#6003=LINE('',#42995,#7436);
#6004=LINE('',#43003,#7437);
#6005=LINE('',#43016,#7438);
#6006=LINE('',#43020,#7439);
#6007=LINE('',#43074,#7440);
#6008=LINE('',#43078,#7441);
#6009=LINE('',#43080,#7442);
#6010=LINE('',#43094,#7443);
#6011=LINE('',#43107,#7444);
#6012=LINE('',#43121,#7445);
#6013=LINE('',#43145,#7446);
#6014=LINE('',#43170,#7447);
#6015=LINE('',#43172,#7448);
#6016=LINE('',#43180,#7449);
#6017=LINE('',#43184,#7450);
#6018=LINE('',#43189,#7451);
#6019=LINE('',#43193,#7452);
#6020=LINE('',#43198,#7453);
#6021=LINE('',#43207,#7454);
#6022=LINE('',#43209,#7455);
#6023=LINE('',#43228,#7456);
#6024=LINE('',#43233,#7457);
#6025=LINE('',#43245,#7458);
#6026=LINE('',#43260,#7459);
#6027=LINE('',#43275,#7460);
#6028=LINE('',#43290,#7461);
#6029=LINE('',#43305,#7462);
#6030=LINE('',#43320,#7463);
#6031=LINE('',#43335,#7464);
#6032=LINE('',#43350,#7465);
#6033=LINE('',#43355,#7466);
#6034=LINE('',#43356,#7467);
#6035=LINE('',#43369,#7468);
#6036=LINE('',#43374,#7469);
#6037=LINE('',#43386,#7470);
#6038=LINE('',#43392,#7471);
#6039=LINE('',#43394,#7472);
#6040=LINE('',#43395,#7473);
#6041=LINE('',#43407,#7474);
#6042=LINE('',#43422,#7475);
#6043=LINE('',#43437,#7476);
#6044=LINE('',#43452,#7477);
#6045=LINE('',#43467,#7478);
#6046=LINE('',#43482,#7479);
#6047=LINE('',#43497,#7480);
#6048=LINE('',#43503,#7481);
#6049=LINE('',#43505,#7482);
#6050=LINE('',#43506,#7483);
#6051=LINE('',#43518,#7484);
#6052=LINE('',#43533,#7485);
#6053=LINE('',#43548,#7486);
#6054=LINE('',#43563,#7487);
#6055=LINE('',#43578,#7488);
#6056=LINE('',#43593,#7489);
#6057=LINE('',#43608,#7490);
#6058=LINE('',#43623,#7491);
#6059=LINE('',#43638,#7492);
#6060=LINE('',#43653,#7493);
#6061=LINE('',#43668,#7494);
#6062=LINE('',#43683,#7495);
#6063=LINE('',#43698,#7496);
#6064=LINE('',#43713,#7497);
#6065=LINE('',#43728,#7498);
#6066=LINE('',#43733,#7499);
#6067=LINE('',#43734,#7500);
#6068=LINE('',#43748,#7501);
#6069=LINE('',#43753,#7502);
#6070=LINE('',#43765,#7503);
#6071=LINE('',#43780,#7504);
#6072=LINE('',#43795,#7505);
#6073=LINE('',#43810,#7506);
#6074=LINE('',#43825,#7507);
#6075=LINE('',#43840,#7508);
#6076=LINE('',#43868,#7509);
#6077=LINE('',#43873,#7510);
#6078=LINE('',#43885,#7511);
#6079=LINE('',#43900,#7512);
#6080=LINE('',#43915,#7513);
#6081=LINE('',#43930,#7514);
#6082=LINE('',#43945,#7515);
#6083=LINE('',#43960,#7516);
#6084=LINE('',#43975,#7517);
#6085=LINE('',#43990,#7518);
#6086=LINE('',#44005,#7519);
#6087=LINE('',#44020,#7520);
#6088=LINE('',#44049,#7521);
#6089=LINE('',#44054,#7522);
#6090=LINE('',#44066,#7523);
#6091=LINE('',#44072,#7524);
#6092=LINE('',#44074,#7525);
#6093=LINE('',#44075,#7526);
#6094=LINE('',#44087,#7527);
#6095=LINE('',#44102,#7528);
#6096=LINE('',#44108,#7529);
#6097=LINE('',#44110,#7530);
#6098=LINE('',#44111,#7531);
#6099=LINE('',#44114,#7532);
#6100=LINE('',#44116,#7533);
#6101=LINE('',#44117,#7534);
#6102=LINE('',#44120,#7535);
#6103=LINE('',#44122,#7536);
#6104=LINE('',#44123,#7537);
#6105=LINE('',#44125,#7538);
#6106=LINE('',#44126,#7539);
#6107=LINE('',#44131,#7540);
#6108=LINE('',#44133,#7541);
#6109=LINE('',#44135,#7542);
#6110=LINE('',#44136,#7543);
#6111=LINE('',#44139,#7544);
#6112=LINE('',#44141,#7545);
#6113=LINE('',#44142,#7546);
#6114=LINE('',#44145,#7547);
#6115=LINE('',#44147,#7548);
#6116=LINE('',#44148,#7549);
#6117=LINE('',#44151,#7550);
#6118=LINE('',#44153,#7551);
#6119=LINE('',#44154,#7552);
#6120=LINE('',#44157,#7553);
#6121=LINE('',#44159,#7554);
#6122=LINE('',#44160,#7555);
#6123=LINE('',#44163,#7556);
#6124=LINE('',#44165,#7557);
#6125=LINE('',#44166,#7558);
#6126=LINE('',#44169,#7559);
#6127=LINE('',#44171,#7560);
#6128=LINE('',#44172,#7561);
#6129=LINE('',#44175,#7562);
#6130=LINE('',#44177,#7563);
#6131=LINE('',#44178,#7564);
#6132=LINE('',#44190,#7565);
#6133=LINE('',#44205,#7566);
#6134=LINE('',#44211,#7567);
#6135=LINE('',#44213,#7568);
#6136=LINE('',#44214,#7569);
#6137=LINE('',#44217,#7570);
#6138=LINE('',#44219,#7571);
#6139=LINE('',#44220,#7572);
#6140=LINE('',#44223,#7573);
#6141=LINE('',#44225,#7574);
#6142=LINE('',#44226,#7575);
#6143=LINE('',#44229,#7576);
#6144=LINE('',#44231,#7577);
#6145=LINE('',#44232,#7578);
#6146=LINE('',#44234,#7579);
#6147=LINE('',#44235,#7580);
#6148=LINE('',#44249,#7581);
#6149=LINE('',#44254,#7582);
#6150=LINE('',#44266,#7583);
#6151=LINE('',#44281,#7584);
#6152=LINE('',#44296,#7585);
#6153=LINE('',#44311,#7586);
#6154=LINE('',#44326,#7587);
#6155=LINE('',#44341,#7588);
#6156=LINE('',#44356,#7589);
#6157=LINE('',#44371,#7590);
#6158=LINE('',#44386,#7591);
#6159=LINE('',#44401,#7592);
#6160=LINE('',#44407,#7593);
#6161=LINE('',#44409,#7594);
#6162=LINE('',#44410,#7595);
#6163=LINE('',#44422,#7596);
#6164=LINE('',#44437,#7597);
#6165=LINE('',#44452,#7598);
#6166=LINE('',#44467,#7599);
#6167=LINE('',#44482,#7600);
#6168=LINE('',#44497,#7601);
#6169=LINE('',#44512,#7602);
#6170=LINE('',#44518,#7603);
#6171=LINE('',#44520,#7604);
#6172=LINE('',#44521,#7605);
#6173=LINE('',#44533,#7606);
#6174=LINE('',#44548,#7607);
#6175=LINE('',#44563,#7608);
#6176=LINE('',#44578,#7609);
#6177=LINE('',#44593,#7610);
#6178=LINE('',#44608,#7611);
#6179=LINE('',#44623,#7612);
#6180=LINE('',#44629,#7613);
#6181=LINE('',#44631,#7614);
#6182=LINE('',#44632,#7615);
#6183=LINE('',#44644,#7616);
#6184=LINE('',#44664,#7617);
#6185=LINE('',#44666,#7618);
#6186=LINE('',#44668,#7619);
#6187=LINE('',#44669,#7620);
#6188=LINE('',#44672,#7621);
#6189=LINE('',#44674,#7622);
#6190=LINE('',#44675,#7623);
#6191=LINE('',#44678,#7624);
#6192=LINE('',#44680,#7625);
#6193=LINE('',#44681,#7626);
#6194=LINE('',#44683,#7627);
#6195=LINE('',#44684,#7628);
#6196=LINE('',#44698,#7629);
#6197=LINE('',#44703,#7630);
#6198=LINE('',#44715,#7631);
#6199=LINE('',#44721,#7632);
#6200=LINE('',#44723,#7633);
#6201=LINE('',#44724,#7634);
#6202=LINE('',#44727,#7635);
#6203=LINE('',#44729,#7636);
#6204=LINE('',#44730,#7637);
#6205=LINE('',#44732,#7638);
#6206=LINE('',#44733,#7639);
#6207=LINE('',#44737,#7640);
#6208=LINE('',#44739,#7641);
#6209=LINE('',#44741,#7642);
#6210=LINE('',#44742,#7643);
#6211=LINE('',#44745,#7644);
#6212=LINE('',#44747,#7645);
#6213=LINE('',#44748,#7646);
#6214=LINE('',#44751,#7647);
#6215=LINE('',#44753,#7648);
#6216=LINE('',#44754,#7649);
#6217=LINE('',#44757,#7650);
#6218=LINE('',#44759,#7651);
#6219=LINE('',#44760,#7652);
#6220=LINE('',#44763,#7653);
#6221=LINE('',#44765,#7654);
#6222=LINE('',#44766,#7655);
#6223=LINE('',#44769,#7656);
#6224=LINE('',#44771,#7657);
#6225=LINE('',#44772,#7658);
#6226=LINE('',#44775,#7659);
#6227=LINE('',#44777,#7660);
#6228=LINE('',#44778,#7661);
#6229=LINE('',#44780,#7662);
#6230=LINE('',#44781,#7663);
#6231=LINE('',#44795,#7664);
#6232=LINE('',#44800,#7665);
#6233=LINE('',#44812,#7666);
#6234=LINE('',#44827,#7667);
#6235=LINE('',#44842,#7668);
#6236=LINE('',#44857,#7669);
#6237=LINE('',#44872,#7670);
#6238=LINE('',#44887,#7671);
#6239=LINE('',#44902,#7672);
#6240=LINE('',#44917,#7673);
#6241=LINE('',#44932,#7674);
#6242=LINE('',#44947,#7675);
#6243=LINE('',#44962,#7676);
#6244=LINE('',#44977,#7677);
#6245=LINE('',#44983,#7678);
#6246=LINE('',#44985,#7679);
#6247=LINE('',#44986,#7680);
#6248=LINE('',#44998,#7681);
#6249=LINE('',#45013,#7682);
#6250=LINE('',#45028,#7683);
#6251=LINE('',#45043,#7684);
#6252=LINE('',#45058,#7685);
#6253=LINE('',#45073,#7686);
#6254=LINE('',#45088,#7687);
#6255=LINE('',#45103,#7688);
#6256=LINE('',#45118,#7689);
#6257=LINE('',#45133,#7690);
#6258=LINE('',#45148,#7691);
#6259=LINE('',#45163,#7692);
#6260=LINE('',#45178,#7693);
#6261=LINE('',#45193,#7694);
#6262=LINE('',#45208,#7695);
#6263=LINE('',#45223,#7696);
#6264=LINE('',#45238,#7697);
#6265=LINE('',#45253,#7698);
#6266=LINE('',#45259,#7699);
#6267=LINE('',#45261,#7700);
#6268=LINE('',#45262,#7701);
#6269=LINE('',#45274,#7702);
#6270=LINE('',#45303,#7703);
#6271=LINE('',#45308,#7704);
#6272=LINE('',#45320,#7705);
#6273=LINE('',#45335,#7706);
#6274=LINE('',#45350,#7707);
#6275=LINE('',#45365,#7708);
#6276=LINE('',#45380,#7709);
#6277=LINE('',#45395,#7710);
#6278=LINE('',#45410,#7711);
#6279=LINE('',#45425,#7712);
#6280=LINE('',#45440,#7713);
#6281=LINE('',#45455,#7714);
#6282=LINE('',#45461,#7715);
#6283=LINE('',#45463,#7716);
#6284=LINE('',#45464,#7717);
#6285=LINE('',#45476,#7718);
#6286=LINE('',#45491,#7719);
#6287=LINE('',#45506,#7720);
#6288=LINE('',#45521,#7721);
#6289=LINE('',#45536,#7722);
#6290=LINE('',#45551,#7723);
#6291=LINE('',#45566,#7724);
#6292=LINE('',#45572,#7725);
#6293=LINE('',#45574,#7726);
#6294=LINE('',#45575,#7727);
#6295=LINE('',#45587,#7728);
#6296=LINE('',#45602,#7729);
#6297=LINE('',#45617,#7730);
#6298=LINE('',#45632,#7731);
#6299=LINE('',#45647,#7732);
#6300=LINE('',#45662,#7733);
#6301=LINE('',#45677,#7734);
#6302=LINE('',#45683,#7735);
#6303=LINE('',#45685,#7736);
#6304=LINE('',#45686,#7737);
#6305=LINE('',#45698,#7738);
#6306=LINE('',#45727,#7739);
#6307=LINE('',#45732,#7740);
#6308=LINE('',#45744,#7741);
#6309=LINE('',#45759,#7742);
#6310=LINE('',#45774,#7743);
#6311=LINE('',#45789,#7744);
#6312=LINE('',#45804,#7745);
#6313=LINE('',#45819,#7746);
#6314=LINE('',#45834,#7747);
#6315=LINE('',#45840,#7748);
#6316=LINE('',#45842,#7749);
#6317=LINE('',#45843,#7750);
#6318=LINE('',#45855,#7751);
#6319=LINE('',#45870,#7752);
#6320=LINE('',#45885,#7753);
#6321=LINE('',#45900,#7754);
#6322=LINE('',#45915,#7755);
#6323=LINE('',#45930,#7756);
#6324=LINE('',#45945,#7757);
#6325=LINE('',#45960,#7758);
#6326=LINE('',#45975,#7759);
#6327=LINE('',#45981,#7760);
#6328=LINE('',#45983,#7761);
#6329=LINE('',#45984,#7762);
#6330=LINE('',#45987,#7763);
#6331=LINE('',#45989,#7764);
#6332=LINE('',#45990,#7765);
#6333=LINE('',#45993,#7766);
#6334=LINE('',#45995,#7767);
#6335=LINE('',#45996,#7768);
#6336=LINE('',#46013,#7769);
#6337=LINE('',#46015,#7770);
#6338=LINE('',#46017,#7771);
#6339=LINE('',#46018,#7772);
#6340=LINE('',#46030,#7773);
#6341=LINE('',#46045,#7774);
#6342=LINE('',#46060,#7775);
#6343=LINE('',#46075,#7776);
#6344=LINE('',#46090,#7777);
#6345=LINE('',#46096,#7778);
#6346=LINE('',#46098,#7779);
#6347=LINE('',#46099,#7780);
#6348=LINE('',#46101,#7781);
#6349=LINE('',#46102,#7782);
#6350=LINE('',#46106,#7783);
#6351=LINE('',#46108,#7784);
#6352=LINE('',#46110,#7785);
#6353=LINE('',#46111,#7786);
#6354=LINE('',#46123,#7787);
#6355=LINE('',#46138,#7788);
#6356=LINE('',#46153,#7789);
#6357=LINE('',#46168,#7790);
#6358=LINE('',#46183,#7791);
#6359=LINE('',#46198,#7792);
#6360=LINE('',#46204,#7793);
#6361=LINE('',#46206,#7794);
#6362=LINE('',#46207,#7795);
#6363=LINE('',#46210,#7796);
#6364=LINE('',#46212,#7797);
#6365=LINE('',#46213,#7798);
#6366=LINE('',#46216,#7799);
#6367=LINE('',#46218,#7800);
#6368=LINE('',#46219,#7801);
#6369=LINE('',#46221,#7802);
#6370=LINE('',#46222,#7803);
#6371=LINE('',#46236,#7804);
#6372=LINE('',#46241,#7805);
#6373=LINE('',#46253,#7806);
#6374=LINE('',#46268,#7807);
#6375=LINE('',#46283,#7808);
#6376=LINE('',#46298,#7809);
#6377=LINE('',#46313,#7810);
#6378=LINE('',#46328,#7811);
#6379=LINE('',#46343,#7812);
#6380=LINE('',#46371,#7813);
#6381=LINE('',#46376,#7814);
#6382=LINE('',#46388,#7815);
#6383=LINE('',#46403,#7816);
#6384=LINE('',#46418,#7817);
#6385=LINE('',#46433,#7818);
#6386=LINE('',#46448,#7819);
#6387=LINE('',#46463,#7820);
#6388=LINE('',#46478,#7821);
#6389=LINE('',#46493,#7822);
#6390=LINE('',#46508,#7823);
#6391=LINE('',#46523,#7824);
#6392=LINE('',#46538,#7825);
#6393=LINE('',#46553,#7826);
#6394=LINE('',#46568,#7827);
#6395=LINE('',#46583,#7828);
#6396=LINE('',#46598,#7829);
#6397=LINE('',#46604,#7830);
#6398=LINE('',#46606,#7831);
#6399=LINE('',#46607,#7832);
#6400=LINE('',#46619,#7833);
#6401=LINE('',#46648,#7834);
#6402=LINE('',#46653,#7835);
#6403=LINE('',#46665,#7836);
#6404=LINE('',#46680,#7837);
#6405=LINE('',#46695,#7838);
#6406=LINE('',#46710,#7839);
#6407=LINE('',#46725,#7840);
#6408=LINE('',#46740,#7841);
#6409=LINE('',#46768,#7842);
#6410=LINE('',#46773,#7843);
#6411=LINE('',#46785,#7844);
#6412=LINE('',#46800,#7845);
#6413=LINE('',#46815,#7846);
#6414=LINE('',#46830,#7847);
#6415=LINE('',#46845,#7848);
#6416=LINE('',#46860,#7849);
#6417=LINE('',#46866,#7850);
#6418=LINE('',#46868,#7851);
#6419=LINE('',#46869,#7852);
#6420=LINE('',#46872,#7853);
#6421=LINE('',#46874,#7854);
#6422=LINE('',#46875,#7855);
#6423=LINE('',#46878,#7856);
#6424=LINE('',#46880,#7857);
#6425=LINE('',#46881,#7858);
#6426=LINE('',#46884,#7859);
#6427=LINE('',#46886,#7860);
#6428=LINE('',#46887,#7861);
#6429=LINE('',#46890,#7862);
#6430=LINE('',#46892,#7863);
#6431=LINE('',#46893,#7864);
#6432=LINE('',#46919,#7865);
#6433=LINE('',#46924,#7866);
#6434=LINE('',#46936,#7867);
#6435=LINE('',#46951,#7868);
#6436=LINE('',#46966,#7869);
#6437=LINE('',#46972,#7870);
#6438=LINE('',#46974,#7871);
#6439=LINE('',#46975,#7872);
#6440=LINE('',#46987,#7873);
#6441=LINE('',#47002,#7874);
#6442=LINE('',#47017,#7875);
#6443=LINE('',#47023,#7876);
#6444=LINE('',#47025,#7877);
#6445=LINE('',#47026,#7878);
#6446=LINE('',#47029,#7879);
#6447=LINE('',#47031,#7880);
#6448=LINE('',#47032,#7881);
#6449=LINE('',#47035,#7882);
#6450=LINE('',#47037,#7883);
#6451=LINE('',#47038,#7884);
#6452=LINE('',#47041,#7885);
#6453=LINE('',#47043,#7886);
#6454=LINE('',#47044,#7887);
#6455=LINE('',#47046,#7888);
#6456=LINE('',#47047,#7889);
#6457=LINE('',#47059,#7890);
#6458=LINE('',#47107,#7891);
#6459=LINE('',#47112,#7892);
#6460=LINE('',#47116,#7893);
#6461=LINE('',#47145,#7894);
#6462=LINE('',#47146,#7895);
#6463=LINE('',#47150,#7896);
#6464=LINE('',#47153,#7897);
#6465=LINE('',#47155,#7898);
#6466=LINE('',#47164,#7899);
#6467=LINE('',#47175,#7900);
#6468=LINE('',#47194,#7901);
#6469=LINE('',#47198,#7902);
#6470=LINE('',#47202,#7903);
#6471=LINE('',#47206,#7904);
#6472=LINE('',#47210,#7905);
#6473=LINE('',#47214,#7906);
#6474=LINE('',#47218,#7907);
#6475=LINE('',#47222,#7908);
#6476=LINE('',#47226,#7909);
#6477=LINE('',#47230,#7910);
#6478=LINE('',#47234,#7911);
#6479=LINE('',#47238,#7912);
#6480=LINE('',#47241,#7913);
#6481=LINE('',#47244,#7914);
#6482=LINE('',#47247,#7915);
#6483=LINE('',#47250,#7916);
#6484=LINE('',#47253,#7917);
#6485=LINE('',#47256,#7918);
#6486=LINE('',#47263,#7919);
#6487=LINE('',#47266,#7920);
#6488=LINE('',#47272,#7921);
#6489=LINE('',#47284,#7922);
#6490=LINE('',#47290,#7923);
#6491=LINE('',#47298,#7924);
#6492=LINE('',#47304,#7925);
#6493=LINE('',#47310,#7926);
#6494=LINE('',#47315,#7927);
#6495=LINE('',#47317,#7928);
#6496=LINE('',#47321,#7929);
#6497=LINE('',#47325,#7930);
#6498=LINE('',#47331,#7931);
#6499=LINE('',#47335,#7932);
#6500=LINE('',#47339,#7933);
#6501=LINE('',#47348,#7934);
#6502=LINE('',#47354,#7935);
#6503=LINE('',#47368,#7936);
#6504=LINE('',#47375,#7937);
#6505=LINE('',#47381,#7938);
#6506=LINE('',#47385,#7939);
#6507=LINE('',#47389,#7940);
#6508=LINE('',#47396,#7941);
#6509=LINE('',#47400,#7942);
#6510=LINE('',#47407,#7943);
#6511=LINE('',#47651,#7944);
#6512=LINE('',#47892,#7945);
#6513=LINE('',#47894,#7946);
#6514=LINE('',#48238,#7947);
#6515=LINE('',#48250,#7948);
#6516=LINE('',#48352,#7949);
#6517=LINE('',#48358,#7950);
#6518=LINE('',#48364,#7951);
#6519=LINE('',#48370,#7952);
#6520=LINE('',#48376,#7953);
#6521=LINE('',#48382,#7954);
#6522=LINE('',#48388,#7955);
#6523=LINE('',#48394,#7956);
#6524=LINE('',#48400,#7957);
#6525=LINE('',#48406,#7958);
#6526=LINE('',#48412,#7959);
#6527=LINE('',#48418,#7960);
#6528=LINE('',#48424,#7961);
#6529=LINE('',#48430,#7962);
#6530=LINE('',#48436,#7963);
#6531=LINE('',#48444,#7964);
#6532=LINE('',#48449,#7965);
#6533=LINE('',#48457,#7966);
#6534=LINE('',#48461,#7967);
#6535=LINE('',#48469,#7968);
#6536=LINE('',#48475,#7969);
#6537=LINE('',#48478,#7970);
#6538=LINE('',#48484,#7971);
#6539=LINE('',#48492,#7972);
#6540=LINE('',#48496,#7973);
#6541=LINE('',#48500,#7974);
#6542=LINE('',#48506,#7975);
#6543=LINE('',#48509,#7976);
#6544=LINE('',#48515,#7977);
#6545=LINE('',#48521,#7978);
#6546=LINE('',#48526,#7979);
#6547=LINE('',#48528,#7980);
#6548=LINE('',#48530,#7981);
#6549=LINE('',#48531,#7982);
#6550=LINE('',#48537,#7983);
#6551=LINE('',#48540,#7984);
#6552=LINE('',#48542,#7985);
#6553=LINE('',#48543,#7986);
#6554=LINE('',#48549,#7987);
#6555=LINE('',#48552,#7988);
#6556=LINE('',#48554,#7989);
#6557=LINE('',#48555,#7990);
#6558=LINE('',#48561,#7991);
#6559=LINE('',#48564,#7992);
#6560=LINE('',#48566,#7993);
#6561=LINE('',#48567,#7994);
#6562=LINE('',#48577,#7995);
#6563=LINE('',#48595,#7996);
#6564=LINE('',#48612,#7997);
#6565=LINE('',#48660,#7998);
#6566=LINE('',#48708,#7999);
#6567=LINE('',#48756,#8000);
#6568=LINE('',#48810,#8001);
#6569=LINE('',#48858,#8002);
#6570=LINE('',#48906,#8003);
#6571=LINE('',#48960,#8004);
#6572=LINE('',#49008,#8005);
#6573=LINE('',#49056,#8006);
#6574=LINE('',#49104,#8007);
#6575=LINE('',#49158,#8008);
#6576=LINE('',#49206,#8009);
#6577=LINE('',#49254,#8010);
#6578=LINE('',#49308,#8011);
#6579=LINE('',#49356,#8012);
#6580=LINE('',#49404,#8013);
#6581=LINE('',#49452,#8014);
#6582=LINE('',#49506,#8015);
#6583=LINE('',#49554,#8016);
#6584=LINE('',#49602,#8017);
#6585=LINE('',#49656,#8018);
#6586=LINE('',#49703,#8019);
#6587=LINE('',#49723,#8020);
#6588=LINE('',#49748,#8021);
#6589=LINE('',#49773,#8022);
#6590=LINE('',#49797,#8023);
#6591=LINE('',#49822,#8024);
#6592=LINE('',#49847,#8025);
#6593=LINE('',#49871,#8026);
#6594=LINE('',#49895,#8027);
#6595=LINE('',#49920,#8028);
#6596=LINE('',#49945,#8029);
#6597=LINE('',#49969,#8030);
#6598=LINE('',#49994,#8031);
#6599=LINE('',#50019,#8032);
#6600=LINE('',#50043,#8033);
#6601=LINE('',#50067,#8034);
#6602=LINE('',#50092,#8035);
#6603=LINE('',#50117,#8036);
#6604=LINE('',#50141,#8037);
#6605=LINE('',#50166,#8038);
#6606=LINE('',#50191,#8039);
#6607=LINE('',#50215,#8040);
#6608=LINE('',#51703,#8041);
#6609=LINE('',#51708,#8042);
#6610=LINE('',#51710,#8043);
#6611=LINE('',#51712,#8044);
#6612=LINE('',#51713,#8045);
#6613=LINE('',#51716,#8046);
#6614=LINE('',#51718,#8047);
#6615=LINE('',#51719,#8048);
#6616=LINE('',#51722,#8049);
#6617=LINE('',#51724,#8050);
#6618=LINE('',#51725,#8051);
#6619=LINE('',#51728,#8052);
#6620=LINE('',#51730,#8053);
#6621=LINE('',#51731,#8054);
#6622=LINE('',#51734,#8055);
#6623=LINE('',#51736,#8056);
#6624=LINE('',#51737,#8057);
#6625=LINE('',#51739,#8058);
#6626=LINE('',#51740,#8059);
#6627=LINE('',#51745,#8060);
#6628=LINE('',#51747,#8061);
#6629=LINE('',#51749,#8062);
#6630=LINE('',#51750,#8063);
#6631=LINE('',#51754,#8064);
#6632=LINE('',#51757,#8065);
#6633=LINE('',#51758,#8066);
#6634=LINE('',#51764,#8067);
#6635=LINE('',#51766,#8068);
#6636=LINE('',#51768,#8069);
#6637=LINE('',#51769,#8070);
#6638=LINE('',#51773,#8071);
#6639=LINE('',#51776,#8072);
#6640=LINE('',#51777,#8073);
#6641=LINE('',#51783,#8074);
#6642=LINE('',#51785,#8075);
#6643=LINE('',#51787,#8076);
#6644=LINE('',#51788,#8077);
#6645=LINE('',#51792,#8078);
#6646=LINE('',#51795,#8079);
#6647=LINE('',#51796,#8080);
#6648=LINE('',#51802,#8081);
#6649=LINE('',#51804,#8082);
#6650=LINE('',#51806,#8083);
#6651=LINE('',#51807,#8084);
#6652=LINE('',#51811,#8085);
#6653=LINE('',#51814,#8086);
#6654=LINE('',#51815,#8087);
#6655=LINE('',#51821,#8088);
#6656=LINE('',#51823,#8089);
#6657=LINE('',#51825,#8090);
#6658=LINE('',#51826,#8091);
#6659=LINE('',#51830,#8092);
#6660=LINE('',#51833,#8093);
#6661=LINE('',#51834,#8094);
#6662=LINE('',#51840,#8095);
#6663=LINE('',#51842,#8096);
#6664=LINE('',#51844,#8097);
#6665=LINE('',#51845,#8098);
#6666=LINE('',#51849,#8099);
#6667=LINE('',#51852,#8100);
#6668=LINE('',#51853,#8101);
#6669=LINE('',#51859,#8102);
#6670=LINE('',#51861,#8103);
#6671=LINE('',#51863,#8104);
#6672=LINE('',#51864,#8105);
#6673=LINE('',#51868,#8106);
#6674=LINE('',#51871,#8107);
#6675=LINE('',#51872,#8108);
#6676=LINE('',#51878,#8109);
#6677=LINE('',#51880,#8110);
#6678=LINE('',#51882,#8111);
#6679=LINE('',#51883,#8112);
#6680=LINE('',#51887,#8113);
#6681=LINE('',#51890,#8114);
#6682=LINE('',#51891,#8115);
#6683=LINE('',#51897,#8116);
#6684=LINE('',#51899,#8117);
#6685=LINE('',#51901,#8118);
#6686=LINE('',#51902,#8119);
#6687=LINE('',#51907,#8120);
#6688=LINE('',#51911,#8121);
#6689=LINE('',#51912,#8122);
#6690=LINE('',#51920,#8123);
#6691=LINE('',#51922,#8124);
#6692=LINE('',#51924,#8125);
#6693=LINE('',#51925,#8126);
#6694=LINE('',#51929,#8127);
#6695=LINE('',#51932,#8128);
#6696=LINE('',#51933,#8129);
#6697=LINE('',#51939,#8130);
#6698=LINE('',#51941,#8131);
#6699=LINE('',#51943,#8132);
#6700=LINE('',#51944,#8133);
#6701=LINE('',#51948,#8134);
#6702=LINE('',#51951,#8135);
#6703=LINE('',#51952,#8136);
#6704=LINE('',#51958,#8137);
#6705=LINE('',#51960,#8138);
#6706=LINE('',#51962,#8139);
#6707=LINE('',#51963,#8140);
#6708=LINE('',#51967,#8141);
#6709=LINE('',#51970,#8142);
#6710=LINE('',#51971,#8143);
#6711=LINE('',#51977,#8144);
#6712=LINE('',#51979,#8145);
#6713=LINE('',#51981,#8146);
#6714=LINE('',#51982,#8147);
#6715=LINE('',#51986,#8148);
#6716=LINE('',#51989,#8149);
#6717=LINE('',#51990,#8150);
#6718=LINE('',#51996,#8151);
#6719=LINE('',#51998,#8152);
#6720=LINE('',#52000,#8153);
#6721=LINE('',#52001,#8154);
#6722=LINE('',#52005,#8155);
#6723=LINE('',#52008,#8156);
#6724=LINE('',#52009,#8157);
#6725=LINE('',#52015,#8158);
#6726=LINE('',#52017,#8159);
#6727=LINE('',#52019,#8160);
#6728=LINE('',#52020,#8161);
#6729=LINE('',#52024,#8162);
#6730=LINE('',#52027,#8163);
#6731=LINE('',#52028,#8164);
#6732=LINE('',#52034,#8165);
#6733=LINE('',#52036,#8166);
#6734=LINE('',#52038,#8167);
#6735=LINE('',#52039,#8168);
#6736=LINE('',#52043,#8169);
#6737=LINE('',#52046,#8170);
#6738=LINE('',#52047,#8171);
#6739=LINE('',#52053,#8172);
#6740=LINE('',#52055,#8173);
#6741=LINE('',#52057,#8174);
#6742=LINE('',#52058,#8175);
#6743=LINE('',#52062,#8176);
#6744=LINE('',#52065,#8177);
#6745=LINE('',#52066,#8178);
#6746=LINE('',#52072,#8179);
#6747=LINE('',#52074,#8180);
#6748=LINE('',#52076,#8181);
#6749=LINE('',#52077,#8182);
#6750=LINE('',#52081,#8183);
#6751=LINE('',#52084,#8184);
#6752=LINE('',#52085,#8185);
#6753=LINE('',#52091,#8186);
#6754=LINE('',#52093,#8187);
#6755=LINE('',#52095,#8188);
#6756=LINE('',#52096,#8189);
#6757=LINE('',#52100,#8190);
#6758=LINE('',#52103,#8191);
#6759=LINE('',#52104,#8192);
#6760=LINE('',#52110,#8193);
#6761=LINE('',#52112,#8194);
#6762=LINE('',#52114,#8195);
#6763=LINE('',#52115,#8196);
#6764=LINE('',#52119,#8197);
#6765=LINE('',#52122,#8198);
#6766=LINE('',#52123,#8199);
#6767=LINE('',#52129,#8200);
#6768=LINE('',#52131,#8201);
#6769=LINE('',#52133,#8202);
#6770=LINE('',#52134,#8203);
#6771=LINE('',#52138,#8204);
#6772=LINE('',#52141,#8205);
#6773=LINE('',#52142,#8206);
#6774=LINE('',#52148,#8207);
#6775=LINE('',#52150,#8208);
#6776=LINE('',#52152,#8209);
#6777=LINE('',#52153,#8210);
#6778=LINE('',#52157,#8211);
#6779=LINE('',#52160,#8212);
#6780=LINE('',#52161,#8213);
#6781=LINE('',#52167,#8214);
#6782=LINE('',#52169,#8215);
#6783=LINE('',#52171,#8216);
#6784=LINE('',#52172,#8217);
#6785=LINE('',#52176,#8218);
#6786=LINE('',#52179,#8219);
#6787=LINE('',#52180,#8220);
#6788=LINE('',#52186,#8221);
#6789=LINE('',#52188,#8222);
#6790=LINE('',#52190,#8223);
#6791=LINE('',#52191,#8224);
#6792=LINE('',#52195,#8225);
#6793=LINE('',#52198,#8226);
#6794=LINE('',#52199,#8227);
#6795=LINE('',#52205,#8228);
#6796=LINE('',#52207,#8229);
#6797=LINE('',#52209,#8230);
#6798=LINE('',#52210,#8231);
#6799=LINE('',#52214,#8232);
#6800=LINE('',#52217,#8233);
#6801=LINE('',#52218,#8234);
#6802=LINE('',#52224,#8235);
#6803=LINE('',#52226,#8236);
#6804=LINE('',#52228,#8237);
#6805=LINE('',#52229,#8238);
#6806=LINE('',#52233,#8239);
#6807=LINE('',#52236,#8240);
#6808=LINE('',#52237,#8241);
#6809=LINE('',#52245,#8242);
#6810=LINE('',#52246,#8243);
#6811=LINE('',#52249,#8244);
#6812=LINE('',#52251,#8245);
#6813=LINE('',#52252,#8246);
#6814=LINE('',#52255,#8247);
#6815=LINE('',#52256,#8248);
#6816=LINE('',#52262,#8249);
#6817=LINE('',#52264,#8250);
#6818=LINE('',#52266,#8251);
#6819=LINE('',#52267,#8252);
#6820=LINE('',#52271,#8253);
#6821=LINE('',#52274,#8254);
#6822=LINE('',#52275,#8255);
#6823=LINE('',#52281,#8256);
#6824=LINE('',#52283,#8257);
#6825=LINE('',#52285,#8258);
#6826=LINE('',#52286,#8259);
#6827=LINE('',#52290,#8260);
#6828=LINE('',#52293,#8261);
#6829=LINE('',#52294,#8262);
#6830=LINE('',#52300,#8263);
#6831=LINE('',#52302,#8264);
#6832=LINE('',#52304,#8265);
#6833=LINE('',#52305,#8266);
#6834=LINE('',#52309,#8267);
#6835=LINE('',#52312,#8268);
#6836=LINE('',#52313,#8269);
#6837=LINE('',#52319,#8270);
#6838=LINE('',#52321,#8271);
#6839=LINE('',#52323,#8272);
#6840=LINE('',#52324,#8273);
#6841=LINE('',#52328,#8274);
#6842=LINE('',#52331,#8275);
#6843=LINE('',#52332,#8276);
#6844=LINE('',#52338,#8277);
#6845=LINE('',#52340,#8278);
#6846=LINE('',#52342,#8279);
#6847=LINE('',#52343,#8280);
#6848=LINE('',#52347,#8281);
#6849=LINE('',#52350,#8282);
#6850=LINE('',#52351,#8283);
#6851=LINE('',#52357,#8284);
#6852=LINE('',#52359,#8285);
#6853=LINE('',#52361,#8286);
#6854=LINE('',#52362,#8287);
#6855=LINE('',#52366,#8288);
#6856=LINE('',#52369,#8289);
#6857=LINE('',#52370,#8290);
#6858=LINE('',#52376,#8291);
#6859=LINE('',#52378,#8292);
#6860=LINE('',#52380,#8293);
#6861=LINE('',#52381,#8294);
#6862=LINE('',#52385,#8295);
#6863=LINE('',#52388,#8296);
#6864=LINE('',#52389,#8297);
#6865=LINE('',#52395,#8298);
#6866=LINE('',#52397,#8299);
#6867=LINE('',#52399,#8300);
#6868=LINE('',#52400,#8301);
#6869=LINE('',#52404,#8302);
#6870=LINE('',#52407,#8303);
#6871=LINE('',#52408,#8304);
#6872=LINE('',#52414,#8305);
#6873=LINE('',#52416,#8306);
#6874=LINE('',#52418,#8307);
#6875=LINE('',#52419,#8308);
#6876=LINE('',#52423,#8309);
#6877=LINE('',#52426,#8310);
#6878=LINE('',#52427,#8311);
#6879=LINE('',#52434,#8312);
#6880=LINE('',#52438,#8313);
#6881=LINE('',#52456,#8314);
#6882=LINE('',#52480,#8315);
#6883=LINE('',#52486,#8316);
#6884=LINE('',#52514,#8317);
#6885=LINE('',#52552,#8318);
#6886=LINE('',#52590,#8319);
#6887=LINE('',#52627,#8320);
#6888=LINE('',#52664,#8321);
#6889=LINE('',#52702,#8322);
#6890=LINE('',#52740,#8323);
#6891=LINE('',#52779,#8324);
#6892=LINE('',#52812,#8325);
#6893=LINE('',#52896,#8326);
#6894=LINE('',#52986,#8327);
#6895=LINE('',#53076,#8328);
#6896=LINE('',#53160,#8329);
#6897=LINE('',#53250,#8330);
#6898=LINE('',#53340,#8331);
#6899=LINE('',#53424,#8332);
#6900=LINE('',#53514,#8333);
#6901=LINE('',#53534,#8334);
#6902=LINE('',#53572,#8335);
#6903=LINE('',#53609,#8336);
#6904=LINE('',#53646,#8337);
#6905=LINE('',#53684,#8338);
#6906=LINE('',#53721,#8339);
#6907=LINE('',#53758,#8340);
#6908=LINE('',#53796,#8341);
#6909=LINE('',#59007,#8342);
#6910=LINE('',#59037,#8343);
#6911=LINE('',#59042,#8344);
#6912=LINE('',#59045,#8345);
#6913=LINE('',#59051,#8346);
#6914=LINE('',#59065,#8347);
#6915=LINE('',#59075,#8348);
#6916=LINE('',#59087,#8349);
#6917=LINE('',#59091,#8350);
#6918=LINE('',#59096,#8351);
#6919=LINE('',#59101,#8352);
#6920=LINE('',#59106,#8353);
#6921=LINE('',#59110,#8354);
#6922=LINE('',#59115,#8355);
#6923=VECTOR('',#25124,0.635);
#6924=VECTOR('',#25129,0.62);
#6925=VECTOR('',#25158,0.635);
#6926=VECTOR('',#25183,0.635);
#6927=VECTOR('',#25188,0.62);
#6928=VECTOR('',#25193,0.635);
#6929=VECTOR('',#25196,0.635);
#6930=VECTOR('',#25201,0.62);
#6931=VECTOR('',#25206,0.635);
#6932=VECTOR('',#25209,0.635);
#6933=VECTOR('',#25214,0.62);
#6934=VECTOR('',#25219,0.635);
#6935=VECTOR('',#25222,0.635);
#6936=VECTOR('',#25227,0.62);
#6937=VECTOR('',#25232,0.635);
#6938=VECTOR('',#25235,0.635);
#6939=VECTOR('',#25240,0.62);
#6940=VECTOR('',#25245,0.635);
#6941=VECTOR('',#25248,0.635);
#6942=VECTOR('',#25253,0.62);
#6943=VECTOR('',#25258,0.635);
#6944=VECTOR('',#25261,0.635);
#6945=VECTOR('',#25266,0.62);
#6946=VECTOR('',#25271,0.635);
#6947=VECTOR('',#25274,0.635);
#6948=VECTOR('',#25279,0.62);
#6949=VECTOR('',#25284,0.635);
#6950=VECTOR('',#25293,3.425);
#6951=VECTOR('',#25298,3.45);
#6952=VECTOR('',#25301,3.425);
#6953=VECTOR('',#25308,1.49);
#6954=VECTOR('',#25319,1.63);
#6955=VECTOR('',#25324,1.65);
#6956=VECTOR('',#25331,1.275);
#6957=VECTOR('',#25336,1.255);
#6958=VECTOR('',#25341,1.275);
#6959=VECTOR('',#25356,1.);
#6960=VECTOR('',#25357,1.);
#6961=VECTOR('',#25358,1.);
#6962=VECTOR('',#25359,1.);
#6963=VECTOR('',#25360,1.);
#6964=VECTOR('',#25361,1.);
#6965=VECTOR('',#25362,1.);
#6966=VECTOR('',#25365,1.);
#6967=VECTOR('',#25366,1.);
#6968=VECTOR('',#25367,1.);
#6969=VECTOR('',#25368,1.);
#6970=VECTOR('',#25369,1.);
#6971=VECTOR('',#25370,1.);
#6972=VECTOR('',#25371,1.);
#6973=VECTOR('',#25374,1.);
#6974=VECTOR('',#25375,1.);
#6975=VECTOR('',#25386,1.);
#6976=VECTOR('',#25389,1.825);
#6977=VECTOR('',#25396,1.8);
#6978=VECTOR('',#25403,1.);
#6979=VECTOR('',#25418,1.);
#6980=VECTOR('',#25427,1.);
#6981=VECTOR('',#25436,1.);
#6982=VECTOR('',#25437,1.);
#6983=VECTOR('',#25438,1.);
#6984=VECTOR('',#25439,1.);
#6985=VECTOR('',#25442,1.);
#6986=VECTOR('',#25449,1.);
#6987=VECTOR('',#25450,1.);
#6988=VECTOR('',#25451,1.);
#6989=VECTOR('',#25460,1.);
#6990=VECTOR('',#25463,1.);
#6991=VECTOR('',#25466,1.);
#6992=VECTOR('',#25467,1.);
#6993=VECTOR('',#25472,1.);
#6994=VECTOR('',#25477,1.);
#6995=VECTOR('',#25486,1.9);
#6996=VECTOR('',#25493,1.7);
#6997=VECTOR('',#25506,1.98);
#6998=VECTOR('',#25513,2.);
#6999=VECTOR('',#25522,1.98);
#7000=VECTOR('',#25533,1.65);
#7001=VECTOR('',#25536,1.4);
#7002=VECTOR('',#25541,1.475);
#7003=VECTOR('',#25546,1.55);
#7004=VECTOR('',#25551,1.4);
#7005=VECTOR('',#25556,1.25);
#7006=VECTOR('',#25561,1.4);
#7007=VECTOR('',#25570,0.7475);
#7008=VECTOR('',#25575,0.7475);
#7009=VECTOR('',#25578,0.7475);
#7010=VECTOR('',#25581,0.7475);
#7011=VECTOR('',#25584,0.7475);
#7012=VECTOR('',#25587,0.7475);
#7013=VECTOR('',#25590,0.7475);
#7014=VECTOR('',#25593,0.7475);
#7015=VECTOR('',#25608,1.);
#7016=VECTOR('',#25609,1.);
#7017=VECTOR('',#25610,1.);
#7018=VECTOR('',#25611,1.);
#7019=VECTOR('',#25614,1.);
#7020=VECTOR('',#25615,1.);
#7021=VECTOR('',#25616,1.);
#7022=VECTOR('',#25619,1.);
#7023=VECTOR('',#25620,1.);
#7024=VECTOR('',#25621,1.);
#7025=VECTOR('',#25624,1.);
#7026=VECTOR('',#25625,1.);
#7027=VECTOR('',#25626,1.);
#7028=VECTOR('',#25629,1.);
#7029=VECTOR('',#25630,1.);
#7030=VECTOR('',#25631,1.);
#7031=VECTOR('',#25634,1.);
#7032=VECTOR('',#25635,1.);
#7033=VECTOR('',#25640,1.);
#7034=VECTOR('',#25641,1.);
#7035=VECTOR('',#25642,1.);
#7036=VECTOR('',#25643,1.);
#7037=VECTOR('',#25648,1.);
#7038=VECTOR('',#25651,1.);
#7039=VECTOR('',#25652,1.);
#7040=VECTOR('',#25659,1.);
#7041=VECTOR('',#25660,1.);
#7042=VECTOR('',#25661,1.);
#7043=VECTOR('',#25662,1.);
#7044=VECTOR('',#25667,1.);
#7045=VECTOR('',#25670,1.);
#7046=VECTOR('',#25671,1.);
#7047=VECTOR('',#25678,1.);
#7048=VECTOR('',#25679,1.);
#7049=VECTOR('',#25680,1.);
#7050=VECTOR('',#25681,1.);
#7051=VECTOR('',#25686,1.);
#7052=VECTOR('',#25689,1.);
#7053=VECTOR('',#25690,1.);
#7054=VECTOR('',#25697,1.);
#7055=VECTOR('',#25698,1.);
#7056=VECTOR('',#25699,1.);
#7057=VECTOR('',#25700,1.);
#7058=VECTOR('',#25705,1.);
#7059=VECTOR('',#25708,1.);
#7060=VECTOR('',#25709,1.);
#7061=VECTOR('',#25716,1.);
#7062=VECTOR('',#25717,1.);
#7063=VECTOR('',#25718,1.);
#7064=VECTOR('',#25719,1.);
#7065=VECTOR('',#25724,1.);
#7066=VECTOR('',#25727,1.);
#7067=VECTOR('',#25728,1.);
#7068=VECTOR('',#25735,1.);
#7069=VECTOR('',#25736,1.);
#7070=VECTOR('',#25737,1.);
#7071=VECTOR('',#25738,1.);
#7072=VECTOR('',#25743,1.);
#7073=VECTOR('',#25746,1.);
#7074=VECTOR('',#25747,1.);
#7075=VECTOR('',#25754,1.);
#7076=VECTOR('',#25755,1.);
#7077=VECTOR('',#25756,1.);
#7078=VECTOR('',#25757,1.);
#7079=VECTOR('',#25762,1.);
#7080=VECTOR('',#25765,1.);
#7081=VECTOR('',#25766,1.);
#7082=VECTOR('',#25775,1.);
#7083=VECTOR('',#25776,1.);
#7084=VECTOR('',#25779,1.);
#7085=VECTOR('',#25780,1.);
#7086=VECTOR('',#25781,1.);
#7087=VECTOR('',#25784,1.);
#7088=VECTOR('',#25785,1.);
#7089=VECTOR('',#25792,1.);
#7090=VECTOR('',#25793,1.);
#7091=VECTOR('',#25794,1.);
#7092=VECTOR('',#25795,1.);
#7093=VECTOR('',#25800,1.);
#7094=VECTOR('',#25803,1.);
#7095=VECTOR('',#25804,1.);
#7096=VECTOR('',#25811,1.);
#7097=VECTOR('',#25812,1.);
#7098=VECTOR('',#25813,1.);
#7099=VECTOR('',#25814,1.);
#7100=VECTOR('',#25819,1.);
#7101=VECTOR('',#25822,1.);
#7102=VECTOR('',#25823,1.);
#7103=VECTOR('',#25830,1.);
#7104=VECTOR('',#25831,1.);
#7105=VECTOR('',#25832,1.);
#7106=VECTOR('',#25833,1.);
#7107=VECTOR('',#25838,1.);
#7108=VECTOR('',#25841,1.);
#7109=VECTOR('',#25842,1.);
#7110=VECTOR('',#25849,1.);
#7111=VECTOR('',#25850,1.);
#7112=VECTOR('',#25851,1.);
#7113=VECTOR('',#25852,1.);
#7114=VECTOR('',#25857,1.);
#7115=VECTOR('',#25860,1.);
#7116=VECTOR('',#25861,1.);
#7117=VECTOR('',#25868,1.);
#7118=VECTOR('',#25869,1.);
#7119=VECTOR('',#25870,1.);
#7120=VECTOR('',#25871,1.);
#7121=VECTOR('',#25876,1.);
#7122=VECTOR('',#25879,1.);
#7123=VECTOR('',#25880,1.);
#7124=VECTOR('',#25887,1.);
#7125=VECTOR('',#25888,1.);
#7126=VECTOR('',#25889,1.);
#7127=VECTOR('',#25890,1.);
#7128=VECTOR('',#25895,1.);
#7129=VECTOR('',#25898,1.);
#7130=VECTOR('',#25899,1.);
#7131=VECTOR('',#25906,1.);
#7132=VECTOR('',#25907,1.);
#7133=VECTOR('',#25908,1.);
#7134=VECTOR('',#25909,1.);
#7135=VECTOR('',#25914,1.);
#7136=VECTOR('',#25917,1.);
#7137=VECTOR('',#25918,1.);
#7138=VECTOR('',#25925,1.);
#7139=VECTOR('',#25926,1.);
#7140=VECTOR('',#25927,1.);
#7141=VECTOR('',#25928,1.);
#7142=VECTOR('',#25933,1.);
#7143=VECTOR('',#25936,1.);
#7144=VECTOR('',#25937,1.);
#7145=VECTOR('',#25944,1.);
#7146=VECTOR('',#25945,1.);
#7147=VECTOR('',#25946,1.);
#7148=VECTOR('',#25947,1.);
#7149=VECTOR('',#25952,1.);
#7150=VECTOR('',#25955,1.);
#7151=VECTOR('',#25956,1.);
#7152=VECTOR('',#25963,1.);
#7153=VECTOR('',#25964,1.);
#7154=VECTOR('',#25965,1.);
#7155=VECTOR('',#25966,1.);
#7156=VECTOR('',#25971,1.);
#7157=VECTOR('',#25974,1.);
#7158=VECTOR('',#25975,1.);
#7159=VECTOR('',#25982,1.);
#7160=VECTOR('',#25983,1.);
#7161=VECTOR('',#25984,1.);
#7162=VECTOR('',#25985,1.);
#7163=VECTOR('',#25990,1.);
#7164=VECTOR('',#25993,1.);
#7165=VECTOR('',#25994,1.);
#7166=VECTOR('',#26001,1.);
#7167=VECTOR('',#26002,1.);
#7168=VECTOR('',#26003,1.);
#7169=VECTOR('',#26004,1.);
#7170=VECTOR('',#26009,1.);
#7171=VECTOR('',#26012,1.);
#7172=VECTOR('',#26013,1.);
#7173=VECTOR('',#26020,1.);
#7174=VECTOR('',#26021,1.);
#7175=VECTOR('',#26022,1.);
#7176=VECTOR('',#26023,1.);
#7177=VECTOR('',#26028,1.);
#7178=VECTOR('',#26031,1.);
#7179=VECTOR('',#26032,1.);
#7180=VECTOR('',#26039,1.);
#7181=VECTOR('',#26040,1.);
#7182=VECTOR('',#26041,1.);
#7183=VECTOR('',#26042,1.);
#7184=VECTOR('',#26047,1.);
#7185=VECTOR('',#26050,1.);
#7186=VECTOR('',#26051,1.);
#7187=VECTOR('',#26058,1.);
#7188=VECTOR('',#26059,1.);
#7189=VECTOR('',#26060,1.);
#7190=VECTOR('',#26061,1.);
#7191=VECTOR('',#26066,1.);
#7192=VECTOR('',#26071,1.);
#7193=VECTOR('',#26072,1.);
#7194=VECTOR('',#26081,1.);
#7195=VECTOR('',#26082,1.);
#7196=VECTOR('',#26083,1.);
#7197=VECTOR('',#26084,1.);
#7198=VECTOR('',#26089,1.);
#7199=VECTOR('',#26092,1.);
#7200=VECTOR('',#26093,1.);
#7201=VECTOR('',#26100,1.);
#7202=VECTOR('',#26101,1.);
#7203=VECTOR('',#26102,1.);
#7204=VECTOR('',#26103,1.);
#7205=VECTOR('',#26108,1.);
#7206=VECTOR('',#26111,1.);
#7207=VECTOR('',#26112,1.);
#7208=VECTOR('',#26119,1.);
#7209=VECTOR('',#26120,1.);
#7210=VECTOR('',#26121,1.);
#7211=VECTOR('',#26122,1.);
#7212=VECTOR('',#26127,1.);
#7213=VECTOR('',#26130,1.);
#7214=VECTOR('',#26131,1.);
#7215=VECTOR('',#26138,1.);
#7216=VECTOR('',#26139,1.);
#7217=VECTOR('',#26140,1.);
#7218=VECTOR('',#26141,1.);
#7219=VECTOR('',#26146,1.);
#7220=VECTOR('',#26149,1.);
#7221=VECTOR('',#26150,1.);
#7222=VECTOR('',#26157,1.);
#7223=VECTOR('',#26158,1.);
#7224=VECTOR('',#26159,1.);
#7225=VECTOR('',#26160,1.);
#7226=VECTOR('',#26165,1.);
#7227=VECTOR('',#26168,1.);
#7228=VECTOR('',#26169,1.);
#7229=VECTOR('',#26176,1.);
#7230=VECTOR('',#26177,1.);
#7231=VECTOR('',#26178,1.);
#7232=VECTOR('',#26179,1.);
#7233=VECTOR('',#26184,1.);
#7234=VECTOR('',#26187,1.);
#7235=VECTOR('',#26188,1.);
#7236=VECTOR('',#26195,1.);
#7237=VECTOR('',#26196,1.);
#7238=VECTOR('',#26197,1.);
#7239=VECTOR('',#26198,1.);
#7240=VECTOR('',#26203,1.);
#7241=VECTOR('',#26206,1.);
#7242=VECTOR('',#26207,1.);
#7243=VECTOR('',#26216,1.18258529610859);
#7244=VECTOR('',#26219,1.);
#7245=VECTOR('',#26220,1.);
#7246=VECTOR('',#26223,1.);
#7247=VECTOR('',#26226,1.);
#7248=VECTOR('',#26229,1.18258529610859);
#7249=VECTOR('',#26234,1.);
#7250=VECTOR('',#26245,1.);
#7251=VECTOR('',#26252,0.3);
#7252=VECTOR('',#26257,0.3);
#7253=VECTOR('',#26264,0.7931);
#7254=VECTOR('',#26271,0.7431);
#7255=VECTOR('',#26300,0.9);
#7256=VECTOR('',#26339,0.87);
#7257=VECTOR('',#26346,0.57225);
#7258=VECTOR('',#26351,0.57225);
#7259=VECTOR('',#26354,0.57225);
#7260=VECTOR('',#26357,0.57225);
#7261=VECTOR('',#26360,0.57225);
#7262=VECTOR('',#26365,0.7);
#7263=VECTOR('',#26370,0.7);
#7264=VECTOR('',#26373,0.7);
#7265=VECTOR('',#26376,0.7);
#7266=VECTOR('',#26379,0.7);
#7267=VECTOR('',#26382,0.7);
#7268=VECTOR('',#26385,0.7);
#7269=VECTOR('',#26388,0.60685);
#7270=VECTOR('',#26393,0.60685);
#7271=VECTOR('',#26396,0.60685);
#7272=VECTOR('',#26399,0.60685);
#7273=VECTOR('',#26402,0.60685);
#7274=VECTOR('',#26405,0.60685);
#7275=VECTOR('',#26408,0.60685);
#7276=VECTOR('',#26437,1.02473275573014);
#7277=VECTOR('',#26440,1.);
#7278=VECTOR('',#26441,1.);
#7279=VECTOR('',#26444,1.);
#7280=VECTOR('',#26447,1.);
#7281=VECTOR('',#26450,1.02473275573014);
#7282=VECTOR('',#26455,1.);
#7283=VECTOR('',#26472,1.);
#7284=VECTOR('',#26477,0.3);
#7285=VECTOR('',#26484,0.3);
#7286=VECTOR('',#26491,0.61785);
#7287=VECTOR('',#26498,0.56785);
#7288=VECTOR('',#26503,0.67);
#7289=VECTOR('',#26510,0.39);
#7290=VECTOR('',#26517,0.1875);
#7291=VECTOR('',#26522,0.125);
#7292=VECTOR('',#26525,1.);
#7293=VECTOR('',#26526,1.);
#7294=VECTOR('',#26527,1.);
#7295=VECTOR('',#26528,1.);
#7296=VECTOR('',#26533,1.);
#7297=VECTOR('',#26536,1.);
#7298=VECTOR('',#26537,1.);
#7299=VECTOR('',#26538,1.);
#7300=VECTOR('',#26547,1.);
#7301=VECTOR('',#26548,1.);
#7302=VECTOR('',#26549,1.);
#7303=VECTOR('',#26550,1.);
#7304=VECTOR('',#26555,1.);
#7305=VECTOR('',#26558,1.);
#7306=VECTOR('',#26559,1.);
#7307=VECTOR('',#26560,1.);
#7308=VECTOR('',#26575,1.05);
#7309=VECTOR('',#26580,1.1);
#7310=VECTOR('',#26589,1.225);
#7311=VECTOR('',#26594,1.25);
#7312=VECTOR('',#26603,1.195);
#7313=VECTOR('',#26612,1.25);
#7314=VECTOR('',#26621,1.195);
#7315=VECTOR('',#26630,1.25);
#7316=VECTOR('',#26635,1.2);
#7317=VECTOR('',#26650,3.6);
#7318=VECTOR('',#26657,3.7);
#7319=VECTOR('',#26662,1.);
#7320=VECTOR('',#26663,1.);
#7321=VECTOR('',#26664,1.);
#7322=VECTOR('',#26665,1.);
#7323=VECTOR('',#26668,1.);
#7324=VECTOR('',#26669,1.);
#7325=VECTOR('',#26670,1.);
#7326=VECTOR('',#26673,1.);
#7327=VECTOR('',#26674,1.);
#7328=VECTOR('',#26675,1.);
#7329=VECTOR('',#26686,0.35);
#7330=VECTOR('',#26693,0.35);
#7331=VECTOR('',#26700,0.35);
#7332=VECTOR('',#26707,0.35);
#7333=VECTOR('',#26714,0.35);
#7334=VECTOR('',#26721,0.35);
#7335=VECTOR('',#26728,0.35);
#7336=VECTOR('',#26735,0.35);
#7337=VECTOR('',#26742,0.35);
#7338=VECTOR('',#26749,0.601);
#7339=VECTOR('',#26760,0.601);
#7340=VECTOR('',#26771,0.601);
#7341=VECTOR('',#26782,0.601);
#7342=VECTOR('',#26793,0.601);
#7343=VECTOR('',#26804,0.601);
#7344=VECTOR('',#26815,0.601);
#7345=VECTOR('',#26826,0.601);
#7346=VECTOR('',#26837,0.601);
#7347=VECTOR('',#26870,1.7);
#7348=VECTOR('',#26875,1.73);
#7349=VECTOR('',#26878,3.45);
#7350=VECTOR('',#26883,3.7);
#7351=VECTOR('',#26888,3.66);
#7352=VECTOR('',#26899,1.);
#7353=VECTOR('',#26900,1.);
#7354=VECTOR('',#26901,1.);
#7355=VECTOR('',#26902,1.);
#7356=VECTOR('',#26905,1.);
#7357=VECTOR('',#26906,1.);
#7358=VECTOR('',#26907,1.);
#7359=VECTOR('',#26910,1.);
#7360=VECTOR('',#26911,1.);
#7361=VECTOR('',#26912,1.);
#7362=VECTOR('',#26915,1.);
#7363=VECTOR('',#26916,1.);
#7364=VECTOR('',#26917,1.);
#7365=VECTOR('',#26922,1.);
#7366=VECTOR('',#26927,1.);
#7367=VECTOR('',#26928,1.);
#7368=VECTOR('',#26929,1.);
#7369=VECTOR('',#26942,0.4625);
#7370=VECTOR('',#26953,0.45);
#7371=VECTOR('',#26960,0.4625);
#7372=VECTOR('',#26971,0.45);
#7373=VECTOR('',#26978,0.4625);
#7374=VECTOR('',#26989,0.45);
#7375=VECTOR('',#26996,0.4625);
#7376=VECTOR('',#27007,0.45);
#7377=VECTOR('',#27014,0.4625);
#7378=VECTOR('',#27025,0.45);
#7379=VECTOR('',#27032,0.4625);
#7380=VECTOR('',#27043,0.45);
#7381=VECTOR('',#27052,0.7);
#7382=VECTOR('',#27075,0.7);
#7383=VECTOR('',#27098,0.7);
#7384=VECTOR('',#27101,0.7);
#7385=VECTOR('',#27104,0.7);
#7386=VECTOR('',#27107,0.7);
#7387=VECTOR('',#27112,0.70285);
#7388=VECTOR('',#27117,0.66285);
#7389=VECTOR('',#27124,1.25);
#7390=VECTOR('',#27129,1.3);
#7391=VECTOR('',#27136,4.325);
#7392=VECTOR('',#27145,4.3);
#7393=VECTOR('',#27152,2.05);
#7394=VECTOR('',#27161,2.);
#7395=VECTOR('',#27176,5.);
#7396=VECTOR('',#27179,4.1);
#7397=VECTOR('',#27186,3.15);
#7398=VECTOR('',#27189,3.2);
#7399=VECTOR('',#27194,6.95);
#7400=VECTOR('',#27199,7.);
#7401=VECTOR('',#27202,6.975);
#7402=VECTOR('',#27209,4.005);
#7403=VECTOR('',#27218,2.2);
#7404=VECTOR('',#27227,2.6);
#7405=VECTOR('',#27236,2.4);
#7406=VECTOR('',#27247,0.465);
#7407=VECTOR('',#27254,0.45);
#7408=VECTOR('',#27257,1.);
#7409=VECTOR('',#27260,1.);
#7410=VECTOR('',#27281,0.465);
#7411=VECTOR('',#27284,1.);
#7412=VECTOR('',#27287,1.);
#7413=VECTOR('',#27320,0.465);
#7414=VECTOR('',#27327,0.45);
#7415=VECTOR('',#27330,0.465);
#7416=VECTOR('',#27333,0.465);
#7417=VECTOR('',#27340,0.45);
#7418=VECTOR('',#27343,0.465);
#7419=VECTOR('',#27346,0.465);
#7420=VECTOR('',#27353,0.45);
#7421=VECTOR('',#27356,0.465);
#7422=VECTOR('',#27359,0.465);
#7423=VECTOR('',#27366,0.45);
#7424=VECTOR('',#27369,0.465);
#7425=VECTOR('',#27372,0.465);
#7426=VECTOR('',#27379,0.45);
#7427=VECTOR('',#27382,0.465);
#7428=VECTOR('',#27385,0.3);
#7429=VECTOR('',#27390,0.8781);
#7430=VECTOR('',#27397,0.8381);
#7431=VECTOR('',#27400,1.);
#7432=VECTOR('',#27401,1.);
#7433=VECTOR('',#27406,0.8781);
#7434=VECTOR('',#27411,0.8381);
#7435=VECTOR('',#27416,1.);
#7436=VECTOR('',#27417,1.);
#7437=VECTOR('',#27422,0.6);
#7438=VECTOR('',#27423,1.);
#7439=VECTOR('',#27426,1.);
#7440=VECTOR('',#27437,0.6);
#7441=VECTOR('',#27442,1.);
#7442=VECTOR('',#27443,1.);
#7443=VECTOR('',#27464,1.);
#7444=VECTOR('',#27465,0.6);
#7445=VECTOR('',#27468,1.);
#7446=VECTOR('',#27479,0.3);
#7447=VECTOR('',#27486,1.);
#7448=VECTOR('',#27487,1.);
#7449=VECTOR('',#27498,1.);
#7450=VECTOR('',#27505,1.);
#7451=VECTOR('',#27512,1.);
#7452=VECTOR('',#27519,1.);
#7453=VECTOR('',#27526,1.525);
#7454=VECTOR('',#27537,1.5);
#7455=VECTOR('',#27540,1.525);
#7456=VECTOR('',#27553,1.);
#7457=VECTOR('',#27554,1.);
#7458=VECTOR('',#27555,1.);
#7459=VECTOR('',#27556,1.);
#7460=VECTOR('',#27557,1.);
#7461=VECTOR('',#27558,1.);
#7462=VECTOR('',#27559,1.);
#7463=VECTOR('',#27560,1.);
#7464=VECTOR('',#27561,1.);
#7465=VECTOR('',#27562,1.);
#7466=VECTOR('',#27565,1.);
#7467=VECTOR('',#27566,1.);
#7468=VECTOR('',#27567,1.);
#7469=VECTOR('',#27568,1.);
#7470=VECTOR('',#27569,1.);
#7471=VECTOR('',#27572,1.);
#7472=VECTOR('',#27573,1.);
#7473=VECTOR('',#27574,1.);
#7474=VECTOR('',#27575,1.);
#7475=VECTOR('',#27576,1.);
#7476=VECTOR('',#27577,1.);
#7477=VECTOR('',#27578,1.);
#7478=VECTOR('',#27579,1.);
#7479=VECTOR('',#27580,1.);
#7480=VECTOR('',#27581,1.);
#7481=VECTOR('',#27584,1.);
#7482=VECTOR('',#27585,1.);
#7483=VECTOR('',#27586,1.);
#7484=VECTOR('',#27587,1.);
#7485=VECTOR('',#27588,1.);
#7486=VECTOR('',#27589,1.);
#7487=VECTOR('',#27590,1.);
#7488=VECTOR('',#27591,1.);
#7489=VECTOR('',#27592,1.);
#7490=VECTOR('',#27593,1.);
#7491=VECTOR('',#27594,1.);
#7492=VECTOR('',#27595,1.);
#7493=VECTOR('',#27596,1.);
#7494=VECTOR('',#27597,1.);
#7495=VECTOR('',#27598,1.);
#7496=VECTOR('',#27599,1.);
#7497=VECTOR('',#27600,1.);
#7498=VECTOR('',#27601,1.);
#7499=VECTOR('',#27604,1.);
#7500=VECTOR('',#27605,1.);
#7501=VECTOR('',#27608,1.);
#7502=VECTOR('',#27609,1.);
#7503=VECTOR('',#27610,1.);
#7504=VECTOR('',#27611,1.);
#7505=VECTOR('',#27612,1.);
#7506=VECTOR('',#27613,1.);
#7507=VECTOR('',#27614,1.);
#7508=VECTOR('',#27615,1.);
#7509=VECTOR('',#27616,1.);
#7510=VECTOR('',#27617,1.);
#7511=VECTOR('',#27618,1.);
#7512=VECTOR('',#27619,1.);
#7513=VECTOR('',#27620,1.);
#7514=VECTOR('',#27621,1.);
#7515=VECTOR('',#27622,1.);
#7516=VECTOR('',#27623,1.);
#7517=VECTOR('',#27624,1.);
#7518=VECTOR('',#27625,1.);
#7519=VECTOR('',#27626,1.);
#7520=VECTOR('',#27627,1.);
#7521=VECTOR('',#27630,1.);
#7522=VECTOR('',#27631,1.);
#7523=VECTOR('',#27632,1.);
#7524=VECTOR('',#27635,1.);
#7525=VECTOR('',#27636,1.);
#7526=VECTOR('',#27637,1.);
#7527=VECTOR('',#27638,1.);
#7528=VECTOR('',#27639,1.);
#7529=VECTOR('',#27642,1.);
#7530=VECTOR('',#27643,1.);
#7531=VECTOR('',#27644,1.);
#7532=VECTOR('',#27647,1.);
#7533=VECTOR('',#27648,1.);
#7534=VECTOR('',#27649,1.);
#7535=VECTOR('',#27652,1.);
#7536=VECTOR('',#27653,1.);
#7537=VECTOR('',#27654,1.);
#7538=VECTOR('',#27657,1.);
#7539=VECTOR('',#27658,1.);
#7540=VECTOR('',#27663,1.);
#7541=VECTOR('',#27664,1.);
#7542=VECTOR('',#27665,1.);
#7543=VECTOR('',#27666,1.);
#7544=VECTOR('',#27669,1.);
#7545=VECTOR('',#27670,1.);
#7546=VECTOR('',#27671,1.);
#7547=VECTOR('',#27674,1.);
#7548=VECTOR('',#27675,1.);
#7549=VECTOR('',#27676,1.);
#7550=VECTOR('',#27679,1.);
#7551=VECTOR('',#27680,1.);
#7552=VECTOR('',#27681,1.);
#7553=VECTOR('',#27684,1.);
#7554=VECTOR('',#27685,1.);
#7555=VECTOR('',#27686,1.);
#7556=VECTOR('',#27689,1.);
#7557=VECTOR('',#27690,1.);
#7558=VECTOR('',#27691,1.);
#7559=VECTOR('',#27694,1.);
#7560=VECTOR('',#27695,1.);
#7561=VECTOR('',#27696,1.);
#7562=VECTOR('',#27699,1.);
#7563=VECTOR('',#27700,1.);
#7564=VECTOR('',#27701,1.);
#7565=VECTOR('',#27702,1.);
#7566=VECTOR('',#27703,1.);
#7567=VECTOR('',#27706,1.);
#7568=VECTOR('',#27707,1.);
#7569=VECTOR('',#27708,1.);
#7570=VECTOR('',#27711,1.);
#7571=VECTOR('',#27712,1.);
#7572=VECTOR('',#27713,1.);
#7573=VECTOR('',#27716,1.);
#7574=VECTOR('',#27717,1.);
#7575=VECTOR('',#27718,1.);
#7576=VECTOR('',#27721,1.);
#7577=VECTOR('',#27722,1.);
#7578=VECTOR('',#27723,1.);
#7579=VECTOR('',#27726,1.);
#7580=VECTOR('',#27727,1.);
#7581=VECTOR('',#27730,1.);
#7582=VECTOR('',#27731,1.);
#7583=VECTOR('',#27732,1.);
#7584=VECTOR('',#27733,1.);
#7585=VECTOR('',#27734,1.);
#7586=VECTOR('',#27735,1.);
#7587=VECTOR('',#27736,1.);
#7588=VECTOR('',#27737,1.);
#7589=VECTOR('',#27738,1.);
#7590=VECTOR('',#27739,1.);
#7591=VECTOR('',#27740,1.);
#7592=VECTOR('',#27741,1.);
#7593=VECTOR('',#27744,1.);
#7594=VECTOR('',#27745,1.);
#7595=VECTOR('',#27746,1.);
#7596=VECTOR('',#27747,1.);
#7597=VECTOR('',#27748,1.);
#7598=VECTOR('',#27749,1.);
#7599=VECTOR('',#27750,1.);
#7600=VECTOR('',#27751,1.);
#7601=VECTOR('',#27752,1.);
#7602=VECTOR('',#27753,1.);
#7603=VECTOR('',#27756,1.);
#7604=VECTOR('',#27757,1.);
#7605=VECTOR('',#27758,1.);
#7606=VECTOR('',#27759,1.);
#7607=VECTOR('',#27760,1.);
#7608=VECTOR('',#27761,1.);
#7609=VECTOR('',#27762,1.);
#7610=VECTOR('',#27763,1.);
#7611=VECTOR('',#27764,1.);
#7612=VECTOR('',#27765,1.);
#7613=VECTOR('',#27768,1.);
#7614=VECTOR('',#27769,1.);
#7615=VECTOR('',#27770,1.);
#7616=VECTOR('',#27771,1.);
#7617=VECTOR('',#27776,1.);
#7618=VECTOR('',#27777,1.);
#7619=VECTOR('',#27778,1.);
#7620=VECTOR('',#27779,1.);
#7621=VECTOR('',#27782,1.);
#7622=VECTOR('',#27783,1.);
#7623=VECTOR('',#27784,1.);
#7624=VECTOR('',#27787,1.);
#7625=VECTOR('',#27788,1.);
#7626=VECTOR('',#27789,1.);
#7627=VECTOR('',#27792,1.);
#7628=VECTOR('',#27793,1.);
#7629=VECTOR('',#27796,1.);
#7630=VECTOR('',#27797,1.);
#7631=VECTOR('',#27798,1.);
#7632=VECTOR('',#27801,1.);
#7633=VECTOR('',#27802,1.);
#7634=VECTOR('',#27803,1.);
#7635=VECTOR('',#27806,1.);
#7636=VECTOR('',#27807,1.);
#7637=VECTOR('',#27808,1.);
#7638=VECTOR('',#27811,1.);
#7639=VECTOR('',#27812,1.);
#7640=VECTOR('',#27815,1.);
#7641=VECTOR('',#27816,1.);
#7642=VECTOR('',#27817,1.);
#7643=VECTOR('',#27818,1.);
#7644=VECTOR('',#27821,1.);
#7645=VECTOR('',#27822,1.);
#7646=VECTOR('',#27823,1.);
#7647=VECTOR('',#27826,1.);
#7648=VECTOR('',#27827,1.);
#7649=VECTOR('',#27828,1.);
#7650=VECTOR('',#27831,1.);
#7651=VECTOR('',#27832,1.);
#7652=VECTOR('',#27833,1.);
#7653=VECTOR('',#27836,1.);
#7654=VECTOR('',#27837,1.);
#7655=VECTOR('',#27838,1.);
#7656=VECTOR('',#27841,1.);
#7657=VECTOR('',#27842,1.);
#7658=VECTOR('',#27843,1.);
#7659=VECTOR('',#27846,1.);
#7660=VECTOR('',#27847,1.);
#7661=VECTOR('',#27848,1.);
#7662=VECTOR('',#27851,1.);
#7663=VECTOR('',#27852,1.);
#7664=VECTOR('',#27855,1.);
#7665=VECTOR('',#27856,1.);
#7666=VECTOR('',#27857,1.);
#7667=VECTOR('',#27858,1.);
#7668=VECTOR('',#27859,1.);
#7669=VECTOR('',#27860,1.);
#7670=VECTOR('',#27861,1.);
#7671=VECTOR('',#27862,1.);
#7672=VECTOR('',#27863,1.);
#7673=VECTOR('',#27864,1.);
#7674=VECTOR('',#27865,1.);
#7675=VECTOR('',#27866,1.);
#7676=VECTOR('',#27867,1.);
#7677=VECTOR('',#27868,1.);
#7678=VECTOR('',#27871,1.);
#7679=VECTOR('',#27872,1.);
#7680=VECTOR('',#27873,1.);
#7681=VECTOR('',#27874,1.);
#7682=VECTOR('',#27875,1.);
#7683=VECTOR('',#27876,1.);
#7684=VECTOR('',#27877,1.);
#7685=VECTOR('',#27878,1.);
#7686=VECTOR('',#27879,1.);
#7687=VECTOR('',#27880,1.);
#7688=VECTOR('',#27881,1.);
#7689=VECTOR('',#27882,1.);
#7690=VECTOR('',#27883,1.);
#7691=VECTOR('',#27884,1.);
#7692=VECTOR('',#27885,1.);
#7693=VECTOR('',#27886,1.);
#7694=VECTOR('',#27887,1.);
#7695=VECTOR('',#27888,1.);
#7696=VECTOR('',#27889,1.);
#7697=VECTOR('',#27890,1.);
#7698=VECTOR('',#27891,1.);
#7699=VECTOR('',#27894,1.);
#7700=VECTOR('',#27895,1.);
#7701=VECTOR('',#27896,1.);
#7702=VECTOR('',#27897,1.);
#7703=VECTOR('',#27900,1.);
#7704=VECTOR('',#27901,1.);
#7705=VECTOR('',#27902,1.);
#7706=VECTOR('',#27903,1.);
#7707=VECTOR('',#27904,1.);
#7708=VECTOR('',#27905,1.);
#7709=VECTOR('',#27906,1.);
#7710=VECTOR('',#27907,1.);
#7711=VECTOR('',#27908,1.);
#7712=VECTOR('',#27909,1.);
#7713=VECTOR('',#27910,1.);
#7714=VECTOR('',#27911,1.);
#7715=VECTOR('',#27914,1.);
#7716=VECTOR('',#27915,1.);
#7717=VECTOR('',#27916,1.);
#7718=VECTOR('',#27917,1.);
#7719=VECTOR('',#27918,1.);
#7720=VECTOR('',#27919,1.);
#7721=VECTOR('',#27920,1.);
#7722=VECTOR('',#27921,1.);
#7723=VECTOR('',#27922,1.);
#7724=VECTOR('',#27923,1.);
#7725=VECTOR('',#27926,1.);
#7726=VECTOR('',#27927,1.);
#7727=VECTOR('',#27928,1.);
#7728=VECTOR('',#27929,1.);
#7729=VECTOR('',#27930,1.);
#7730=VECTOR('',#27931,1.);
#7731=VECTOR('',#27932,1.);
#7732=VECTOR('',#27933,1.);
#7733=VECTOR('',#27934,1.);
#7734=VECTOR('',#27935,1.);
#7735=VECTOR('',#27938,1.);
#7736=VECTOR('',#27939,1.);
#7737=VECTOR('',#27940,1.);
#7738=VECTOR('',#27941,1.);
#7739=VECTOR('',#27944,1.);
#7740=VECTOR('',#27945,1.);
#7741=VECTOR('',#27946,1.);
#7742=VECTOR('',#27947,1.);
#7743=VECTOR('',#27948,1.);
#7744=VECTOR('',#27949,1.);
#7745=VECTOR('',#27950,1.);
#7746=VECTOR('',#27951,1.);
#7747=VECTOR('',#27952,1.);
#7748=VECTOR('',#27955,1.);
#7749=VECTOR('',#27956,1.);
#7750=VECTOR('',#27957,1.);
#7751=VECTOR('',#27958,1.);
#7752=VECTOR('',#27959,1.);
#7753=VECTOR('',#27960,1.);
#7754=VECTOR('',#27961,1.);
#7755=VECTOR('',#27962,1.);
#7756=VECTOR('',#27963,1.);
#7757=VECTOR('',#27964,1.);
#7758=VECTOR('',#27965,1.);
#7759=VECTOR('',#27966,1.);
#7760=VECTOR('',#27969,1.);
#7761=VECTOR('',#27970,1.);
#7762=VECTOR('',#27971,1.);
#7763=VECTOR('',#27974,1.);
#7764=VECTOR('',#27975,1.);
#7765=VECTOR('',#27976,1.);
#7766=VECTOR('',#27979,1.);
#7767=VECTOR('',#27980,1.);
#7768=VECTOR('',#27981,1.);
#7769=VECTOR('',#27986,1.);
#7770=VECTOR('',#27987,1.);
#7771=VECTOR('',#27988,1.);
#7772=VECTOR('',#27989,1.);
#7773=VECTOR('',#27990,1.);
#7774=VECTOR('',#27991,1.);
#7775=VECTOR('',#27992,1.);
#7776=VECTOR('',#27993,1.);
#7777=VECTOR('',#27994,1.);
#7778=VECTOR('',#27997,1.);
#7779=VECTOR('',#27998,1.);
#7780=VECTOR('',#27999,1.);
#7781=VECTOR('',#28002,1.);
#7782=VECTOR('',#28003,1.);
#7783=VECTOR('',#28006,1.);
#7784=VECTOR('',#28007,1.);
#7785=VECTOR('',#28008,1.);
#7786=VECTOR('',#28009,1.);
#7787=VECTOR('',#28010,1.);
#7788=VECTOR('',#28011,1.);
#7789=VECTOR('',#28012,1.);
#7790=VECTOR('',#28013,1.);
#7791=VECTOR('',#28014,1.);
#7792=VECTOR('',#28015,1.);
#7793=VECTOR('',#28018,1.);
#7794=VECTOR('',#28019,1.);
#7795=VECTOR('',#28020,1.);
#7796=VECTOR('',#28023,1.);
#7797=VECTOR('',#28024,1.);
#7798=VECTOR('',#28025,1.);
#7799=VECTOR('',#28028,1.);
#7800=VECTOR('',#28029,1.);
#7801=VECTOR('',#28030,1.);
#7802=VECTOR('',#28033,1.);
#7803=VECTOR('',#28034,1.);
#7804=VECTOR('',#28037,1.);
#7805=VECTOR('',#28038,1.);
#7806=VECTOR('',#28039,1.);
#7807=VECTOR('',#28040,1.);
#7808=VECTOR('',#28041,1.);
#7809=VECTOR('',#28042,1.);
#7810=VECTOR('',#28043,1.);
#7811=VECTOR('',#28044,1.);
#7812=VECTOR('',#28045,1.);
#7813=VECTOR('',#28046,1.);
#7814=VECTOR('',#28047,1.);
#7815=VECTOR('',#28048,1.);
#7816=VECTOR('',#28049,1.);
#7817=VECTOR('',#28050,1.);
#7818=VECTOR('',#28051,1.);
#7819=VECTOR('',#28052,1.);
#7820=VECTOR('',#28053,1.);
#7821=VECTOR('',#28054,1.);
#7822=VECTOR('',#28055,1.);
#7823=VECTOR('',#28056,1.);
#7824=VECTOR('',#28057,1.);
#7825=VECTOR('',#28058,1.);
#7826=VECTOR('',#28059,1.);
#7827=VECTOR('',#28060,1.);
#7828=VECTOR('',#28061,1.);
#7829=VECTOR('',#28062,1.);
#7830=VECTOR('',#28065,1.);
#7831=VECTOR('',#28066,1.);
#7832=VECTOR('',#28067,1.);
#7833=VECTOR('',#28068,1.);
#7834=VECTOR('',#28071,1.);
#7835=VECTOR('',#28072,1.);
#7836=VECTOR('',#28073,1.);
#7837=VECTOR('',#28074,1.);
#7838=VECTOR('',#28075,1.);
#7839=VECTOR('',#28076,1.);
#7840=VECTOR('',#28077,1.);
#7841=VECTOR('',#28078,1.);
#7842=VECTOR('',#28079,1.);
#7843=VECTOR('',#28080,1.);
#7844=VECTOR('',#28081,1.);
#7845=VECTOR('',#28082,1.);
#7846=VECTOR('',#28083,1.);
#7847=VECTOR('',#28084,1.);
#7848=VECTOR('',#28085,1.);
#7849=VECTOR('',#28086,1.);
#7850=VECTOR('',#28089,1.);
#7851=VECTOR('',#28090,1.);
#7852=VECTOR('',#28091,1.);
#7853=VECTOR('',#28094,1.);
#7854=VECTOR('',#28095,1.);
#7855=VECTOR('',#28096,1.);
#7856=VECTOR('',#28099,1.);
#7857=VECTOR('',#28100,1.);
#7858=VECTOR('',#28101,1.);
#7859=VECTOR('',#28104,1.);
#7860=VECTOR('',#28105,1.);
#7861=VECTOR('',#28106,1.);
#7862=VECTOR('',#28109,1.);
#7863=VECTOR('',#28110,1.);
#7864=VECTOR('',#28111,1.);
#7865=VECTOR('',#28114,1.);
#7866=VECTOR('',#28115,1.);
#7867=VECTOR('',#28116,1.);
#7868=VECTOR('',#28117,1.);
#7869=VECTOR('',#28118,1.);
#7870=VECTOR('',#28121,1.);
#7871=VECTOR('',#28122,1.);
#7872=VECTOR('',#28123,1.);
#7873=VECTOR('',#28124,1.);
#7874=VECTOR('',#28125,1.);
#7875=VECTOR('',#28126,1.);
#7876=VECTOR('',#28129,1.);
#7877=VECTOR('',#28130,1.);
#7878=VECTOR('',#28131,1.);
#7879=VECTOR('',#28134,1.);
#7880=VECTOR('',#28135,1.);
#7881=VECTOR('',#28136,1.);
#7882=VECTOR('',#28139,1.);
#7883=VECTOR('',#28140,1.);
#7884=VECTOR('',#28141,1.);
#7885=VECTOR('',#28144,1.);
#7886=VECTOR('',#28145,1.);
#7887=VECTOR('',#28146,1.);
#7888=VECTOR('',#28149,1.);
#7889=VECTOR('',#28150,1.);
#7890=VECTOR('',#28169,0.3);
#7891=VECTOR('',#28174,0.8781);
#7892=VECTOR('',#28181,0.8381);
#7893=VECTOR('',#28184,1.);
#7894=VECTOR('',#28185,1.);
#7895=VECTOR('',#28186,1.);
#7896=VECTOR('',#28189,0.25);
#7897=VECTOR('',#28194,0.5);
#7898=VECTOR('',#28195,0.5);
#7899=VECTOR('',#28208,7.);
#7900=VECTOR('',#28223,0.429999999999999);
#7901=VECTOR('',#28244,0.404999999999999);
#7902=VECTOR('',#28249,0.429999999999999);
#7903=VECTOR('',#28254,0.404999999999999);
#7904=VECTOR('',#28259,0.43);
#7905=VECTOR('',#28264,0.405);
#7906=VECTOR('',#28269,0.429999999999999);
#7907=VECTOR('',#28274,0.404999999999999);
#7908=VECTOR('',#28279,0.43);
#7909=VECTOR('',#28284,0.405);
#7910=VECTOR('',#28289,0.429999999999999);
#7911=VECTOR('',#28294,0.404999999999999);
#7912=VECTOR('',#28299,0.404999999999999);
#7913=VECTOR('',#28302,0.405);
#7914=VECTOR('',#28305,0.404999999999999);
#7915=VECTOR('',#28308,0.405);
#7916=VECTOR('',#28311,0.404999999999999);
#7917=VECTOR('',#28314,0.404999999999999);
#7918=VECTOR('',#28317,2.63);
#7919=VECTOR('',#28326,2.6);
#7920=VECTOR('',#28331,6.975);
#7921=VECTOR('',#28338,2.4);
#7922=VECTOR('',#28355,0.575);
#7923=VECTOR('',#28362,0.6);
#7924=VECTOR('',#28373,0.575);
#7925=VECTOR('',#28380,0.6);
#7926=VECTOR('',#28387,0.3);
#7927=VECTOR('',#28394,0.42);
#7928=VECTOR('',#28397,0.57);
#7929=VECTOR('',#28402,0.6);
#7930=VECTOR('',#28407,0.57);
#7931=VECTOR('',#28414,0.25);
#7932=VECTOR('',#28419,0.1625);
#7933=VECTOR('',#28424,0.075);
#7934=VECTOR('',#28437,0.59);
#7935=VECTOR('',#28444,0.65);
#7936=VECTOR('',#28463,0.075);
#7937=VECTOR('',#28472,0.4);
#7938=VECTOR('',#28481,0.78);
#7939=VECTOR('',#28486,0.8);
#7940=VECTOR('',#28491,0.78);
#7941=VECTOR('',#28500,0.55);
#7942=VECTOR('',#28505,0.53);
#7943=VECTOR('',#28514,1.88899277133291);
#7944=VECTOR('',#28589,1.96724457939162);
#7945=VECTOR('',#28662,2.06222171593972);
#7946=VECTOR('',#28665,1.79401563478481);
#7947=VECTOR('',#29078,1.);
#7948=VECTOR('',#29087,1.61107777577792);
#7949=VECTOR('',#29128,1.);
#7950=VECTOR('',#29137,1.);
#7951=VECTOR('',#29146,1.);
#7952=VECTOR('',#29155,1.);
#7953=VECTOR('',#29164,1.);
#7954=VECTOR('',#29173,1.);
#7955=VECTOR('',#29182,1.);
#7956=VECTOR('',#29191,1.);
#7957=VECTOR('',#29200,1.);
#7958=VECTOR('',#29209,1.);
#7959=VECTOR('',#29218,1.);
#7960=VECTOR('',#29227,1.);
#7961=VECTOR('',#29236,1.);
#7962=VECTOR('',#29245,1.);
#7963=VECTOR('',#29254,1.);
#7964=VECTOR('',#29267,1.);
#7965=VECTOR('',#29272,1.28);
#7966=VECTOR('',#29283,1.87);
#7967=VECTOR('',#29288,1.9);
#7968=VECTOR('',#29299,1.6);
#7969=VECTOR('',#29306,1.28);
#7970=VECTOR('',#29311,1.25);
#7971=VECTOR('',#29318,2.40256617975257);
#7972=VECTOR('',#29329,2.57);
#7973=VECTOR('',#29334,2.6);
#7974=VECTOR('',#29339,2.57);
#7975=VECTOR('',#29346,2.09090617619859);
#7976=VECTOR('',#29351,2.22173617797558);
#7977=VECTOR('',#29358,0.1);
#7978=VECTOR('',#29365,0.1);
#7979=VECTOR('',#29370,1.);
#7980=VECTOR('',#29371,1.);
#7981=VECTOR('',#29372,1.);
#7982=VECTOR('',#29373,1.);
#7983=VECTOR('',#29380,1.);
#7984=VECTOR('',#29383,1.);
#7985=VECTOR('',#29384,1.);
#7986=VECTOR('',#29385,1.);
#7987=VECTOR('',#29392,1.);
#7988=VECTOR('',#29395,1.);
#7989=VECTOR('',#29396,1.);
#7990=VECTOR('',#29397,1.);
#7991=VECTOR('',#29404,1.);
#7992=VECTOR('',#29407,1.);
#7993=VECTOR('',#29408,1.);
#7994=VECTOR('',#29409,1.);
#7995=VECTOR('',#29424,0.4);
#7996=VECTOR('',#29427,0.4);
#7997=VECTOR('',#29434,0.4);
#7998=VECTOR('',#29437,0.4);
#7999=VECTOR('',#29440,0.4);
#8000=VECTOR('',#29443,0.4);
#8001=VECTOR('',#29446,0.4);
#8002=VECTOR('',#29449,0.4);
#8003=VECTOR('',#29452,0.4);
#8004=VECTOR('',#29455,0.4);
#8005=VECTOR('',#29458,0.4);
#8006=VECTOR('',#29461,0.4);
#8007=VECTOR('',#29464,0.4);
#8008=VECTOR('',#29467,0.4);
#8009=VECTOR('',#29470,0.4);
#8010=VECTOR('',#29473,0.4);
#8011=VECTOR('',#29476,0.4);
#8012=VECTOR('',#29479,0.4);
#8013=VECTOR('',#29482,0.4);
#8014=VECTOR('',#29485,0.4);
#8015=VECTOR('',#29488,0.4);
#8016=VECTOR('',#29491,0.4);
#8017=VECTOR('',#29494,0.4);
#8018=VECTOR('',#29497,0.4);
#8019=VECTOR('',#29502,0.322275);
#8020=VECTOR('',#29507,0.322275);
#8021=VECTOR('',#29510,0.322275);
#8022=VECTOR('',#29513,0.322275);
#8023=VECTOR('',#29516,0.322275);
#8024=VECTOR('',#29519,0.322275);
#8025=VECTOR('',#29522,0.322275);
#8026=VECTOR('',#29525,0.322275);
#8027=VECTOR('',#29528,0.322275);
#8028=VECTOR('',#29531,0.322275);
#8029=VECTOR('',#29534,0.322275);
#8030=VECTOR('',#29537,0.322275);
#8031=VECTOR('',#29540,0.322275);
#8032=VECTOR('',#29543,0.322275);
#8033=VECTOR('',#29546,0.322275);
#8034=VECTOR('',#29549,0.322275);
#8035=VECTOR('',#29552,0.322275);
#8036=VECTOR('',#29555,0.322275);
#8037=VECTOR('',#29558,0.322275);
#8038=VECTOR('',#29561,0.322275);
#8039=VECTOR('',#29564,0.322275);
#8040=VECTOR('',#29567,0.322275);
#8041=VECTOR('',#29594,0.149995599935465);
#8042=VECTOR('',#29599,1.);
#8043=VECTOR('',#29600,1.);
#8044=VECTOR('',#29601,1.);
#8045=VECTOR('',#29602,1.);
#8046=VECTOR('',#29605,1.);
#8047=VECTOR('',#29606,1.);
#8048=VECTOR('',#29607,1.);
#8049=VECTOR('',#29610,1.);
#8050=VECTOR('',#29611,1.);
#8051=VECTOR('',#29612,1.);
#8052=VECTOR('',#29615,1.);
#8053=VECTOR('',#29616,1.);
#8054=VECTOR('',#29617,1.);
#8055=VECTOR('',#29620,1.);
#8056=VECTOR('',#29621,1.);
#8057=VECTOR('',#29622,1.);
#8058=VECTOR('',#29625,1.);
#8059=VECTOR('',#29626,1.);
#8060=VECTOR('',#29631,1.);
#8061=VECTOR('',#29632,1.);
#8062=VECTOR('',#29633,1.);
#8063=VECTOR('',#29634,1.);
#8064=VECTOR('',#29639,1.);
#8065=VECTOR('',#29642,1.);
#8066=VECTOR('',#29643,1.);
#8067=VECTOR('',#29650,1.);
#8068=VECTOR('',#29651,1.);
#8069=VECTOR('',#29652,1.);
#8070=VECTOR('',#29653,1.);
#8071=VECTOR('',#29658,1.);
#8072=VECTOR('',#29661,1.);
#8073=VECTOR('',#29662,1.);
#8074=VECTOR('',#29669,1.);
#8075=VECTOR('',#29670,1.);
#8076=VECTOR('',#29671,1.);
#8077=VECTOR('',#29672,1.);
#8078=VECTOR('',#29677,1.);
#8079=VECTOR('',#29680,1.);
#8080=VECTOR('',#29681,1.);
#8081=VECTOR('',#29688,1.);
#8082=VECTOR('',#29689,1.);
#8083=VECTOR('',#29690,1.);
#8084=VECTOR('',#29691,1.);
#8085=VECTOR('',#29696,1.);
#8086=VECTOR('',#29699,1.);
#8087=VECTOR('',#29700,1.);
#8088=VECTOR('',#29707,1.);
#8089=VECTOR('',#29708,1.);
#8090=VECTOR('',#29709,1.);
#8091=VECTOR('',#29710,1.);
#8092=VECTOR('',#29715,1.);
#8093=VECTOR('',#29718,1.);
#8094=VECTOR('',#29719,1.);
#8095=VECTOR('',#29726,1.);
#8096=VECTOR('',#29727,1.);
#8097=VECTOR('',#29728,1.);
#8098=VECTOR('',#29729,1.);
#8099=VECTOR('',#29734,1.);
#8100=VECTOR('',#29737,1.);
#8101=VECTOR('',#29738,1.);
#8102=VECTOR('',#29745,1.);
#8103=VECTOR('',#29746,1.);
#8104=VECTOR('',#29747,1.);
#8105=VECTOR('',#29748,1.);
#8106=VECTOR('',#29753,1.);
#8107=VECTOR('',#29756,1.);
#8108=VECTOR('',#29757,1.);
#8109=VECTOR('',#29764,1.);
#8110=VECTOR('',#29765,1.);
#8111=VECTOR('',#29766,1.);
#8112=VECTOR('',#29767,1.);
#8113=VECTOR('',#29772,1.);
#8114=VECTOR('',#29775,1.);
#8115=VECTOR('',#29776,1.);
#8116=VECTOR('',#29783,1.);
#8117=VECTOR('',#29784,1.);
#8118=VECTOR('',#29785,1.);
#8119=VECTOR('',#29786,1.);
#8120=VECTOR('',#29791,1.);
#8121=VECTOR('',#29796,1.);
#8122=VECTOR('',#29797,1.);
#8123=VECTOR('',#29806,1.);
#8124=VECTOR('',#29807,1.);
#8125=VECTOR('',#29808,1.);
#8126=VECTOR('',#29809,1.);
#8127=VECTOR('',#29814,1.);
#8128=VECTOR('',#29817,1.);
#8129=VECTOR('',#29818,1.);
#8130=VECTOR('',#29825,1.);
#8131=VECTOR('',#29826,1.);
#8132=VECTOR('',#29827,1.);
#8133=VECTOR('',#29828,1.);
#8134=VECTOR('',#29833,1.);
#8135=VECTOR('',#29836,1.);
#8136=VECTOR('',#29837,1.);
#8137=VECTOR('',#29844,1.);
#8138=VECTOR('',#29845,1.);
#8139=VECTOR('',#29846,1.);
#8140=VECTOR('',#29847,1.);
#8141=VECTOR('',#29852,1.);
#8142=VECTOR('',#29855,1.);
#8143=VECTOR('',#29856,1.);
#8144=VECTOR('',#29863,1.);
#8145=VECTOR('',#29864,1.);
#8146=VECTOR('',#29865,1.);
#8147=VECTOR('',#29866,1.);
#8148=VECTOR('',#29871,1.);
#8149=VECTOR('',#29874,1.);
#8150=VECTOR('',#29875,1.);
#8151=VECTOR('',#29882,1.);
#8152=VECTOR('',#29883,1.);
#8153=VECTOR('',#29884,1.);
#8154=VECTOR('',#29885,1.);
#8155=VECTOR('',#29890,1.);
#8156=VECTOR('',#29893,1.);
#8157=VECTOR('',#29894,1.);
#8158=VECTOR('',#29901,1.);
#8159=VECTOR('',#29902,1.);
#8160=VECTOR('',#29903,1.);
#8161=VECTOR('',#29904,1.);
#8162=VECTOR('',#29909,1.);
#8163=VECTOR('',#29912,1.);
#8164=VECTOR('',#29913,1.);
#8165=VECTOR('',#29920,1.);
#8166=VECTOR('',#29921,1.);
#8167=VECTOR('',#29922,1.);
#8168=VECTOR('',#29923,1.);
#8169=VECTOR('',#29928,1.);
#8170=VECTOR('',#29931,1.);
#8171=VECTOR('',#29932,1.);
#8172=VECTOR('',#29939,1.);
#8173=VECTOR('',#29940,1.);
#8174=VECTOR('',#29941,1.);
#8175=VECTOR('',#29942,1.);
#8176=VECTOR('',#29947,1.);
#8177=VECTOR('',#29950,1.);
#8178=VECTOR('',#29951,1.);
#8179=VECTOR('',#29958,1.);
#8180=VECTOR('',#29959,1.);
#8181=VECTOR('',#29960,1.);
#8182=VECTOR('',#29961,1.);
#8183=VECTOR('',#29966,1.);
#8184=VECTOR('',#29969,1.);
#8185=VECTOR('',#29970,1.);
#8186=VECTOR('',#29977,1.);
#8187=VECTOR('',#29978,1.);
#8188=VECTOR('',#29979,1.);
#8189=VECTOR('',#29980,1.);
#8190=VECTOR('',#29985,1.);
#8191=VECTOR('',#29988,1.);
#8192=VECTOR('',#29989,1.);
#8193=VECTOR('',#29996,1.);
#8194=VECTOR('',#29997,1.);
#8195=VECTOR('',#29998,1.);
#8196=VECTOR('',#29999,1.);
#8197=VECTOR('',#30004,1.);
#8198=VECTOR('',#30007,1.);
#8199=VECTOR('',#30008,1.);
#8200=VECTOR('',#30015,1.);
#8201=VECTOR('',#30016,1.);
#8202=VECTOR('',#30017,1.);
#8203=VECTOR('',#30018,1.);
#8204=VECTOR('',#30023,1.);
#8205=VECTOR('',#30026,1.);
#8206=VECTOR('',#30027,1.);
#8207=VECTOR('',#30034,1.);
#8208=VECTOR('',#30035,1.);
#8209=VECTOR('',#30036,1.);
#8210=VECTOR('',#30037,1.);
#8211=VECTOR('',#30042,1.);
#8212=VECTOR('',#30045,1.);
#8213=VECTOR('',#30046,1.);
#8214=VECTOR('',#30053,1.);
#8215=VECTOR('',#30054,1.);
#8216=VECTOR('',#30055,1.);
#8217=VECTOR('',#30056,1.);
#8218=VECTOR('',#30061,1.);
#8219=VECTOR('',#30064,1.);
#8220=VECTOR('',#30065,1.);
#8221=VECTOR('',#30072,1.);
#8222=VECTOR('',#30073,1.);
#8223=VECTOR('',#30074,1.);
#8224=VECTOR('',#30075,1.);
#8225=VECTOR('',#30080,1.);
#8226=VECTOR('',#30083,1.);
#8227=VECTOR('',#30084,1.);
#8228=VECTOR('',#30091,1.);
#8229=VECTOR('',#30092,1.);
#8230=VECTOR('',#30093,1.);
#8231=VECTOR('',#30094,1.);
#8232=VECTOR('',#30099,1.);
#8233=VECTOR('',#30102,1.);
#8234=VECTOR('',#30103,1.);
#8235=VECTOR('',#30110,1.);
#8236=VECTOR('',#30111,1.);
#8237=VECTOR('',#30112,1.);
#8238=VECTOR('',#30113,1.);
#8239=VECTOR('',#30118,1.);
#8240=VECTOR('',#30121,1.);
#8241=VECTOR('',#30122,1.);
#8242=VECTOR('',#30131,1.);
#8243=VECTOR('',#30132,1.);
#8244=VECTOR('',#30135,1.);
#8245=VECTOR('',#30136,1.);
#8246=VECTOR('',#30137,1.);
#8247=VECTOR('',#30140,1.);
#8248=VECTOR('',#30141,1.);
#8249=VECTOR('',#30148,1.);
#8250=VECTOR('',#30149,1.);
#8251=VECTOR('',#30150,1.);
#8252=VECTOR('',#30151,1.);
#8253=VECTOR('',#30156,1.);
#8254=VECTOR('',#30159,1.);
#8255=VECTOR('',#30160,1.);
#8256=VECTOR('',#30167,1.);
#8257=VECTOR('',#30168,1.);
#8258=VECTOR('',#30169,1.);
#8259=VECTOR('',#30170,1.);
#8260=VECTOR('',#30175,1.);
#8261=VECTOR('',#30178,1.);
#8262=VECTOR('',#30179,1.);
#8263=VECTOR('',#30186,1.);
#8264=VECTOR('',#30187,1.);
#8265=VECTOR('',#30188,1.);
#8266=VECTOR('',#30189,1.);
#8267=VECTOR('',#30194,1.);
#8268=VECTOR('',#30197,1.);
#8269=VECTOR('',#30198,1.);
#8270=VECTOR('',#30205,1.);
#8271=VECTOR('',#30206,1.);
#8272=VECTOR('',#30207,1.);
#8273=VECTOR('',#30208,1.);
#8274=VECTOR('',#30213,1.);
#8275=VECTOR('',#30216,1.);
#8276=VECTOR('',#30217,1.);
#8277=VECTOR('',#30224,1.);
#8278=VECTOR('',#30225,1.);
#8279=VECTOR('',#30226,1.);
#8280=VECTOR('',#30227,1.);
#8281=VECTOR('',#30232,1.);
#8282=VECTOR('',#30235,1.);
#8283=VECTOR('',#30236,1.);
#8284=VECTOR('',#30243,1.);
#8285=VECTOR('',#30244,1.);
#8286=VECTOR('',#30245,1.);
#8287=VECTOR('',#30246,1.);
#8288=VECTOR('',#30251,1.);
#8289=VECTOR('',#30254,1.);
#8290=VECTOR('',#30255,1.);
#8291=VECTOR('',#30262,1.);
#8292=VECTOR('',#30263,1.);
#8293=VECTOR('',#30264,1.);
#8294=VECTOR('',#30265,1.);
#8295=VECTOR('',#30270,1.);
#8296=VECTOR('',#30273,1.);
#8297=VECTOR('',#30274,1.);
#8298=VECTOR('',#30281,1.);
#8299=VECTOR('',#30282,1.);
#8300=VECTOR('',#30283,1.);
#8301=VECTOR('',#30284,1.);
#8302=VECTOR('',#30289,1.);
#8303=VECTOR('',#30292,1.);
#8304=VECTOR('',#30293,1.);
#8305=VECTOR('',#30300,1.);
#8306=VECTOR('',#30301,1.);
#8307=VECTOR('',#30302,1.);
#8308=VECTOR('',#30303,1.);
#8309=VECTOR('',#30308,1.);
#8310=VECTOR('',#30311,1.);
#8311=VECTOR('',#30312,1.);
#8312=VECTOR('',#30323,0.37);
#8313=VECTOR('',#30328,0.63);
#8314=VECTOR('',#30363,0.65);
#8315=VECTOR('',#30408,0.62);
#8316=VECTOR('',#30415,0.7475);
#8317=VECTOR('',#30420,0.7475);
#8318=VECTOR('',#30423,0.7475);
#8319=VECTOR('',#30426,0.7475);
#8320=VECTOR('',#30429,0.7475);
#8321=VECTOR('',#30432,0.7475);
#8322=VECTOR('',#30435,0.7475);
#8323=VECTOR('',#30438,0.7475);
#8324=VECTOR('',#30443,0.8);
#8325=VECTOR('',#30448,0.8);
#8326=VECTOR('',#30451,0.8);
#8327=VECTOR('',#30454,0.8);
#8328=VECTOR('',#30457,0.8);
#8329=VECTOR('',#30460,0.8);
#8330=VECTOR('',#30463,0.8);
#8331=VECTOR('',#30466,0.8);
#8332=VECTOR('',#30469,0.8);
#8333=VECTOR('',#30472,0.70685);
#8334=VECTOR('',#30477,0.70685);
#8335=VECTOR('',#30480,0.70685);
#8336=VECTOR('',#30483,0.70685);
#8337=VECTOR('',#30486,0.70685);
#8338=VECTOR('',#30489,0.70685);
#8339=VECTOR('',#30492,0.70685);
#8340=VECTOR('',#30495,0.70685);
#8341=VECTOR('',#30498,0.70685);
#8342=VECTOR('',#30527,1.18258529610859);
#8343=VECTOR('',#30530,1.);
#8344=VECTOR('',#30531,1.);
#8345=VECTOR('',#30534,1.);
#8346=VECTOR('',#30537,1.);
#8347=VECTOR('',#30540,1.18258529610859);
#8348=VECTOR('',#30545,1.);
#8349=VECTOR('',#30562,1.);
#8350=VECTOR('',#30567,0.4);
#8351=VECTOR('',#30574,0.4);
#8352=VECTOR('',#30581,0.7931);
#8353=VECTOR('',#30588,0.7431);
#8354=VECTOR('',#30593,0.77);
#8355=VECTOR('',#30600,0.49);
#8356=CIRCLE('',#23048,0.65);
#8357=CIRCLE('',#23049,0.62);
#8358=CIRCLE('',#23051,0.62);
#8359=CIRCLE('',#23053,3.4);
#8360=CIRCLE('',#23054,0.65);
#8361=CIRCLE('',#23055,0.65);
#8362=CIRCLE('',#23056,0.65);
#8363=CIRCLE('',#23057,0.65);
#8364=CIRCLE('',#23058,1.57765648986083);
#8365=CIRCLE('',#23059,0.65);
#8366=CIRCLE('',#23060,0.65);
#8367=CIRCLE('',#23061,0.65);
#8368=CIRCLE('',#23062,0.65);
#8369=CIRCLE('',#23064,0.65);
#8370=CIRCLE('',#23066,3.4);
#8371=CIRCLE('',#23067,0.65);
#8372=CIRCLE('',#23068,0.65);
#8373=CIRCLE('',#23069,0.65);
#8374=CIRCLE('',#23070,0.65);
#8375=CIRCLE('',#23071,1.60499221181911);
#8376=CIRCLE('',#23072,0.65);
#8377=CIRCLE('',#23073,0.65);
#8378=CIRCLE('',#23074,0.65);
#8379=CIRCLE('',#23075,0.65);
#8380=CIRCLE('',#23077,0.62);
#8381=CIRCLE('',#23079,0.62);
#8382=CIRCLE('',#23082,0.62);
#8383=CIRCLE('',#23084,0.62);
#8384=CIRCLE('',#23087,0.62);
#8385=CIRCLE('',#23089,0.62);
#8386=CIRCLE('',#23092,0.62);
#8387=CIRCLE('',#23094,0.62);
#8388=CIRCLE('',#23097,0.62);
#8389=CIRCLE('',#23099,0.62);
#8390=CIRCLE('',#23102,0.62);
#8391=CIRCLE('',#23104,0.62);
#8392=CIRCLE('',#23107,0.62);
#8393=CIRCLE('',#23109,0.62);
#8394=CIRCLE('',#23112,0.62);
#8395=CIRCLE('',#23114,0.62);
#8396=CIRCLE('',#23117,1.605);
#8397=CIRCLE('',#23119,3.45);
#8398=CIRCLE('',#23121,3.45);
#8399=CIRCLE('',#23125,1.49);
#8400=CIRCLE('',#23126,1.49);
#8401=CIRCLE('',#23128,1.61);
#8402=CIRCLE('',#23130,1.65);
#8403=CIRCLE('',#23132,1.65);
#8404=CIRCLE('',#23134,1.295);
#8405=CIRCLE('',#23136,1.255);
#8406=CIRCLE('',#23138,1.255);
#8407=CIRCLE('',#23140,1.295);
#8408=CIRCLE('',#23142,1.48323969741913);
#8409=CIRCLE('',#23144,1.6);
#8410=CIRCLE('',#23150,3.92);
#8411=CIRCLE('',#23151,1.85);
#8412=CIRCLE('',#23153,4.);
#8413=CIRCLE('',#23155,1.8);
#8414=CIRCLE('',#23156,1.8);
#8415=CIRCLE('',#23160,3.6);
#8416=CIRCLE('',#23162,4.);
#8417=CIRCLE('',#23164,3.94);
#8418=CIRCLE('',#23169,0.15);
#8419=CIRCLE('',#23170,0.15);
#8420=CIRCLE('',#23173,0.15);
#8421=CIRCLE('',#23177,0.37);
#8422=CIRCLE('',#23178,0.4);
#8423=CIRCLE('',#23181,0.37);
#8424=CIRCLE('',#23182,0.4);
#8425=CIRCLE('',#23184,0.4);
#8426=CIRCLE('',#23188,0.4);
#8427=CIRCLE('',#23193,1.9);
#8428=CIRCLE('',#23194,1.9);
#8429=CIRCLE('',#23196,1.7);
#8430=CIRCLE('',#23197,1.7);
#8431=CIRCLE('',#23200,1.4);
#8432=CIRCLE('',#23202,1.96);
#8433=CIRCLE('',#23203,2.);
#8434=CIRCLE('',#23204,2.);
#8435=CIRCLE('',#23206,2.);
#8436=CIRCLE('',#23207,2.);
#8437=CIRCLE('',#23210,1.96);
#8438=CIRCLE('',#23212,1.65);
#8439=CIRCLE('',#23214,1.65);
#8440=CIRCLE('',#23216,1.4);
#8441=CIRCLE('',#23218,1.55);
#8442=CIRCLE('',#23220,1.55);
#8443=CIRCLE('',#23222,1.25);
#8444=CIRCLE('',#23224,1.25);
#8445=CIRCLE('',#23226,1.55);
#8446=CIRCLE('',#23230,0.7475);
#8447=CIRCLE('',#23238,0.7475);
#8448=CIRCLE('',#23240,0.82685);
#8449=CIRCLE('',#23241,0.82685);
#8450=CIRCLE('',#23242,0.7475);
#8451=CIRCLE('',#23253,0.9);
#8452=CIRCLE('',#23256,0.9);
#8453=CIRCLE('',#23259,0.9);
#8454=CIRCLE('',#23262,0.9);
#8455=CIRCLE('',#23265,0.9);
#8456=CIRCLE('',#23268,0.9);
#8457=CIRCLE('',#23271,0.9);
#8458=CIRCLE('',#23274,0.9);
#8459=CIRCLE('',#23277,0.9);
#8460=CIRCLE('',#23280,0.9);
#8461=CIRCLE('',#23283,0.9);
#8462=CIRCLE('',#23286,0.9);
#8463=CIRCLE('',#23289,0.9);
#8464=CIRCLE('',#23292,0.9);
#8465=CIRCLE('',#23294,0.9);
#8466=CIRCLE('',#23298,0.9);
#8467=CIRCLE('',#23301,0.9);
#8468=CIRCLE('',#23304,0.9);
#8469=CIRCLE('',#23307,0.9);
#8470=CIRCLE('',#23310,0.9);
#8471=CIRCLE('',#23313,0.9);
#8472=CIRCLE('',#23316,0.9);
#8473=CIRCLE('',#23319,0.9);
#8474=CIRCLE('',#23322,0.9);
#8475=CIRCLE('',#23325,0.9);
#8476=CIRCLE('',#23328,0.9);
#8477=CIRCLE('',#23331,0.9);
#8478=CIRCLE('',#23334,0.9);
#8479=CIRCLE('',#23337,0.9);
#8480=CIRCLE('',#23340,0.9);
#8481=CIRCLE('',#23343,0.9);
#8482=CIRCLE('',#23346,0.9);
#8483=CIRCLE('',#23349,0.9);
#8484=CIRCLE('',#23352,0.9);
#8485=CIRCLE('',#23355,0.9);
#8486=CIRCLE('',#23358,0.9);
#8487=CIRCLE('',#23361,0.9);
#8488=CIRCLE('',#23364,0.9);
#8489=CIRCLE('',#23367,0.9);
#8490=CIRCLE('',#23370,0.9);
#8491=CIRCLE('',#23373,0.9);
#8492=CIRCLE('',#23376,0.9);
#8493=CIRCLE('',#23379,0.9);
#8494=CIRCLE('',#23382,0.9);
#8495=CIRCLE('',#23385,0.9);
#8496=CIRCLE('',#23386,0.9);
#8497=CIRCLE('',#23389,0.9);
#8498=CIRCLE('',#23390,0.9);
#8499=CIRCLE('',#23393,0.9);
#8500=CIRCLE('',#23396,0.9);
#8501=CIRCLE('',#23399,0.9);
#8502=CIRCLE('',#23402,0.9);
#8503=CIRCLE('',#23405,0.9);
#8504=CIRCLE('',#23408,0.9);
#8505=CIRCLE('',#23411,0.9);
#8506=CIRCLE('',#23414,0.9);
#8507=CIRCLE('',#23417,0.9);
#8508=CIRCLE('',#23420,0.9);
#8509=CIRCLE('',#23423,0.9);
#8510=CIRCLE('',#23426,0.9);
#8511=CIRCLE('',#23429,0.9);
#8512=CIRCLE('',#23432,0.9);
#8513=CIRCLE('',#23434,1.045);
#8514=CIRCLE('',#23439,1.045);
#8515=CIRCLE('',#23442,0.9);
#8516=CIRCLE('',#23444,0.7431);
#8517=CIRCLE('',#23448,0.3);
#8518=CIRCLE('',#23449,0.3);
#8519=CIRCLE('',#23452,0.7531);
#8520=CIRCLE('',#23455,0.7431);
#8521=CIRCLE('',#23458,0.9);
#8522=CIRCLE('',#23459,0.9);
#8523=CIRCLE('',#23460,0.9);
#8524=CIRCLE('',#23461,0.9);
#8525=CIRCLE('',#23462,0.9);
#8526=CIRCLE('',#23463,0.9);
#8527=CIRCLE('',#23464,0.9);
#8528=CIRCLE('',#23465,0.9);
#8529=CIRCLE('',#23466,0.9);
#8530=CIRCLE('',#23467,0.9);
#8531=CIRCLE('',#23468,0.9);
#8532=CIRCLE('',#23469,0.9);
#8533=CIRCLE('',#23470,0.9);
#8534=CIRCLE('',#23471,0.9);
#8535=CIRCLE('',#23472,0.9);
#8536=CIRCLE('',#23473,0.9);
#8537=CIRCLE('',#23474,0.9);
#8538=CIRCLE('',#23475,0.9);
#8539=CIRCLE('',#23476,0.9);
#8540=CIRCLE('',#23477,0.9);
#8541=CIRCLE('',#23478,0.9);
#8542=CIRCLE('',#23479,0.9);
#8543=CIRCLE('',#23480,0.9);
#8544=CIRCLE('',#23481,0.9);
#8545=CIRCLE('',#23482,0.9);
#8546=CIRCLE('',#23483,0.9);
#8547=CIRCLE('',#23484,0.9);
#8548=CIRCLE('',#23485,0.9);
#8549=CIRCLE('',#23486,0.9);
#8550=CIRCLE('',#23487,0.9);
#8551=CIRCLE('',#23489,0.84);
#8552=CIRCLE('',#23493,0.57225);
#8553=CIRCLE('',#23498,0.57225);
#8554=CIRCLE('',#23500,0.6925);
#8555=CIRCLE('',#23508,0.60685);
#8556=CIRCLE('',#23516,0.6925);
#8557=CIRCLE('',#23517,0.6925);
#8558=CIRCLE('',#23519,0.60685);
#8559=CIRCLE('',#23521,0.6925);
#8560=CIRCLE('',#23523,0.6516);
#8561=CIRCLE('',#23524,0.6516);
#8562=CIRCLE('',#23525,0.57225);
#8563=CIRCLE('',#23528,0.9025);
#8564=CIRCLE('',#23533,0.9025);
#8565=CIRCLE('',#23537,0.3);
#8566=CIRCLE('',#23539,0.56785);
#8567=CIRCLE('',#23541,0.3);
#8568=CIRCLE('',#23545,0.3);
#8569=CIRCLE('',#23547,0.3);
#8570=CIRCLE('',#23549,0.57785);
#8571=CIRCLE('',#23552,0.56785);
#8572=CIRCLE('',#23555,0.64);
#8573=CIRCLE('',#23557,0.48);
#8574=CIRCLE('',#23561,0.24404761904762);
#8575=CIRCLE('',#23562,0.125);
#8576=CIRCLE('',#23566,0.3);
#8577=CIRCLE('',#23569,0.3);
#8578=CIRCLE('',#23573,0.4);
#8579=CIRCLE('',#23576,0.4);
#8580=CIRCLE('',#23579,1.);
#8581=CIRCLE('',#23581,1.1);
#8582=CIRCLE('',#23583,1.1);
#8583=CIRCLE('',#23585,1.2);
#8584=CIRCLE('',#23587,1.25);
#8585=CIRCLE('',#23589,1.25);
#8586=CIRCLE('',#23591,1.195);
#8587=CIRCLE('',#23593,1.195);
#8588=CIRCLE('',#23595,1.25);
#8589=CIRCLE('',#23597,1.25);
#8590=CIRCLE('',#23599,1.195);
#8591=CIRCLE('',#23601,1.195);
#8592=CIRCLE('',#23603,1.25);
#8593=CIRCLE('',#23605,1.25);
#8594=CIRCLE('',#23607,1.15);
#8595=CIRCLE('',#23611,3.7);
#8596=CIRCLE('',#23612,3.6);
#8597=CIRCLE('',#23614,3.6);
#8598=CIRCLE('',#23616,3.7);
#8599=CIRCLE('',#23618,3.7);
#8600=CIRCLE('',#23623,1.7);
#8601=CIRCLE('',#23624,1.252);
#8602=CIRCLE('',#23626,0.35);
#8603=CIRCLE('',#23627,0.35);
#8604=CIRCLE('',#23629,0.35);
#8605=CIRCLE('',#23630,0.35);
#8606=CIRCLE('',#23632,0.35);
#8607=CIRCLE('',#23633,0.35);
#8608=CIRCLE('',#23635,0.35);
#8609=CIRCLE('',#23636,0.35);
#8610=CIRCLE('',#23638,0.35);
#8611=CIRCLE('',#23639,0.35);
#8612=CIRCLE('',#23641,0.35);
#8613=CIRCLE('',#23642,0.35);
#8614=CIRCLE('',#23644,0.35);
#8615=CIRCLE('',#23645,0.35);
#8616=CIRCLE('',#23647,0.35);
#8617=CIRCLE('',#23648,0.35);
#8618=CIRCLE('',#23650,0.35);
#8619=CIRCLE('',#23651,0.35);
#8620=CIRCLE('',#23653,0.601);
#8621=CIRCLE('',#23654,0.601);
#8622=CIRCLE('',#23655,0.601);
#8623=CIRCLE('',#23658,0.601);
#8624=CIRCLE('',#23659,0.601);
#8625=CIRCLE('',#23660,0.601);
#8626=CIRCLE('',#23663,0.601);
#8627=CIRCLE('',#23664,0.601);
#8628=CIRCLE('',#23665,0.601);
#8629=CIRCLE('',#23668,0.601);
#8630=CIRCLE('',#23669,0.601);
#8631=CIRCLE('',#23670,0.601);
#8632=CIRCLE('',#23673,0.601);
#8633=CIRCLE('',#23674,0.601);
#8634=CIRCLE('',#23675,0.601);
#8635=CIRCLE('',#23678,0.601);
#8636=CIRCLE('',#23679,0.601);
#8637=CIRCLE('',#23680,0.601);
#8638=CIRCLE('',#23683,0.601);
#8639=CIRCLE('',#23684,0.601);
#8640=CIRCLE('',#23685,0.601);
#8641=CIRCLE('',#23688,0.601);
#8642=CIRCLE('',#23689,0.601);
#8643=CIRCLE('',#23690,0.601);
#8644=CIRCLE('',#23693,0.601);
#8645=CIRCLE('',#23694,0.601);
#8646=CIRCLE('',#23695,0.601);
#8647=CIRCLE('',#23698,3.2);
#8648=CIRCLE('',#23699,3.2);
#8649=CIRCLE('',#23700,3.2);
#8650=CIRCLE('',#23701,3.2);
#8651=CIRCLE('',#23702,3.2);
#8652=CIRCLE('',#23703,3.2);
#8653=CIRCLE('',#23704,3.2);
#8654=CIRCLE('',#23705,3.2);
#8655=CIRCLE('',#23706,3.2);
#8656=CIRCLE('',#23707,3.2);
#8657=CIRCLE('',#23708,1.76);
#8658=CIRCLE('',#23710,1.7);
#8659=CIRCLE('',#23714,3.7);
#8660=CIRCLE('',#23716,3.62);
#8661=CIRCLE('',#23718,1.252);
#8662=CIRCLE('',#23726,2.56);
#8663=CIRCLE('',#23727,2.56);
#8664=CIRCLE('',#23730,2.84);
#8665=CIRCLE('',#23731,2.84);
#8666=CIRCLE('',#23734,0.475000000000001);
#8667=CIRCLE('',#23735,0.45);
#8668=CIRCLE('',#23736,0.45);
#8669=CIRCLE('',#23738,0.7);
#8670=CIRCLE('',#23740,0.45);
#8671=CIRCLE('',#23742,0.475);
#8672=CIRCLE('',#23743,0.45);
#8673=CIRCLE('',#23744,0.45);
#8674=CIRCLE('',#23746,0.7);
#8675=CIRCLE('',#23748,0.45);
#8676=CIRCLE('',#23750,0.475);
#8677=CIRCLE('',#23751,0.45);
#8678=CIRCLE('',#23752,0.45);
#8679=CIRCLE('',#23754,0.7);
#8680=CIRCLE('',#23756,0.45);
#8681=CIRCLE('',#23758,0.475000000000001);
#8682=CIRCLE('',#23759,0.45);
#8683=CIRCLE('',#23760,0.45);
#8684=CIRCLE('',#23762,0.7);
#8685=CIRCLE('',#23764,0.45);
#8686=CIRCLE('',#23766,0.475);
#8687=CIRCLE('',#23767,0.45);
#8688=CIRCLE('',#23768,0.45);
#8689=CIRCLE('',#23770,0.7);
#8690=CIRCLE('',#23772,0.45);
#8691=CIRCLE('',#23774,0.475);
#8692=CIRCLE('',#23775,0.45);
#8693=CIRCLE('',#23776,0.45);
#8694=CIRCLE('',#23778,0.7);
#8695=CIRCLE('',#23780,0.45);
#8696=CIRCLE('',#23782,0.7);
#8697=CIRCLE('',#23783,0.7);
#8698=CIRCLE('',#23785,5.);
#8699=CIRCLE('',#23786,0.4);
#8700=CIRCLE('',#23787,5.4);
#8701=CIRCLE('',#23788,5.4);
#8702=CIRCLE('',#23789,5.4);
#8703=CIRCLE('',#23790,5.4);
#8704=CIRCLE('',#23791,5.4);
#8705=CIRCLE('',#23792,5.4);
#8706=CIRCLE('',#23794,0.7);
#8707=CIRCLE('',#23795,0.7);
#8708=CIRCLE('',#23797,6.9);
#8709=CIRCLE('',#23798,0.7);
#8710=CIRCLE('',#23799,0.7);
#8711=CIRCLE('',#23800,0.7);
#8712=CIRCLE('',#23801,0.7);
#8713=CIRCLE('',#23802,0.7);
#8714=CIRCLE('',#23803,0.7);
#8715=CIRCLE('',#23804,0.7);
#8716=CIRCLE('',#23810,0.74285);
#8717=CIRCLE('',#23811,0.66285);
#8718=CIRCLE('',#23814,1.2);
#8719=CIRCLE('',#23816,1.3);
#8720=CIRCLE('',#23819,4.3);
#8721=CIRCLE('',#23820,4.3);
#8722=CIRCLE('',#23821,4.35);
#8723=CIRCLE('',#23823,6.95);
#8724=CIRCLE('',#23825,4.3);
#8725=CIRCLE('',#23827,2.1);
#8726=CIRCLE('',#23828,2.);
#8727=CIRCLE('',#23829,2.);
#8728=CIRCLE('',#23831,2.);
#8729=CIRCLE('',#23833,3.1);
#8730=CIRCLE('',#23835,5.);
#8731=CIRCLE('',#23836,0.6);
#8732=CIRCLE('',#23837,4.74223748569721);
#8733=CIRCLE('',#23840,3.2);
#8734=CIRCLE('',#23842,3.2);
#8735=CIRCLE('',#23845,7.);
#8736=CIRCLE('',#23847,7.);
#8737=CIRCLE('',#23850,4.005);
#8738=CIRCLE('',#23852,4.005);
#8739=CIRCLE('',#23854,2.2);
#8740=CIRCLE('',#23856,2.2);
#8741=CIRCLE('',#23858,2.6);
#8742=CIRCLE('',#23860,2.6);
#8743=CIRCLE('',#23862,2.4);
#8744=CIRCLE('',#23864,2.4);
#8745=CIRCLE('',#23868,0.48);
#8746=CIRCLE('',#23869,0.45);
#8747=CIRCLE('',#23871,0.45);
#8748=CIRCLE('',#23873,6.9);
#8749=CIRCLE('',#23874,6.9);
#8750=CIRCLE('',#23875,0.48);
#8751=CIRCLE('',#23876,0.48);
#8752=CIRCLE('',#23877,0.48);
#8753=CIRCLE('',#23878,1.55);
#8754=CIRCLE('',#23879,0.3);
#8755=CIRCLE('',#23880,0.48);
#8756=CIRCLE('',#23881,0.48);
#8757=CIRCLE('',#23883,0.48);
#8758=CIRCLE('',#23885,6.9);
#8759=CIRCLE('',#23886,6.9);
#8760=CIRCLE('',#23887,0.48);
#8761=CIRCLE('',#23888,0.48);
#8762=CIRCLE('',#23889,0.48);
#8763=CIRCLE('',#23890,2.25);
#8764=CIRCLE('',#23891,0.35);
#8765=CIRCLE('',#23892,2.95);
#8766=CIRCLE('',#23893,0.35);
#8767=CIRCLE('',#23894,2.25);
#8768=CIRCLE('',#23895,0.35);
#8769=CIRCLE('',#23896,2.95);
#8770=CIRCLE('',#23897,0.35);
#8771=CIRCLE('',#23898,1.55);
#8772=CIRCLE('',#23899,0.48);
#8773=CIRCLE('',#23900,0.48);
#8774=CIRCLE('',#23902,0.45);
#8775=CIRCLE('',#23904,0.45);
#8776=CIRCLE('',#23907,0.45);
#8777=CIRCLE('',#23909,0.45);
#8778=CIRCLE('',#23912,0.45);
#8779=CIRCLE('',#23914,0.45);
#8780=CIRCLE('',#23917,0.45);
#8781=CIRCLE('',#23919,0.45);
#8782=CIRCLE('',#23922,0.45);
#8783=CIRCLE('',#23924,0.45);
#8784=CIRCLE('',#23928,0.9181);
#8785=CIRCLE('',#23929,0.8381);
#8786=CIRCLE('',#23931,0.8381);
#8787=CIRCLE('',#23934,0.9181);
#8788=CIRCLE('',#23935,0.8381);
#8789=CIRCLE('',#23937,0.8381);
#8790=CIRCLE('',#23940,0.6);
#8791=CIRCLE('',#23941,0.6);
#8792=CIRCLE('',#23943,0.6);
#8793=CIRCLE('',#23944,0.6);
#8794=CIRCLE('',#23948,2.25);
#8795=CIRCLE('',#23949,2.25);
#8796=CIRCLE('',#23951,2.95);
#8797=CIRCLE('',#23952,0.35);
#8798=CIRCLE('',#23954,7.);
#8799=CIRCLE('',#23956,7.);
#8800=CIRCLE('',#23959,0.6);
#8801=CIRCLE('',#23960,0.6);
#8802=CIRCLE('',#23962,0.6);
#8803=CIRCLE('',#23963,0.6);
#8804=CIRCLE('',#23967,2.25);
#8805=CIRCLE('',#23968,2.25);
#8806=CIRCLE('',#23970,2.95);
#8807=CIRCLE('',#23971,0.35);
#8808=CIRCLE('',#23973,0.35);
#8809=CIRCLE('',#23975,2.95);
#8810=CIRCLE('',#23979,0.35);
#8811=CIRCLE('',#23981,2.95);
#8812=CIRCLE('',#23985,1.5);
#8813=CIRCLE('',#23986,1.5);
#8814=CIRCLE('',#23988,1.5);
#8815=CIRCLE('',#23989,1.5);
#8816=CIRCLE('',#23992,7.);
#8817=CIRCLE('',#23994,7.);
#8818=CIRCLE('',#24087,0.3);
#8819=CIRCLE('',#24089,0.9181);
#8820=CIRCLE('',#24090,0.8381);
#8821=CIRCLE('',#24092,0.8381);
#8822=CIRCLE('',#24095,0.5);
#8823=CIRCLE('',#24097,0.5);
#8824=CIRCLE('',#24100,7.);
#8825=CIRCLE('',#24102,7.);
#8826=CIRCLE('',#24103,7.);
#8827=CIRCLE('',#24104,7.);
#8828=CIRCLE('',#24106,6.3);
#8829=CIRCLE('',#24107,0.7);
#8830=CIRCLE('',#24109,0.454999999999999);
#8831=CIRCLE('',#24110,0.404999999999999);
#8832=CIRCLE('',#24112,6.95);
#8833=CIRCLE('',#24113,0.455);
#8834=CIRCLE('',#24114,0.455);
#8835=CIRCLE('',#24115,2.66);
#8836=CIRCLE('',#24116,0.454999999999999);
#8837=CIRCLE('',#24117,0.454999999999999);
#8838=CIRCLE('',#24118,0.454999999999999);
#8839=CIRCLE('',#24120,0.404999999999999);
#8840=CIRCLE('',#24122,0.404999999999999);
#8841=CIRCLE('',#24124,0.404999999999999);
#8842=CIRCLE('',#24126,0.405);
#8843=CIRCLE('',#24128,0.405);
#8844=CIRCLE('',#24130,0.404999999999999);
#8845=CIRCLE('',#24132,0.404999999999999);
#8846=CIRCLE('',#24134,0.405);
#8847=CIRCLE('',#24136,0.405);
#8848=CIRCLE('',#24138,0.404999999999999);
#8849=CIRCLE('',#24140,0.404999999999999);
#8850=CIRCLE('',#24148,2.6);
#8851=CIRCLE('',#24149,2.6);
#8852=CIRCLE('',#24151,2.6);
#8853=CIRCLE('',#24155,2.4);
#8854=CIRCLE('',#24157,2.4);
#8855=CIRCLE('',#24161,0.6);
#8856=CIRCLE('',#24162,0.575);
#8857=CIRCLE('',#24164,0.575);
#8858=CIRCLE('',#24166,0.6);
#8859=CIRCLE('',#24168,0.6);
#8860=CIRCLE('',#24170,0.575);
#8861=CIRCLE('',#24172,0.575);
#8862=CIRCLE('',#24174,0.6);
#8863=CIRCLE('',#24176,0.6);
#8864=CIRCLE('',#24178,0.3);
#8865=CIRCLE('',#24179,0.3);
#8866=CIRCLE('',#24181,0.54);
#8867=CIRCLE('',#24184,0.6);
#8868=CIRCLE('',#24186,0.54);
#8869=CIRCLE('',#24188,0.25);
#8870=CIRCLE('',#24190,0.25);
#8871=CIRCLE('',#24192,0.075);
#8872=CIRCLE('',#24194,0.075);
#8873=CIRCLE('',#24196,0.45);
#8874=CIRCLE('',#24199,0.59);
#8875=CIRCLE('',#24200,0.59);
#8876=CIRCLE('',#24202,0.65);
#8877=CIRCLE('',#24203,0.65);
#8878=CIRCLE('',#24206,0.76);
#8879=CIRCLE('',#24208,0.405344298097309);
#8880=CIRCLE('',#24209,0.452);
#8881=CIRCLE('',#24210,0.075);
#8882=CIRCLE('',#24212,0.075);
#8883=CIRCLE('',#24214,0.4);
#8884=CIRCLE('',#24216,0.4);
#8885=CIRCLE('',#24219,0.8);
#8886=CIRCLE('',#24221,0.8);
#8887=CIRCLE('',#24223,0.76);
#8888=CIRCLE('',#24225,0.55);
#8889=CIRCLE('',#24227,0.55);
#8890=CIRCLE('',#24229,0.51);
#8891=CIRCLE('',#24233,1.75488973075546);
#8892=CIRCLE('',#24234,2.02309581191037);
#8893=CIRCLE('',#24270,1.83314153881416);
#8894=CIRCLE('',#24271,2.10134761996907);
#8895=CIRCLE('',#24309,0.3);
#8896=CIRCLE('',#24311,0.3);
#8897=CIRCLE('',#24313,0.3);
#8898=CIRCLE('',#24315,0.34);
#8899=CIRCLE('',#24317,0.34);
#8900=CIRCLE('',#24321,0.3);
#8901=CIRCLE('',#24323,0.3);
#8902=CIRCLE('',#24325,0.3);
#8903=CIRCLE('',#24327,0.34);
#8904=CIRCLE('',#24329,0.34);
#8905=CIRCLE('',#24333,0.3);
#8906=CIRCLE('',#24335,0.3);
#8907=CIRCLE('',#24337,0.3);
#8908=CIRCLE('',#24339,0.34);
#8909=CIRCLE('',#24341,0.34);
#8910=CIRCLE('',#24345,0.3);
#8911=CIRCLE('',#24347,0.3);
#8912=CIRCLE('',#24349,0.3);
#8913=CIRCLE('',#24351,0.34);
#8914=CIRCLE('',#24353,0.34);
#8915=CIRCLE('',#24357,0.3);
#8916=CIRCLE('',#24359,0.3);
#8917=CIRCLE('',#24361,0.3);
#8918=CIRCLE('',#24363,0.34);
#8919=CIRCLE('',#24365,0.34);
#8920=CIRCLE('',#24369,0.3);
#8921=CIRCLE('',#24371,0.3);
#8922=CIRCLE('',#24373,0.3);
#8923=CIRCLE('',#24375,0.34);
#8924=CIRCLE('',#24377,0.34);
#8925=CIRCLE('',#24381,0.3);
#8926=CIRCLE('',#24383,0.3);
#8927=CIRCLE('',#24385,0.3);
#8928=CIRCLE('',#24387,0.34);
#8929=CIRCLE('',#24389,0.34);
#8930=CIRCLE('',#24393,0.3);
#8931=CIRCLE('',#24395,0.3);
#8932=CIRCLE('',#24397,0.3);
#8933=CIRCLE('',#24399,0.34);
#8934=CIRCLE('',#24401,0.34);
#8935=CIRCLE('',#24405,0.3);
#8936=CIRCLE('',#24407,0.3);
#8937=CIRCLE('',#24409,0.3);
#8938=CIRCLE('',#24411,0.34);
#8939=CIRCLE('',#24413,0.34);
#8940=CIRCLE('',#24417,0.3);
#8941=CIRCLE('',#24419,0.3);
#8942=CIRCLE('',#24421,0.3);
#8943=CIRCLE('',#24423,0.34);
#8944=CIRCLE('',#24425,0.34);
#8945=CIRCLE('',#24429,0.3);
#8946=CIRCLE('',#24431,0.3);
#8947=CIRCLE('',#24433,0.3);
#8948=CIRCLE('',#24435,0.34);
#8949=CIRCLE('',#24437,0.34);
#8950=CIRCLE('',#24441,0.3);
#8951=CIRCLE('',#24443,0.3);
#8952=CIRCLE('',#24445,0.3);
#8953=CIRCLE('',#24447,0.34);
#8954=CIRCLE('',#24449,0.34);
#8955=CIRCLE('',#24453,0.3);
#8956=CIRCLE('',#24455,0.3);
#8957=CIRCLE('',#24457,0.3);
#8958=CIRCLE('',#24459,0.34);
#8959=CIRCLE('',#24461,0.34);
#8960=CIRCLE('',#24465,0.3);
#8961=CIRCLE('',#24467,0.3);
#8962=CIRCLE('',#24469,0.3);
#8963=CIRCLE('',#24471,0.34);
#8964=CIRCLE('',#24473,0.34);
#8965=CIRCLE('',#24477,0.3);
#8966=CIRCLE('',#24479,0.3);
#8967=CIRCLE('',#24481,0.3);
#8968=CIRCLE('',#24483,0.34);
#8969=CIRCLE('',#24485,0.34);
#8970=CIRCLE('',#24489,0.3);
#8971=CIRCLE('',#24491,0.3);
#8972=CIRCLE('',#24493,0.3);
#8973=CIRCLE('',#24495,0.34);
#8974=CIRCLE('',#24497,0.34);
#8975=CIRCLE('',#24501,0.34);
#8976=CIRCLE('',#24503,0.3);
#8977=CIRCLE('',#24505,0.3);
#8978=CIRCLE('',#24507,0.3);
#8979=CIRCLE('',#24510,0.34);
#8980=CIRCLE('',#24513,0.34);
#8981=CIRCLE('',#24517,1.5105713967741);
#8982=CIRCLE('',#24518,1.71158415478175);
#8983=CIRCLE('',#24519,1.71158415478175);
#8984=CIRCLE('',#24520,1.71158415478175);
#8985=CIRCLE('',#24521,1.71158415478175);
#8986=CIRCLE('',#24522,1.71158415478175);
#8987=CIRCLE('',#24523,1.71158415478175);
#8988=CIRCLE('',#24524,1.71158415478175);
#8989=CIRCLE('',#24525,1.71158415478175);
#8990=CIRCLE('',#24526,1.71158415478175);
#8991=CIRCLE('',#24527,1.71158415478175);
#8992=CIRCLE('',#24528,1.71158415478175);
#8993=CIRCLE('',#24529,1.71158415478175);
#8994=CIRCLE('',#24530,1.71158415478175);
#8995=CIRCLE('',#24531,1.71158415478175);
#8996=CIRCLE('',#24532,1.71158415478175);
#8997=CIRCLE('',#24533,1.71158415478175);
#8998=CIRCLE('',#24534,1.71158415478175);
#8999=CIRCLE('',#24535,1.71158415478175);
#9000=CIRCLE('',#24537,0.34);
#9001=CIRCLE('',#24541,0.34);
#9002=CIRCLE('',#24545,0.34);
#9003=CIRCLE('',#24549,0.34);
#9004=CIRCLE('',#24553,0.34);
#9005=CIRCLE('',#24557,0.34);
#9006=CIRCLE('',#24561,0.34);
#9007=CIRCLE('',#24565,0.34);
#9008=CIRCLE('',#24569,0.34);
#9009=CIRCLE('',#24573,0.34);
#9010=CIRCLE('',#24577,0.34);
#9011=CIRCLE('',#24581,0.34);
#9012=CIRCLE('',#24585,0.34);
#9013=CIRCLE('',#24589,0.34);
#9014=CIRCLE('',#24593,0.34);
#9015=CIRCLE('',#24598,0.34);
#9016=CIRCLE('',#24601,1.25);
#9017=CIRCLE('',#24602,1.31);
#9018=CIRCLE('',#24604,1.84);
#9019=CIRCLE('',#24606,1.9);
#9020=CIRCLE('',#24608,1.9);
#9021=CIRCLE('',#24611,1.6);
#9022=CIRCLE('',#24613,1.6);
#9023=CIRCLE('',#24615,1.31);
#9024=CIRCLE('',#24617,1.25);
#9025=CIRCLE('',#24621,2.37133297968149);
#9026=CIRCLE('',#24622,2.43379937982364);
#9027=CIRCLE('',#24624,2.54);
#9028=CIRCLE('',#24626,2.6);
#9029=CIRCLE('',#24628,2.6);
#9030=CIRCLE('',#24630,2.54);
#9031=CIRCLE('',#24632,2.10967297612751);
#9032=CIRCLE('',#24634,2.07213937626967);
#9033=CIRCLE('',#24638,0.1);
#9034=CIRCLE('',#24639,0.1);
#9035=CIRCLE('',#24641,0.1);
#9036=CIRCLE('',#24642,0.1);
#9037=CIRCLE('',#24645,0.328820889047374);
#9038=CIRCLE('',#24646,0.328820889047374);
#9039=CIRCLE('',#24649,1.195);
#9040=CIRCLE('',#24650,1.195);
#9041=CIRCLE('',#24653,0.328820889047374);
#9042=CIRCLE('',#24654,0.328820889047374);
#9043=CIRCLE('',#24657,1.53);
#9044=CIRCLE('',#24658,1.53);
#9045=CIRCLE('',#24663,0.3933);
#9046=CIRCLE('',#24664,0.3933);
#9047=CIRCLE('',#24665,0.3933);
#9048=CIRCLE('',#24688,0.3933);
#9049=CIRCLE('',#24690,0.322275);
#9050=CIRCLE('',#24713,0.3933);
#9051=CIRCLE('',#24715,0.322275);
#9052=CIRCLE('',#24718,0.3933);
#9053=CIRCLE('',#24720,0.04);
#9054=CIRCLE('',#24721,0.4333);
#9055=CIRCLE('',#24723,0.61);
#9056=CIRCLE('',#24725,0.29999119987093);
#9057=CIRCLE('',#24735,0.65);
#9058=CIRCLE('',#24738,0.65);
#9059=CIRCLE('',#24741,0.65);
#9060=CIRCLE('',#24744,0.65);
#9061=CIRCLE('',#24747,0.65);
#9062=CIRCLE('',#24750,0.65);
#9063=CIRCLE('',#24753,0.65);
#9064=CIRCLE('',#24756,0.65);
#9065=CIRCLE('',#24759,0.65);
#9066=CIRCLE('',#24762,0.65);
#9067=CIRCLE('',#24765,0.65);
#9068=CIRCLE('',#24768,0.65);
#9069=CIRCLE('',#24771,0.65);
#9070=CIRCLE('',#24774,0.65);
#9071=CIRCLE('',#24777,0.65);
#9072=CIRCLE('',#24780,0.65);
#9073=CIRCLE('',#24783,0.65);
#9074=CIRCLE('',#24784,0.65);
#9075=CIRCLE('',#24787,0.65);
#9076=CIRCLE('',#24788,0.65);
#9077=CIRCLE('',#24791,0.65);
#9078=CIRCLE('',#24794,0.65);
#9079=CIRCLE('',#24797,0.65);
#9080=CIRCLE('',#24800,0.65);
#9081=CIRCLE('',#24803,0.65);
#9082=CIRCLE('',#24806,0.65);
#9083=CIRCLE('',#24809,0.65);
#9084=CIRCLE('',#24812,0.65);
#9085=CIRCLE('',#24815,0.65);
#9086=CIRCLE('',#24818,0.65);
#9087=CIRCLE('',#24821,0.65);
#9088=CIRCLE('',#24824,0.65);
#9089=CIRCLE('',#24827,0.65);
#9090=CIRCLE('',#24830,0.65);
#9091=CIRCLE('',#24833,0.65);
#9092=CIRCLE('',#24836,0.65);
#9093=CIRCLE('',#24839,0.65);
#9094=CIRCLE('',#24842,0.65);
#9095=CIRCLE('',#24845,0.65);
#9096=CIRCLE('',#24848,0.65);
#9097=CIRCLE('',#24851,0.65);
#9098=CIRCLE('',#24854,0.65);
#9099=CIRCLE('',#24857,0.65);
#9100=CIRCLE('',#24860,0.65);
#9101=CIRCLE('',#24863,0.65);
#9102=CIRCLE('',#24866,0.65);
#9103=CIRCLE('',#24869,0.65);
#9104=CIRCLE('',#24872,0.65);
#9105=CIRCLE('',#24875,0.65);
#9106=CIRCLE('',#24878,0.65);
#9107=CIRCLE('',#24881,0.65);
#9108=CIRCLE('',#24884,0.65);
#9109=CIRCLE('',#24887,0.65);
#9110=CIRCLE('',#24890,0.65);
#9111=CIRCLE('',#24892,0.65);
#9112=CIRCLE('',#24896,0.65);
#9113=CIRCLE('',#24899,0.65);
#9114=CIRCLE('',#24902,0.65);
#9115=CIRCLE('',#24905,0.65);
#9116=CIRCLE('',#24908,0.65);
#9117=CIRCLE('',#24911,0.65);
#9118=CIRCLE('',#24914,0.65);
#9119=CIRCLE('',#24917,0.65);
#9120=CIRCLE('',#24920,0.65);
#9121=CIRCLE('',#24923,0.65);
#9122=CIRCLE('',#24926,0.65);
#9123=CIRCLE('',#24929,0.65);
#9124=CIRCLE('',#24932,0.65);
#9125=CIRCLE('',#24935,0.65);
#9126=CIRCLE('',#24938,0.65);
#9127=CIRCLE('',#24941,0.65);
#9128=CIRCLE('',#24944,0.65);
#9129=CIRCLE('',#24947,0.65);
#9130=CIRCLE('',#24950,0.65);
#9131=CIRCLE('',#24952,0.34);
#9132=CIRCLE('',#24955,0.65);
#9133=CIRCLE('',#24957,0.65);
#9134=CIRCLE('',#24958,0.65);
#9135=CIRCLE('',#24959,0.65);
#9136=CIRCLE('',#24960,0.65);
#9137=CIRCLE('',#24961,0.65);
#9138=CIRCLE('',#24962,0.65);
#9139=CIRCLE('',#24963,0.65);
#9140=CIRCLE('',#24964,0.65);
#9141=CIRCLE('',#24965,0.65);
#9142=CIRCLE('',#24966,0.65);
#9143=CIRCLE('',#24967,0.65);
#9144=CIRCLE('',#24968,0.65);
#9145=CIRCLE('',#24969,0.65);
#9146=CIRCLE('',#24970,0.65);
#9147=CIRCLE('',#24971,0.65);
#9148=CIRCLE('',#24972,0.65);
#9149=CIRCLE('',#24973,0.65);
#9150=CIRCLE('',#24974,0.65);
#9151=CIRCLE('',#24975,0.65);
#9152=CIRCLE('',#24976,0.65);
#9153=CIRCLE('',#24977,0.65);
#9154=CIRCLE('',#24978,0.65);
#9155=CIRCLE('',#24979,0.65);
#9156=CIRCLE('',#24980,0.65);
#9157=CIRCLE('',#24981,0.65);
#9158=CIRCLE('',#24982,0.65);
#9159=CIRCLE('',#24983,0.65);
#9160=CIRCLE('',#24984,0.65);
#9161=CIRCLE('',#24985,0.65);
#9162=CIRCLE('',#24986,0.65);
#9163=CIRCLE('',#24987,0.65);
#9164=CIRCLE('',#24988,0.65);
#9165=CIRCLE('',#24989,0.65);
#9166=CIRCLE('',#24990,0.65);
#9167=CIRCLE('',#24991,0.65);
#9168=CIRCLE('',#24992,0.65);
#9169=CIRCLE('',#24994,0.59);
#9170=CIRCLE('',#24998,0.7475);
#9171=CIRCLE('',#25006,0.7475);
#9172=CIRCLE('',#25008,0.7925);
#9173=CIRCLE('',#25018,0.70685);
#9174=CIRCLE('',#25028,0.7925);
#9175=CIRCLE('',#25029,0.7925);
#9176=CIRCLE('',#25031,0.70685);
#9177=CIRCLE('',#25033,0.7925);
#9178=CIRCLE('',#25035,0.82685);
#9179=CIRCLE('',#25036,0.82685);
#9180=CIRCLE('',#25037,0.7475);
#9181=CIRCLE('',#25040,1.045);
#9182=CIRCLE('',#25045,1.045);
#9183=CIRCLE('',#25049,0.4);
#9184=CIRCLE('',#25051,0.7431);
#9185=CIRCLE('',#25053,0.4);
#9186=CIRCLE('',#25057,0.4);
#9187=CIRCLE('',#25059,0.4);
#9188=CIRCLE('',#25061,0.7531);
#9189=CIRCLE('',#25064,0.7431);
#9190=CIRCLE('',#25067,0.74);
#9191=CIRCLE('',#25069,0.58);
#9192=VERTEX_POINT('',#30694);
#9193=VERTEX_POINT('',#30696);
#9194=VERTEX_POINT('',#30700);
#9195=VERTEX_POINT('',#30704);
#9196=VERTEX_POINT('',#30706);
#9197=VERTEX_POINT('',#30708);
#9198=VERTEX_POINT('',#30710);
#9199=VERTEX_POINT('',#30712);
#9200=VERTEX_POINT('',#30714);
#9201=VERTEX_POINT('',#30716);
#9202=VERTEX_POINT('',#30718);
#9203=VERTEX_POINT('',#30720);
#9204=VERTEX_POINT('',#30722);
#9205=VERTEX_POINT('',#30725);
#9206=VERTEX_POINT('',#30729);
#9207=VERTEX_POINT('',#30731);
#9208=VERTEX_POINT('',#30733);
#9209=VERTEX_POINT('',#30735);
#9210=VERTEX_POINT('',#30737);
#9211=VERTEX_POINT('',#30739);
#9212=VERTEX_POINT('',#30741);
#9213=VERTEX_POINT('',#30743);
#9214=VERTEX_POINT('',#30745);
#9215=VERTEX_POINT('',#30747);
#9216=VERTEX_POINT('',#30750);
#9217=VERTEX_POINT('',#30754);
#9218=VERTEX_POINT('',#30760);
#9219=VERTEX_POINT('',#30764);
#9220=VERTEX_POINT('',#30770);
#9221=VERTEX_POINT('',#30774);
#9222=VERTEX_POINT('',#30780);
#9223=VERTEX_POINT('',#30784);
#9224=VERTEX_POINT('',#30790);
#9225=VERTEX_POINT('',#30794);
#9226=VERTEX_POINT('',#30800);
#9227=VERTEX_POINT('',#30804);
#9228=VERTEX_POINT('',#30810);
#9229=VERTEX_POINT('',#30814);
#9230=VERTEX_POINT('',#30820);
#9231=VERTEX_POINT('',#30824);
#9232=VERTEX_POINT('',#30832);
#9233=VERTEX_POINT('',#30836);
#9234=VERTEX_POINT('',#30843);
#9235=VERTEX_POINT('',#30845);
#9236=VERTEX_POINT('',#30849);
#9237=VERTEX_POINT('',#30852);
#9238=VERTEX_POINT('',#30856);
#9239=VERTEX_POINT('',#30860);
#9240=VERTEX_POINT('',#30863);
#9241=VERTEX_POINT('',#30867);
#9242=VERTEX_POINT('',#30871);
#9243=VERTEX_POINT('',#30875);
#9244=VERTEX_POINT('',#30881);
#9245=VERTEX_POINT('',#30882);
#9246=VERTEX_POINT('',#30886);
#9247=VERTEX_POINT('',#30888);
#9248=VERTEX_POINT('',#30890);
#9249=VERTEX_POINT('',#30892);
#9250=VERTEX_POINT('',#30899);
#9251=VERTEX_POINT('',#30901);
#9252=VERTEX_POINT('',#30903);
#9253=VERTEX_POINT('',#30907);
#9254=VERTEX_POINT('',#30908);
#9255=VERTEX_POINT('',#30912);
#9256=VERTEX_POINT('',#30914);
#9257=VERTEX_POINT('',#30916);
#9258=VERTEX_POINT('',#30918);
#9259=VERTEX_POINT('',#30920);
#9260=VERTEX_POINT('',#30927);
#9261=VERTEX_POINT('',#30929);
#9262=VERTEX_POINT('',#30937);
#9263=VERTEX_POINT('',#30981);
#9264=VERTEX_POINT('',#30992);
#9265=VERTEX_POINT('',#31005);
#9266=VERTEX_POINT('',#31007);
#9267=VERTEX_POINT('',#31011);
#9268=VERTEX_POINT('',#31091);
#9269=VERTEX_POINT('',#31187);
#9270=VERTEX_POINT('',#31188);
#9271=VERTEX_POINT('',#31227);
#9272=VERTEX_POINT('',#31231);
#9273=VERTEX_POINT('',#31232);
#9274=VERTEX_POINT('',#31249);
#9275=VERTEX_POINT('',#32187);
#9276=VERTEX_POINT('',#32188);
#9277=VERTEX_POINT('',#32190);
#9278=VERTEX_POINT('',#32192);
#9279=VERTEX_POINT('',#32196);
#9280=VERTEX_POINT('',#32197);
#9281=VERTEX_POINT('',#32202);
#9282=VERTEX_POINT('',#32203);
#9283=VERTEX_POINT('',#32211);
#9284=VERTEX_POINT('',#32213);
#9285=VERTEX_POINT('',#32217);
#9286=VERTEX_POINT('',#32222);
#9287=VERTEX_POINT('',#32230);
#9288=VERTEX_POINT('',#32232);
#9289=VERTEX_POINT('',#32236);
#9290=VERTEX_POINT('',#32238);
#9291=VERTEX_POINT('',#32243);
#9292=VERTEX_POINT('',#32246);
#9293=VERTEX_POINT('',#32248);
#9294=VERTEX_POINT('',#32250);
#9295=VERTEX_POINT('',#32254);
#9296=VERTEX_POINT('',#32256);
#9297=VERTEX_POINT('',#32261);
#9298=VERTEX_POINT('',#32265);
#9299=VERTEX_POINT('',#32268);
#9300=VERTEX_POINT('',#32272);
#9301=VERTEX_POINT('',#32276);
#9302=VERTEX_POINT('',#32280);
#9303=VERTEX_POINT('',#32284);
#9304=VERTEX_POINT('',#32288);
#9305=VERTEX_POINT('',#32292);
#9306=VERTEX_POINT('',#32298);
#9307=VERTEX_POINT('',#32299);
#9308=VERTEX_POINT('',#32301);
#9309=VERTEX_POINT('',#32313);
#9310=VERTEX_POINT('',#32326);
#9311=VERTEX_POINT('',#32327);
#9312=VERTEX_POINT('',#32364);
#9313=VERTEX_POINT('',#32365);
#9314=VERTEX_POINT('',#32402);
#9315=VERTEX_POINT('',#32403);
#9316=VERTEX_POINT('',#32439);
#9317=VERTEX_POINT('',#32440);
#9318=VERTEX_POINT('',#32476);
#9319=VERTEX_POINT('',#32477);
#9320=VERTEX_POINT('',#32514);
#9321=VERTEX_POINT('',#32515);
#9322=VERTEX_POINT('',#32552);
#9323=VERTEX_POINT('',#32553);
#9324=VERTEX_POINT('',#32555);
#9325=VERTEX_POINT('',#33095);
#9326=VERTEX_POINT('',#33096);
#9327=VERTEX_POINT('',#33105);
#9328=VERTEX_POINT('',#33398);
#9329=VERTEX_POINT('',#33911);
#9330=VERTEX_POINT('',#33964);
#9331=VERTEX_POINT('',#34626);
#9332=VERTEX_POINT('',#34640);
#9333=VERTEX_POINT('',#34643);
#9334=VERTEX_POINT('',#34652);
#9335=VERTEX_POINT('',#35215);
#9336=VERTEX_POINT('',#35726);
#9337=VERTEX_POINT('',#36392);
#9338=VERTEX_POINT('',#36393);
#9339=VERTEX_POINT('',#36395);
#9340=VERTEX_POINT('',#36397);
#9341=VERTEX_POINT('',#36401);
#9342=VERTEX_POINT('',#36403);
#9343=VERTEX_POINT('',#36407);
#9344=VERTEX_POINT('',#36409);
#9345=VERTEX_POINT('',#36413);
#9346=VERTEX_POINT('',#36415);
#9347=VERTEX_POINT('',#36419);
#9348=VERTEX_POINT('',#36421);
#9349=VERTEX_POINT('',#36429);
#9350=VERTEX_POINT('',#36430);
#9351=VERTEX_POINT('',#36432);
#9352=VERTEX_POINT('',#36434);
#9353=VERTEX_POINT('',#36438);
#9354=VERTEX_POINT('',#36442);
#9355=VERTEX_POINT('',#36448);
#9356=VERTEX_POINT('',#36449);
#9357=VERTEX_POINT('',#36451);
#9358=VERTEX_POINT('',#36453);
#9359=VERTEX_POINT('',#36457);
#9360=VERTEX_POINT('',#36461);
#9361=VERTEX_POINT('',#36467);
#9362=VERTEX_POINT('',#36468);
#9363=VERTEX_POINT('',#36470);
#9364=VERTEX_POINT('',#36472);
#9365=VERTEX_POINT('',#36476);
#9366=VERTEX_POINT('',#36480);
#9367=VERTEX_POINT('',#36486);
#9368=VERTEX_POINT('',#36487);
#9369=VERTEX_POINT('',#36489);
#9370=VERTEX_POINT('',#36491);
#9371=VERTEX_POINT('',#36495);
#9372=VERTEX_POINT('',#36499);
#9373=VERTEX_POINT('',#36505);
#9374=VERTEX_POINT('',#36506);
#9375=VERTEX_POINT('',#36508);
#9376=VERTEX_POINT('',#36510);
#9377=VERTEX_POINT('',#36514);
#9378=VERTEX_POINT('',#36518);
#9379=VERTEX_POINT('',#36524);
#9380=VERTEX_POINT('',#36525);
#9381=VERTEX_POINT('',#36527);
#9382=VERTEX_POINT('',#36529);
#9383=VERTEX_POINT('',#36533);
#9384=VERTEX_POINT('',#36537);
#9385=VERTEX_POINT('',#36543);
#9386=VERTEX_POINT('',#36544);
#9387=VERTEX_POINT('',#36546);
#9388=VERTEX_POINT('',#36548);
#9389=VERTEX_POINT('',#36552);
#9390=VERTEX_POINT('',#36556);
#9391=VERTEX_POINT('',#36562);
#9392=VERTEX_POINT('',#36563);
#9393=VERTEX_POINT('',#36565);
#9394=VERTEX_POINT('',#36569);
#9395=VERTEX_POINT('',#36571);
#9396=VERTEX_POINT('',#36575);
#9397=VERTEX_POINT('',#36581);
#9398=VERTEX_POINT('',#36582);
#9399=VERTEX_POINT('',#36584);
#9400=VERTEX_POINT('',#36586);
#9401=VERTEX_POINT('',#36590);
#9402=VERTEX_POINT('',#36594);
#9403=VERTEX_POINT('',#36600);
#9404=VERTEX_POINT('',#36601);
#9405=VERTEX_POINT('',#36603);
#9406=VERTEX_POINT('',#36605);
#9407=VERTEX_POINT('',#36609);
#9408=VERTEX_POINT('',#36613);
#9409=VERTEX_POINT('',#36619);
#9410=VERTEX_POINT('',#36620);
#9411=VERTEX_POINT('',#36622);
#9412=VERTEX_POINT('',#36624);
#9413=VERTEX_POINT('',#36628);
#9414=VERTEX_POINT('',#36632);
#9415=VERTEX_POINT('',#36638);
#9416=VERTEX_POINT('',#36639);
#9417=VERTEX_POINT('',#36641);
#9418=VERTEX_POINT('',#36643);
#9419=VERTEX_POINT('',#36647);
#9420=VERTEX_POINT('',#36651);
#9421=VERTEX_POINT('',#36657);
#9422=VERTEX_POINT('',#36658);
#9423=VERTEX_POINT('',#36660);
#9424=VERTEX_POINT('',#36662);
#9425=VERTEX_POINT('',#36666);
#9426=VERTEX_POINT('',#36670);
#9427=VERTEX_POINT('',#36676);
#9428=VERTEX_POINT('',#36677);
#9429=VERTEX_POINT('',#36679);
#9430=VERTEX_POINT('',#36681);
#9431=VERTEX_POINT('',#36685);
#9432=VERTEX_POINT('',#36689);
#9433=VERTEX_POINT('',#36695);
#9434=VERTEX_POINT('',#36696);
#9435=VERTEX_POINT('',#36698);
#9436=VERTEX_POINT('',#36700);
#9437=VERTEX_POINT('',#36704);
#9438=VERTEX_POINT('',#36708);
#9439=VERTEX_POINT('',#36714);
#9440=VERTEX_POINT('',#36715);
#9441=VERTEX_POINT('',#36717);
#9442=VERTEX_POINT('',#36719);
#9443=VERTEX_POINT('',#36723);
#9444=VERTEX_POINT('',#36727);
#9445=VERTEX_POINT('',#36733);
#9446=VERTEX_POINT('',#36734);
#9447=VERTEX_POINT('',#36736);
#9448=VERTEX_POINT('',#36738);
#9449=VERTEX_POINT('',#36742);
#9450=VERTEX_POINT('',#36746);
#9451=VERTEX_POINT('',#36752);
#9452=VERTEX_POINT('',#36753);
#9453=VERTEX_POINT('',#36755);
#9454=VERTEX_POINT('',#36757);
#9455=VERTEX_POINT('',#36761);
#9456=VERTEX_POINT('',#36765);
#9457=VERTEX_POINT('',#36771);
#9458=VERTEX_POINT('',#36772);
#9459=VERTEX_POINT('',#36774);
#9460=VERTEX_POINT('',#36776);
#9461=VERTEX_POINT('',#36780);
#9462=VERTEX_POINT('',#36784);
#9463=VERTEX_POINT('',#36790);
#9464=VERTEX_POINT('',#36791);
#9465=VERTEX_POINT('',#36793);
#9466=VERTEX_POINT('',#36795);
#9467=VERTEX_POINT('',#36799);
#9468=VERTEX_POINT('',#36803);
#9469=VERTEX_POINT('',#36809);
#9470=VERTEX_POINT('',#36810);
#9471=VERTEX_POINT('',#36812);
#9472=VERTEX_POINT('',#36814);
#9473=VERTEX_POINT('',#36818);
#9474=VERTEX_POINT('',#36822);
#9475=VERTEX_POINT('',#36828);
#9476=VERTEX_POINT('',#36829);
#9477=VERTEX_POINT('',#36831);
#9478=VERTEX_POINT('',#36833);
#9479=VERTEX_POINT('',#36837);
#9480=VERTEX_POINT('',#36841);
#9481=VERTEX_POINT('',#36847);
#9482=VERTEX_POINT('',#36848);
#9483=VERTEX_POINT('',#36850);
#9484=VERTEX_POINT('',#36852);
#9485=VERTEX_POINT('',#36856);
#9486=VERTEX_POINT('',#36858);
#9487=VERTEX_POINT('',#36862);
#9488=VERTEX_POINT('',#36866);
#9489=VERTEX_POINT('',#36870);
#9490=VERTEX_POINT('',#36871);
#9491=VERTEX_POINT('',#36873);
#9492=VERTEX_POINT('',#36875);
#9493=VERTEX_POINT('',#36879);
#9494=VERTEX_POINT('',#36883);
#9495=VERTEX_POINT('',#36889);
#9496=VERTEX_POINT('',#36890);
#9497=VERTEX_POINT('',#36892);
#9498=VERTEX_POINT('',#36894);
#9499=VERTEX_POINT('',#36898);
#9500=VERTEX_POINT('',#36902);
#9501=VERTEX_POINT('',#36908);
#9502=VERTEX_POINT('',#36909);
#9503=VERTEX_POINT('',#36911);
#9504=VERTEX_POINT('',#36913);
#9505=VERTEX_POINT('',#36917);
#9506=VERTEX_POINT('',#36921);
#9507=VERTEX_POINT('',#36927);
#9508=VERTEX_POINT('',#36928);
#9509=VERTEX_POINT('',#36930);
#9510=VERTEX_POINT('',#36932);
#9511=VERTEX_POINT('',#36936);
#9512=VERTEX_POINT('',#36940);
#9513=VERTEX_POINT('',#36946);
#9514=VERTEX_POINT('',#36947);
#9515=VERTEX_POINT('',#36949);
#9516=VERTEX_POINT('',#36951);
#9517=VERTEX_POINT('',#36955);
#9518=VERTEX_POINT('',#36959);
#9519=VERTEX_POINT('',#36965);
#9520=VERTEX_POINT('',#36966);
#9521=VERTEX_POINT('',#36968);
#9522=VERTEX_POINT('',#36970);
#9523=VERTEX_POINT('',#36974);
#9524=VERTEX_POINT('',#36978);
#9525=VERTEX_POINT('',#36984);
#9526=VERTEX_POINT('',#36985);
#9527=VERTEX_POINT('',#36987);
#9528=VERTEX_POINT('',#36989);
#9529=VERTEX_POINT('',#36993);
#9530=VERTEX_POINT('',#36997);
#9531=VERTEX_POINT('',#37003);
#9532=VERTEX_POINT('',#37005);
#9533=VERTEX_POINT('',#37007);
#9534=VERTEX_POINT('',#37011);
#9535=VERTEX_POINT('',#37015);
#9536=VERTEX_POINT('',#37019);
#9537=VERTEX_POINT('',#37023);
#9538=VERTEX_POINT('',#37027);
#9539=VERTEX_POINT('',#37035);
#9540=VERTEX_POINT('',#37037);
#9541=VERTEX_POINT('',#37043);
#9542=VERTEX_POINT('',#37049);
#9543=VERTEX_POINT('',#37055);
#9544=VERTEX_POINT('',#37059);
#9545=VERTEX_POINT('',#37063);
#9546=VERTEX_POINT('',#37066);
#9547=VERTEX_POINT('',#37076);
#9548=VERTEX_POINT('',#37079);
#9549=VERTEX_POINT('',#37085);
#9550=VERTEX_POINT('',#37087);
#9551=VERTEX_POINT('',#37091);
#9552=VERTEX_POINT('',#37094);
#9553=VERTEX_POINT('',#37099);
#9554=VERTEX_POINT('',#37136);
#9555=VERTEX_POINT('',#37142);
#9556=VERTEX_POINT('',#37143);
#9557=VERTEX_POINT('',#37145);
#9558=VERTEX_POINT('',#37157);
#9559=VERTEX_POINT('',#37170);
#9560=VERTEX_POINT('',#37171);
#9561=VERTEX_POINT('',#37208);
#9562=VERTEX_POINT('',#37209);
#9563=VERTEX_POINT('',#37246);
#9564=VERTEX_POINT('',#37247);
#9565=VERTEX_POINT('',#37284);
#9566=VERTEX_POINT('',#37285);
#9567=VERTEX_POINT('',#37287);
#9568=VERTEX_POINT('',#37323);
#9569=VERTEX_POINT('',#37324);
#9570=VERTEX_POINT('',#37326);
#9571=VERTEX_POINT('',#37343);
#9572=VERTEX_POINT('',#37356);
#9573=VERTEX_POINT('',#37357);
#9574=VERTEX_POINT('',#37440);
#9575=VERTEX_POINT('',#37441);
#9576=VERTEX_POINT('',#37530);
#9577=VERTEX_POINT('',#37531);
#9578=VERTEX_POINT('',#37614);
#9579=VERTEX_POINT('',#37615);
#9580=VERTEX_POINT('',#37704);
#9581=VERTEX_POINT('',#37705);
#9582=VERTEX_POINT('',#37794);
#9583=VERTEX_POINT('',#37795);
#9584=VERTEX_POINT('',#37878);
#9585=VERTEX_POINT('',#37879);
#9586=VERTEX_POINT('',#37881);
#9587=VERTEX_POINT('',#37890);
#9588=VERTEX_POINT('',#37898);
#9589=VERTEX_POINT('',#37899);
#9590=VERTEX_POINT('',#37935);
#9591=VERTEX_POINT('',#37936);
#9592=VERTEX_POINT('',#37972);
#9593=VERTEX_POINT('',#37973);
#9594=VERTEX_POINT('',#38010);
#9595=VERTEX_POINT('',#38011);
#9596=VERTEX_POINT('',#38047);
#9597=VERTEX_POINT('',#38048);
#9598=VERTEX_POINT('',#38084);
#9599=VERTEX_POINT('',#38085);
#9600=VERTEX_POINT('',#38121);
#9601=VERTEX_POINT('',#38195);
#9602=VERTEX_POINT('',#38197);
#9603=VERTEX_POINT('',#38686);
#9604=VERTEX_POINT('',#38775);
#9605=VERTEX_POINT('',#39587);
#9606=VERTEX_POINT('',#39588);
#9607=VERTEX_POINT('',#39597);
#9608=VERTEX_POINT('',#39776);
#9609=VERTEX_POINT('',#40099);
#9610=VERTEX_POINT('',#40146);
#9611=VERTEX_POINT('',#40580);
#9612=VERTEX_POINT('',#40594);
#9613=VERTEX_POINT('',#40597);
#9614=VERTEX_POINT('',#40606);
#9615=VERTEX_POINT('',#40979);
#9616=VERTEX_POINT('',#41300);
#9617=VERTEX_POINT('',#41735);
#9618=VERTEX_POINT('',#41737);
#9619=VERTEX_POINT('',#41739);
#9620=VERTEX_POINT('',#41743);
#9621=VERTEX_POINT('',#41747);
#9622=VERTEX_POINT('',#41751);
#9623=VERTEX_POINT('',#41755);
#9624=VERTEX_POINT('',#41759);
#9625=VERTEX_POINT('',#41767);
#9626=VERTEX_POINT('',#41769);
#9627=VERTEX_POINT('',#41775);
#9628=VERTEX_POINT('',#41781);
#9629=VERTEX_POINT('',#41787);
#9630=VERTEX_POINT('',#41791);
#9631=VERTEX_POINT('',#41795);
#9632=VERTEX_POINT('',#41798);
#9633=VERTEX_POINT('',#41809);
#9634=VERTEX_POINT('',#41812);
#9635=VERTEX_POINT('',#41815);
#9636=VERTEX_POINT('',#41821);
#9637=VERTEX_POINT('',#41825);
#9638=VERTEX_POINT('',#41829);
#9639=VERTEX_POINT('',#41834);
#9640=VERTEX_POINT('',#41839);
#9641=VERTEX_POINT('',#41843);
#9642=VERTEX_POINT('',#41849);
#9643=VERTEX_POINT('',#41851);
#9644=VERTEX_POINT('',#41855);
#9645=VERTEX_POINT('',#41858);
#9646=VERTEX_POINT('',#41859);
#9647=VERTEX_POINT('',#41861);
#9648=VERTEX_POINT('',#41863);
#9649=VERTEX_POINT('',#41867);
#9650=VERTEX_POINT('',#41886);
#9651=VERTEX_POINT('',#41890);
#9652=VERTEX_POINT('',#41892);
#9653=VERTEX_POINT('',#41917);
#9654=VERTEX_POINT('',#41918);
#9655=VERTEX_POINT('',#41920);
#9656=VERTEX_POINT('',#41922);
#9657=VERTEX_POINT('',#41926);
#9658=VERTEX_POINT('',#41945);
#9659=VERTEX_POINT('',#41949);
#9660=VERTEX_POINT('',#41951);
#9661=VERTEX_POINT('',#41976);
#9662=VERTEX_POINT('',#41979);
#9663=VERTEX_POINT('',#41983);
#9664=VERTEX_POINT('',#41987);
#9665=VERTEX_POINT('',#41990);
#9666=VERTEX_POINT('',#41994);
#9667=VERTEX_POINT('',#41998);
#9668=VERTEX_POINT('',#42001);
#9669=VERTEX_POINT('',#42005);
#9670=VERTEX_POINT('',#42008);
#9671=VERTEX_POINT('',#42012);
#9672=VERTEX_POINT('',#42015);
#9673=VERTEX_POINT('',#42019);
#9674=VERTEX_POINT('',#42022);
#9675=VERTEX_POINT('',#42026);
#9676=VERTEX_POINT('',#42032);
#9677=VERTEX_POINT('',#42034);
#9678=VERTEX_POINT('',#42037);
#9679=VERTEX_POINT('',#42041);
#9680=VERTEX_POINT('',#42044);
#9681=VERTEX_POINT('',#42048);
#9682=VERTEX_POINT('',#42049);
#9683=VERTEX_POINT('',#42051);
#9684=VERTEX_POINT('',#42053);
#9685=VERTEX_POINT('',#42057);
#9686=VERTEX_POINT('',#42059);
#9687=VERTEX_POINT('',#42063);
#9688=VERTEX_POINT('',#42064);
#9689=VERTEX_POINT('',#42069);
#9690=VERTEX_POINT('',#42073);
#9691=VERTEX_POINT('',#42075);
#9692=VERTEX_POINT('',#42079);
#9693=VERTEX_POINT('',#42081);
#9694=VERTEX_POINT('',#42085);
#9695=VERTEX_POINT('',#42087);
#9696=VERTEX_POINT('',#42091);
#9697=VERTEX_POINT('',#42093);
#9698=VERTEX_POINT('',#42097);
#9699=VERTEX_POINT('',#42099);
#9700=VERTEX_POINT('',#42103);
#9701=VERTEX_POINT('',#42105);
#9702=VERTEX_POINT('',#42109);
#9703=VERTEX_POINT('',#42111);
#9704=VERTEX_POINT('',#42115);
#9705=VERTEX_POINT('',#42117);
#9706=VERTEX_POINT('',#42121);
#9707=VERTEX_POINT('',#42123);
#9708=VERTEX_POINT('',#42127);
#9709=VERTEX_POINT('',#42128);
#9710=VERTEX_POINT('',#42135);
#9711=VERTEX_POINT('',#42137);
#9712=VERTEX_POINT('',#42143);
#9713=VERTEX_POINT('',#42144);
#9714=VERTEX_POINT('',#42151);
#9715=VERTEX_POINT('',#42153);
#9716=VERTEX_POINT('',#42159);
#9717=VERTEX_POINT('',#42160);
#9718=VERTEX_POINT('',#42167);
#9719=VERTEX_POINT('',#42169);
#9720=VERTEX_POINT('',#42175);
#9721=VERTEX_POINT('',#42176);
#9722=VERTEX_POINT('',#42183);
#9723=VERTEX_POINT('',#42185);
#9724=VERTEX_POINT('',#42191);
#9725=VERTEX_POINT('',#42192);
#9726=VERTEX_POINT('',#42199);
#9727=VERTEX_POINT('',#42201);
#9728=VERTEX_POINT('',#42207);
#9729=VERTEX_POINT('',#42208);
#9730=VERTEX_POINT('',#42215);
#9731=VERTEX_POINT('',#42217);
#9732=VERTEX_POINT('',#42223);
#9733=VERTEX_POINT('',#42224);
#9734=VERTEX_POINT('',#42231);
#9735=VERTEX_POINT('',#42233);
#9736=VERTEX_POINT('',#42239);
#9737=VERTEX_POINT('',#42240);
#9738=VERTEX_POINT('',#42247);
#9739=VERTEX_POINT('',#42249);
#9740=VERTEX_POINT('',#42255);
#9741=VERTEX_POINT('',#42256);
#9742=VERTEX_POINT('',#42263);
#9743=VERTEX_POINT('',#42265);
#9744=VERTEX_POINT('',#42273);
#9745=VERTEX_POINT('',#42282);
#9746=VERTEX_POINT('',#42285);
#9747=VERTEX_POINT('',#42293);
#9748=VERTEX_POINT('',#42297);
#9749=VERTEX_POINT('',#42305);
#9750=VERTEX_POINT('',#42306);
#9751=VERTEX_POINT('',#42308);
#9752=VERTEX_POINT('',#42310);
#9753=VERTEX_POINT('',#42314);
#9754=VERTEX_POINT('',#42316);
#9755=VERTEX_POINT('',#42320);
#9756=VERTEX_POINT('',#42322);
#9757=VERTEX_POINT('',#42326);
#9758=VERTEX_POINT('',#42328);
#9759=VERTEX_POINT('',#42332);
#9760=VERTEX_POINT('',#42334);
#9761=VERTEX_POINT('',#42338);
#9762=VERTEX_POINT('',#42340);
#9763=VERTEX_POINT('',#42348);
#9764=VERTEX_POINT('',#42350);
#9765=VERTEX_POINT('',#42352);
#9766=VERTEX_POINT('',#42356);
#9767=VERTEX_POINT('',#42359);
#9768=VERTEX_POINT('',#42363);
#9769=VERTEX_POINT('',#42365);
#9770=VERTEX_POINT('',#42367);
#9771=VERTEX_POINT('',#42371);
#9772=VERTEX_POINT('',#42374);
#9773=VERTEX_POINT('',#42378);
#9774=VERTEX_POINT('',#42380);
#9775=VERTEX_POINT('',#42382);
#9776=VERTEX_POINT('',#42386);
#9777=VERTEX_POINT('',#42389);
#9778=VERTEX_POINT('',#42393);
#9779=VERTEX_POINT('',#42395);
#9780=VERTEX_POINT('',#42397);
#9781=VERTEX_POINT('',#42401);
#9782=VERTEX_POINT('',#42404);
#9783=VERTEX_POINT('',#42408);
#9784=VERTEX_POINT('',#42410);
#9785=VERTEX_POINT('',#42412);
#9786=VERTEX_POINT('',#42416);
#9787=VERTEX_POINT('',#42419);
#9788=VERTEX_POINT('',#42423);
#9789=VERTEX_POINT('',#42425);
#9790=VERTEX_POINT('',#42427);
#9791=VERTEX_POINT('',#42431);
#9792=VERTEX_POINT('',#42434);
#9793=VERTEX_POINT('',#42438);
#9794=VERTEX_POINT('',#42439);
#9795=VERTEX_POINT('',#42441);
#9796=VERTEX_POINT('',#42461);
#9797=VERTEX_POINT('',#42463);
#9798=VERTEX_POINT('',#42465);
#9799=VERTEX_POINT('',#42476);
#9800=VERTEX_POINT('',#42478);
#9801=VERTEX_POINT('',#42495);
#9802=VERTEX_POINT('',#42497);
#9803=VERTEX_POINT('',#42514);
#9804=VERTEX_POINT('',#42516);
#9805=VERTEX_POINT('',#42527);
#9806=VERTEX_POINT('',#42539);
#9807=VERTEX_POINT('',#42541);
#9808=VERTEX_POINT('',#42558);
#9809=VERTEX_POINT('',#42571);
#9810=VERTEX_POINT('',#42576);
#9811=VERTEX_POINT('',#42579);
#9812=VERTEX_POINT('',#42582);
#9813=VERTEX_POINT('',#42585);
#9814=VERTEX_POINT('',#42597);
#9815=VERTEX_POINT('',#42599);
#9816=VERTEX_POINT('',#42603);
#9817=VERTEX_POINT('',#42605);
#9818=VERTEX_POINT('',#42643);
#9819=VERTEX_POINT('',#42646);
#9820=VERTEX_POINT('',#42650);
#9821=VERTEX_POINT('',#42652);
#9822=VERTEX_POINT('',#42690);
#9823=VERTEX_POINT('',#42691);
#9824=VERTEX_POINT('',#42694);
#9825=VERTEX_POINT('',#42698);
#9826=VERTEX_POINT('',#42701);
#9827=VERTEX_POINT('',#42705);
#9828=VERTEX_POINT('',#42707);
#9829=VERTEX_POINT('',#42709);
#9830=VERTEX_POINT('',#42713);
#9831=VERTEX_POINT('',#42717);
#9832=VERTEX_POINT('',#42720);
#9833=VERTEX_POINT('',#42722);
#9834=VERTEX_POINT('',#42728);
#9835=VERTEX_POINT('',#42732);
#9836=VERTEX_POINT('',#42738);
#9837=VERTEX_POINT('',#42742);
#9838=VERTEX_POINT('',#42748);
#9839=VERTEX_POINT('',#42751);
#9840=VERTEX_POINT('',#42755);
#9841=VERTEX_POINT('',#42758);
#9842=VERTEX_POINT('',#42762);
#9843=VERTEX_POINT('',#42765);
#9844=VERTEX_POINT('',#42769);
#9845=VERTEX_POINT('',#42772);
#9846=VERTEX_POINT('',#42778);
#9847=VERTEX_POINT('',#42780);
#9848=VERTEX_POINT('',#42784);
#9849=VERTEX_POINT('',#42788);
#9850=VERTEX_POINT('',#42789);
#9851=VERTEX_POINT('',#42791);
#9852=VERTEX_POINT('',#42793);
#9853=VERTEX_POINT('',#42796);
#9854=VERTEX_POINT('',#42798);
#9855=VERTEX_POINT('',#42800);
#9856=VERTEX_POINT('',#42802);
#9857=VERTEX_POINT('',#42804);
#9858=VERTEX_POINT('',#42806);
#9859=VERTEX_POINT('',#42808);
#9860=VERTEX_POINT('',#42811);
#9861=VERTEX_POINT('',#42815);
#9862=VERTEX_POINT('',#42816);
#9863=VERTEX_POINT('',#42818);
#9864=VERTEX_POINT('',#42820);
#9865=VERTEX_POINT('',#42823);
#9866=VERTEX_POINT('',#42825);
#9867=VERTEX_POINT('',#42827);
#9868=VERTEX_POINT('',#42829);
#9869=VERTEX_POINT('',#42830);
#9870=VERTEX_POINT('',#42832);
#9871=VERTEX_POINT('',#42834);
#9872=VERTEX_POINT('',#42837);
#9873=VERTEX_POINT('',#42838);
#9874=VERTEX_POINT('',#42840);
#9875=VERTEX_POINT('',#42842);
#9876=VERTEX_POINT('',#42845);
#9877=VERTEX_POINT('',#42847);
#9878=VERTEX_POINT('',#42849);
#9879=VERTEX_POINT('',#42852);
#9880=VERTEX_POINT('',#42856);
#9881=VERTEX_POINT('',#42862);
#9882=VERTEX_POINT('',#42866);
#9883=VERTEX_POINT('',#42872);
#9884=VERTEX_POINT('',#42876);
#9885=VERTEX_POINT('',#42882);
#9886=VERTEX_POINT('',#42886);
#9887=VERTEX_POINT('',#42892);
#9888=VERTEX_POINT('',#42896);
#9889=VERTEX_POINT('',#42902);
#9890=VERTEX_POINT('',#42903);
#9891=VERTEX_POINT('',#42942);
#9892=VERTEX_POINT('',#42944);
#9893=VERTEX_POINT('',#42948);
#9894=VERTEX_POINT('',#42952);
#9895=VERTEX_POINT('',#42956);
#9896=VERTEX_POINT('',#42961);
#9897=VERTEX_POINT('',#42965);
#9898=VERTEX_POINT('',#42971);
#9899=VERTEX_POINT('',#42973);
#9900=VERTEX_POINT('',#42977);
#9901=VERTEX_POINT('',#42981);
#9902=VERTEX_POINT('',#42985);
#9903=VERTEX_POINT('',#42990);
#9904=VERTEX_POINT('',#42994);
#9905=VERTEX_POINT('',#43000);
#9906=VERTEX_POINT('',#43002);
#9907=VERTEX_POINT('',#43004);
#9908=VERTEX_POINT('',#43015);
#9909=VERTEX_POINT('',#43017);
#9910=VERTEX_POINT('',#43019);
#9911=VERTEX_POINT('',#43032);
#9912=VERTEX_POINT('',#43033);
#9913=VERTEX_POINT('',#43048);
#9914=VERTEX_POINT('',#43053);
#9915=VERTEX_POINT('',#43063);
#9916=VERTEX_POINT('',#43073);
#9917=VERTEX_POINT('',#43076);
#9918=VERTEX_POINT('',#43079);
#9919=VERTEX_POINT('',#43083);
#9920=VERTEX_POINT('',#43092);
#9921=VERTEX_POINT('',#43093);
#9922=VERTEX_POINT('',#43095);
#9923=VERTEX_POINT('',#43106);
#9924=VERTEX_POINT('',#43109);
#9925=VERTEX_POINT('',#43120);
#9926=VERTEX_POINT('',#43124);
#9927=VERTEX_POINT('',#43125);
#9928=VERTEX_POINT('',#43140);
#9929=VERTEX_POINT('',#43144);
#9930=VERTEX_POINT('',#43146);
#9931=VERTEX_POINT('',#43156);
#9932=VERTEX_POINT('',#43168);
#9933=VERTEX_POINT('',#43171);
#9934=VERTEX_POINT('',#43175);
#9935=VERTEX_POINT('',#43179);
#9936=VERTEX_POINT('',#43188);
#9937=VERTEX_POINT('',#43197);
#9938=VERTEX_POINT('',#43199);
#9939=VERTEX_POINT('',#43203);
#9940=VERTEX_POINT('',#43204);
#9941=VERTEX_POINT('',#43222);
#9942=VERTEX_POINT('',#43223);
#9943=VERTEX_POINT('',#43227);
#9944=VERTEX_POINT('',#43229);
#9945=VERTEX_POINT('',#43240);
#9946=VERTEX_POINT('',#43244);
#9947=VERTEX_POINT('',#43255);
#9948=VERTEX_POINT('',#43259);
#9949=VERTEX_POINT('',#43270);
#9950=VERTEX_POINT('',#43274);
#9951=VERTEX_POINT('',#43285);
#9952=VERTEX_POINT('',#43289);
#9953=VERTEX_POINT('',#43300);
#9954=VERTEX_POINT('',#43304);
#9955=VERTEX_POINT('',#43315);
#9956=VERTEX_POINT('',#43319);
#9957=VERTEX_POINT('',#43330);
#9958=VERTEX_POINT('',#43334);
#9959=VERTEX_POINT('',#43345);
#9960=VERTEX_POINT('',#43349);
#9961=VERTEX_POINT('',#43363);
#9962=VERTEX_POINT('',#43364);
#9963=VERTEX_POINT('',#43368);
#9964=VERTEX_POINT('',#43370);
#9965=VERTEX_POINT('',#43381);
#9966=VERTEX_POINT('',#43385);
#9967=VERTEX_POINT('',#43391);
#9968=VERTEX_POINT('',#43393);
#9969=VERTEX_POINT('',#43402);
#9970=VERTEX_POINT('',#43406);
#9971=VERTEX_POINT('',#43417);
#9972=VERTEX_POINT('',#43421);
#9973=VERTEX_POINT('',#43432);
#9974=VERTEX_POINT('',#43436);
#9975=VERTEX_POINT('',#43447);
#9976=VERTEX_POINT('',#43451);
#9977=VERTEX_POINT('',#43462);
#9978=VERTEX_POINT('',#43466);
#9979=VERTEX_POINT('',#43477);
#9980=VERTEX_POINT('',#43481);
#9981=VERTEX_POINT('',#43492);
#9982=VERTEX_POINT('',#43496);
#9983=VERTEX_POINT('',#43502);
#9984=VERTEX_POINT('',#43504);
#9985=VERTEX_POINT('',#43513);
#9986=VERTEX_POINT('',#43517);
#9987=VERTEX_POINT('',#43528);
#9988=VERTEX_POINT('',#43532);
#9989=VERTEX_POINT('',#43543);
#9990=VERTEX_POINT('',#43547);
#9991=VERTEX_POINT('',#43558);
#9992=VERTEX_POINT('',#43562);
#9993=VERTEX_POINT('',#43573);
#9994=VERTEX_POINT('',#43577);
#9995=VERTEX_POINT('',#43588);
#9996=VERTEX_POINT('',#43592);
#9997=VERTEX_POINT('',#43603);
#9998=VERTEX_POINT('',#43607);
#9999=VERTEX_POINT('',#43618);
#10000=VERTEX_POINT('',#43622);
#10001=VERTEX_POINT('',#43633);
#10002=VERTEX_POINT('',#43637);
#10003=VERTEX_POINT('',#43648);
#10004=VERTEX_POINT('',#43652);
#10005=VERTEX_POINT('',#43663);
#10006=VERTEX_POINT('',#43667);
#10007=VERTEX_POINT('',#43678);
#10008=VERTEX_POINT('',#43682);
#10009=VERTEX_POINT('',#43693);
#10010=VERTEX_POINT('',#43697);
#10011=VERTEX_POINT('',#43708);
#10012=VERTEX_POINT('',#43712);
#10013=VERTEX_POINT('',#43723);
#10014=VERTEX_POINT('',#43727);
#10015=VERTEX_POINT('',#43742);
#10016=VERTEX_POINT('',#43743);
#10017=VERTEX_POINT('',#43747);
#10018=VERTEX_POINT('',#43749);
#10019=VERTEX_POINT('',#43760);
#10020=VERTEX_POINT('',#43764);
#10021=VERTEX_POINT('',#43775);
#10022=VERTEX_POINT('',#43779);
#10023=VERTEX_POINT('',#43790);
#10024=VERTEX_POINT('',#43794);
#10025=VERTEX_POINT('',#43805);
#10026=VERTEX_POINT('',#43809);
#10027=VERTEX_POINT('',#43820);
#10028=VERTEX_POINT('',#43824);
#10029=VERTEX_POINT('',#43835);
#10030=VERTEX_POINT('',#43839);
#10031=VERTEX_POINT('',#43862);
#10032=VERTEX_POINT('',#43863);
#10033=VERTEX_POINT('',#43867);
#10034=VERTEX_POINT('',#43869);
#10035=VERTEX_POINT('',#43880);
#10036=VERTEX_POINT('',#43884);
#10037=VERTEX_POINT('',#43895);
#10038=VERTEX_POINT('',#43899);
#10039=VERTEX_POINT('',#43910);
#10040=VERTEX_POINT('',#43914);
#10041=VERTEX_POINT('',#43925);
#10042=VERTEX_POINT('',#43929);
#10043=VERTEX_POINT('',#43940);
#10044=VERTEX_POINT('',#43944);
#10045=VERTEX_POINT('',#43955);
#10046=VERTEX_POINT('',#43959);
#10047=VERTEX_POINT('',#43970);
#10048=VERTEX_POINT('',#43974);
#10049=VERTEX_POINT('',#43985);
#10050=VERTEX_POINT('',#43989);
#10051=VERTEX_POINT('',#44000);
#10052=VERTEX_POINT('',#44004);
#10053=VERTEX_POINT('',#44015);
#10054=VERTEX_POINT('',#44019);
#10055=VERTEX_POINT('',#44043);
#10056=VERTEX_POINT('',#44044);
#10057=VERTEX_POINT('',#44048);
#10058=VERTEX_POINT('',#44050);
#10059=VERTEX_POINT('',#44061);
#10060=VERTEX_POINT('',#44065);
#10061=VERTEX_POINT('',#44071);
#10062=VERTEX_POINT('',#44073);
#10063=VERTEX_POINT('',#44082);
#10064=VERTEX_POINT('',#44086);
#10065=VERTEX_POINT('',#44097);
#10066=VERTEX_POINT('',#44101);
#10067=VERTEX_POINT('',#44107);
#10068=VERTEX_POINT('',#44109);
#10069=VERTEX_POINT('',#44113);
#10070=VERTEX_POINT('',#44115);
#10071=VERTEX_POINT('',#44119);
#10072=VERTEX_POINT('',#44121);
#10073=VERTEX_POINT('',#44129);
#10074=VERTEX_POINT('',#44130);
#10075=VERTEX_POINT('',#44132);
#10076=VERTEX_POINT('',#44134);
#10077=VERTEX_POINT('',#44138);
#10078=VERTEX_POINT('',#44140);
#10079=VERTEX_POINT('',#44144);
#10080=VERTEX_POINT('',#44146);
#10081=VERTEX_POINT('',#44150);
#10082=VERTEX_POINT('',#44152);
#10083=VERTEX_POINT('',#44156);
#10084=VERTEX_POINT('',#44158);
#10085=VERTEX_POINT('',#44162);
#10086=VERTEX_POINT('',#44164);
#10087=VERTEX_POINT('',#44168);
#10088=VERTEX_POINT('',#44170);
#10089=VERTEX_POINT('',#44174);
#10090=VERTEX_POINT('',#44176);
#10091=VERTEX_POINT('',#44185);
#10092=VERTEX_POINT('',#44189);
#10093=VERTEX_POINT('',#44200);
#10094=VERTEX_POINT('',#44204);
#10095=VERTEX_POINT('',#44210);
#10096=VERTEX_POINT('',#44212);
#10097=VERTEX_POINT('',#44216);
#10098=VERTEX_POINT('',#44218);
#10099=VERTEX_POINT('',#44222);
#10100=VERTEX_POINT('',#44224);
#10101=VERTEX_POINT('',#44228);
#10102=VERTEX_POINT('',#44230);
#10103=VERTEX_POINT('',#44243);
#10104=VERTEX_POINT('',#44244);
#10105=VERTEX_POINT('',#44248);
#10106=VERTEX_POINT('',#44250);
#10107=VERTEX_POINT('',#44261);
#10108=VERTEX_POINT('',#44265);
#10109=VERTEX_POINT('',#44276);
#10110=VERTEX_POINT('',#44280);
#10111=VERTEX_POINT('',#44291);
#10112=VERTEX_POINT('',#44295);
#10113=VERTEX_POINT('',#44306);
#10114=VERTEX_POINT('',#44310);
#10115=VERTEX_POINT('',#44321);
#10116=VERTEX_POINT('',#44325);
#10117=VERTEX_POINT('',#44336);
#10118=VERTEX_POINT('',#44340);
#10119=VERTEX_POINT('',#44351);
#10120=VERTEX_POINT('',#44355);
#10121=VERTEX_POINT('',#44366);
#10122=VERTEX_POINT('',#44370);
#10123=VERTEX_POINT('',#44381);
#10124=VERTEX_POINT('',#44385);
#10125=VERTEX_POINT('',#44396);
#10126=VERTEX_POINT('',#44400);
#10127=VERTEX_POINT('',#44406);
#10128=VERTEX_POINT('',#44408);
#10129=VERTEX_POINT('',#44417);
#10130=VERTEX_POINT('',#44421);
#10131=VERTEX_POINT('',#44432);
#10132=VERTEX_POINT('',#44436);
#10133=VERTEX_POINT('',#44447);
#10134=VERTEX_POINT('',#44451);
#10135=VERTEX_POINT('',#44462);
#10136=VERTEX_POINT('',#44466);
#10137=VERTEX_POINT('',#44477);
#10138=VERTEX_POINT('',#44481);
#10139=VERTEX_POINT('',#44492);
#10140=VERTEX_POINT('',#44496);
#10141=VERTEX_POINT('',#44507);
#10142=VERTEX_POINT('',#44511);
#10143=VERTEX_POINT('',#44517);
#10144=VERTEX_POINT('',#44519);
#10145=VERTEX_POINT('',#44528);
#10146=VERTEX_POINT('',#44532);
#10147=VERTEX_POINT('',#44543);
#10148=VERTEX_POINT('',#44547);
#10149=VERTEX_POINT('',#44558);
#10150=VERTEX_POINT('',#44562);
#10151=VERTEX_POINT('',#44573);
#10152=VERTEX_POINT('',#44577);
#10153=VERTEX_POINT('',#44588);
#10154=VERTEX_POINT('',#44592);
#10155=VERTEX_POINT('',#44603);
#10156=VERTEX_POINT('',#44607);
#10157=VERTEX_POINT('',#44618);
#10158=VERTEX_POINT('',#44622);
#10159=VERTEX_POINT('',#44628);
#10160=VERTEX_POINT('',#44630);
#10161=VERTEX_POINT('',#44639);
#10162=VERTEX_POINT('',#44643);
#10163=VERTEX_POINT('',#44662);
#10164=VERTEX_POINT('',#44663);
#10165=VERTEX_POINT('',#44665);
#10166=VERTEX_POINT('',#44667);
#10167=VERTEX_POINT('',#44671);
#10168=VERTEX_POINT('',#44673);
#10169=VERTEX_POINT('',#44677);
#10170=VERTEX_POINT('',#44679);
#10171=VERTEX_POINT('',#44692);
#10172=VERTEX_POINT('',#44693);
#10173=VERTEX_POINT('',#44697);
#10174=VERTEX_POINT('',#44699);
#10175=VERTEX_POINT('',#44710);
#10176=VERTEX_POINT('',#44714);
#10177=VERTEX_POINT('',#44720);
#10178=VERTEX_POINT('',#44722);
#10179=VERTEX_POINT('',#44726);
#10180=VERTEX_POINT('',#44728);
#10181=VERTEX_POINT('',#44735);
#10182=VERTEX_POINT('',#44736);
#10183=VERTEX_POINT('',#44738);
#10184=VERTEX_POINT('',#44740);
#10185=VERTEX_POINT('',#44744);
#10186=VERTEX_POINT('',#44746);
#10187=VERTEX_POINT('',#44750);
#10188=VERTEX_POINT('',#44752);
#10189=VERTEX_POINT('',#44756);
#10190=VERTEX_POINT('',#44758);
#10191=VERTEX_POINT('',#44762);
#10192=VERTEX_POINT('',#44764);
#10193=VERTEX_POINT('',#44768);
#10194=VERTEX_POINT('',#44770);
#10195=VERTEX_POINT('',#44774);
#10196=VERTEX_POINT('',#44776);
#10197=VERTEX_POINT('',#44789);
#10198=VERTEX_POINT('',#44790);
#10199=VERTEX_POINT('',#44794);
#10200=VERTEX_POINT('',#44796);
#10201=VERTEX_POINT('',#44807);
#10202=VERTEX_POINT('',#44811);
#10203=VERTEX_POINT('',#44822);
#10204=VERTEX_POINT('',#44826);
#10205=VERTEX_POINT('',#44837);
#10206=VERTEX_POINT('',#44841);
#10207=VERTEX_POINT('',#44852);
#10208=VERTEX_POINT('',#44856);
#10209=VERTEX_POINT('',#44867);
#10210=VERTEX_POINT('',#44871);
#10211=VERTEX_POINT('',#44882);
#10212=VERTEX_POINT('',#44886);
#10213=VERTEX_POINT('',#44897);
#10214=VERTEX_POINT('',#44901);
#10215=VERTEX_POINT('',#44912);
#10216=VERTEX_POINT('',#44916);
#10217=VERTEX_POINT('',#44927);
#10218=VERTEX_POINT('',#44931);
#10219=VERTEX_POINT('',#44942);
#10220=VERTEX_POINT('',#44946);
#10221=VERTEX_POINT('',#44957);
#10222=VERTEX_POINT('',#44961);
#10223=VERTEX_POINT('',#44972);
#10224=VERTEX_POINT('',#44976);
#10225=VERTEX_POINT('',#44982);
#10226=VERTEX_POINT('',#44984);
#10227=VERTEX_POINT('',#44993);
#10228=VERTEX_POINT('',#44997);
#10229=VERTEX_POINT('',#45008);
#10230=VERTEX_POINT('',#45012);
#10231=VERTEX_POINT('',#45023);
#10232=VERTEX_POINT('',#45027);
#10233=VERTEX_POINT('',#45038);
#10234=VERTEX_POINT('',#45042);
#10235=VERTEX_POINT('',#45053);
#10236=VERTEX_POINT('',#45057);
#10237=VERTEX_POINT('',#45068);
#10238=VERTEX_POINT('',#45072);
#10239=VERTEX_POINT('',#45083);
#10240=VERTEX_POINT('',#45087);
#10241=VERTEX_POINT('',#45098);
#10242=VERTEX_POINT('',#45102);
#10243=VERTEX_POINT('',#45113);
#10244=VERTEX_POINT('',#45117);
#10245=VERTEX_POINT('',#45128);
#10246=VERTEX_POINT('',#45132);
#10247=VERTEX_POINT('',#45143);
#10248=VERTEX_POINT('',#45147);
#10249=VERTEX_POINT('',#45158);
#10250=VERTEX_POINT('',#45162);
#10251=VERTEX_POINT('',#45173);
#10252=VERTEX_POINT('',#45177);
#10253=VERTEX_POINT('',#45188);
#10254=VERTEX_POINT('',#45192);
#10255=VERTEX_POINT('',#45203);
#10256=VERTEX_POINT('',#45207);
#10257=VERTEX_POINT('',#45218);
#10258=VERTEX_POINT('',#45222);
#10259=VERTEX_POINT('',#45233);
#10260=VERTEX_POINT('',#45237);
#10261=VERTEX_POINT('',#45248);
#10262=VERTEX_POINT('',#45252);
#10263=VERTEX_POINT('',#45258);
#10264=VERTEX_POINT('',#45260);
#10265=VERTEX_POINT('',#45269);
#10266=VERTEX_POINT('',#45273);
#10267=VERTEX_POINT('',#45297);
#10268=VERTEX_POINT('',#45298);
#10269=VERTEX_POINT('',#45302);
#10270=VERTEX_POINT('',#45304);
#10271=VERTEX_POINT('',#45315);
#10272=VERTEX_POINT('',#45319);
#10273=VERTEX_POINT('',#45330);
#10274=VERTEX_POINT('',#45334);
#10275=VERTEX_POINT('',#45345);
#10276=VERTEX_POINT('',#45349);
#10277=VERTEX_POINT('',#45360);
#10278=VERTEX_POINT('',#45364);
#10279=VERTEX_POINT('',#45375);
#10280=VERTEX_POINT('',#45379);
#10281=VERTEX_POINT('',#45390);
#10282=VERTEX_POINT('',#45394);
#10283=VERTEX_POINT('',#45405);
#10284=VERTEX_POINT('',#45409);
#10285=VERTEX_POINT('',#45420);
#10286=VERTEX_POINT('',#45424);
#10287=VERTEX_POINT('',#45435);
#10288=VERTEX_POINT('',#45439);
#10289=VERTEX_POINT('',#45450);
#10290=VERTEX_POINT('',#45454);
#10291=VERTEX_POINT('',#45460);
#10292=VERTEX_POINT('',#45462);
#10293=VERTEX_POINT('',#45471);
#10294=VERTEX_POINT('',#45475);
#10295=VERTEX_POINT('',#45486);
#10296=VERTEX_POINT('',#45490);
#10297=VERTEX_POINT('',#45501);
#10298=VERTEX_POINT('',#45505);
#10299=VERTEX_POINT('',#45516);
#10300=VERTEX_POINT('',#45520);
#10301=VERTEX_POINT('',#45531);
#10302=VERTEX_POINT('',#45535);
#10303=VERTEX_POINT('',#45546);
#10304=VERTEX_POINT('',#45550);
#10305=VERTEX_POINT('',#45561);
#10306=VERTEX_POINT('',#45565);
#10307=VERTEX_POINT('',#45571);
#10308=VERTEX_POINT('',#45573);
#10309=VERTEX_POINT('',#45582);
#10310=VERTEX_POINT('',#45586);
#10311=VERTEX_POINT('',#45597);
#10312=VERTEX_POINT('',#45601);
#10313=VERTEX_POINT('',#45612);
#10314=VERTEX_POINT('',#45616);
#10315=VERTEX_POINT('',#45627);
#10316=VERTEX_POINT('',#45631);
#10317=VERTEX_POINT('',#45642);
#10318=VERTEX_POINT('',#45646);
#10319=VERTEX_POINT('',#45657);
#10320=VERTEX_POINT('',#45661);
#10321=VERTEX_POINT('',#45672);
#10322=VERTEX_POINT('',#45676);
#10323=VERTEX_POINT('',#45682);
#10324=VERTEX_POINT('',#45684);
#10325=VERTEX_POINT('',#45693);
#10326=VERTEX_POINT('',#45697);
#10327=VERTEX_POINT('',#45721);
#10328=VERTEX_POINT('',#45722);
#10329=VERTEX_POINT('',#45726);
#10330=VERTEX_POINT('',#45728);
#10331=VERTEX_POINT('',#45739);
#10332=VERTEX_POINT('',#45743);
#10333=VERTEX_POINT('',#45754);
#10334=VERTEX_POINT('',#45758);
#10335=VERTEX_POINT('',#45769);
#10336=VERTEX_POINT('',#45773);
#10337=VERTEX_POINT('',#45784);
#10338=VERTEX_POINT('',#45788);
#10339=VERTEX_POINT('',#45799);
#10340=VERTEX_POINT('',#45803);
#10341=VERTEX_POINT('',#45814);
#10342=VERTEX_POINT('',#45818);
#10343=VERTEX_POINT('',#45829);
#10344=VERTEX_POINT('',#45833);
#10345=VERTEX_POINT('',#45839);
#10346=VERTEX_POINT('',#45841);
#10347=VERTEX_POINT('',#45850);
#10348=VERTEX_POINT('',#45854);
#10349=VERTEX_POINT('',#45865);
#10350=VERTEX_POINT('',#45869);
#10351=VERTEX_POINT('',#45880);
#10352=VERTEX_POINT('',#45884);
#10353=VERTEX_POINT('',#45895);
#10354=VERTEX_POINT('',#45899);
#10355=VERTEX_POINT('',#45910);
#10356=VERTEX_POINT('',#45914);
#10357=VERTEX_POINT('',#45925);
#10358=VERTEX_POINT('',#45929);
#10359=VERTEX_POINT('',#45940);
#10360=VERTEX_POINT('',#45944);
#10361=VERTEX_POINT('',#45955);
#10362=VERTEX_POINT('',#45959);
#10363=VERTEX_POINT('',#45970);
#10364=VERTEX_POINT('',#45974);
#10365=VERTEX_POINT('',#45980);
#10366=VERTEX_POINT('',#45982);
#10367=VERTEX_POINT('',#45986);
#10368=VERTEX_POINT('',#45988);
#10369=VERTEX_POINT('',#45992);
#10370=VERTEX_POINT('',#45994);
#10371=VERTEX_POINT('',#46011);
#10372=VERTEX_POINT('',#46012);
#10373=VERTEX_POINT('',#46014);
#10374=VERTEX_POINT('',#46016);
#10375=VERTEX_POINT('',#46025);
#10376=VERTEX_POINT('',#46029);
#10377=VERTEX_POINT('',#46040);
#10378=VERTEX_POINT('',#46044);
#10379=VERTEX_POINT('',#46055);
#10380=VERTEX_POINT('',#46059);
#10381=VERTEX_POINT('',#46070);
#10382=VERTEX_POINT('',#46074);
#10383=VERTEX_POINT('',#46085);
#10384=VERTEX_POINT('',#46089);
#10385=VERTEX_POINT('',#46095);
#10386=VERTEX_POINT('',#46097);
#10387=VERTEX_POINT('',#46104);
#10388=VERTEX_POINT('',#46105);
#10389=VERTEX_POINT('',#46107);
#10390=VERTEX_POINT('',#46109);
#10391=VERTEX_POINT('',#46118);
#10392=VERTEX_POINT('',#46122);
#10393=VERTEX_POINT('',#46133);
#10394=VERTEX_POINT('',#46137);
#10395=VERTEX_POINT('',#46148);
#10396=VERTEX_POINT('',#46152);
#10397=VERTEX_POINT('',#46163);
#10398=VERTEX_POINT('',#46167);
#10399=VERTEX_POINT('',#46178);
#10400=VERTEX_POINT('',#46182);
#10401=VERTEX_POINT('',#46193);
#10402=VERTEX_POINT('',#46197);
#10403=VERTEX_POINT('',#46203);
#10404=VERTEX_POINT('',#46205);
#10405=VERTEX_POINT('',#46209);
#10406=VERTEX_POINT('',#46211);
#10407=VERTEX_POINT('',#46215);
#10408=VERTEX_POINT('',#46217);
#10409=VERTEX_POINT('',#46230);
#10410=VERTEX_POINT('',#46231);
#10411=VERTEX_POINT('',#46235);
#10412=VERTEX_POINT('',#46237);
#10413=VERTEX_POINT('',#46248);
#10414=VERTEX_POINT('',#46252);
#10415=VERTEX_POINT('',#46263);
#10416=VERTEX_POINT('',#46267);
#10417=VERTEX_POINT('',#46278);
#10418=VERTEX_POINT('',#46282);
#10419=VERTEX_POINT('',#46293);
#10420=VERTEX_POINT('',#46297);
#10421=VERTEX_POINT('',#46308);
#10422=VERTEX_POINT('',#46312);
#10423=VERTEX_POINT('',#46323);
#10424=VERTEX_POINT('',#46327);
#10425=VERTEX_POINT('',#46338);
#10426=VERTEX_POINT('',#46342);
#10427=VERTEX_POINT('',#46365);
#10428=VERTEX_POINT('',#46366);
#10429=VERTEX_POINT('',#46370);
#10430=VERTEX_POINT('',#46372);
#10431=VERTEX_POINT('',#46383);
#10432=VERTEX_POINT('',#46387);
#10433=VERTEX_POINT('',#46398);
#10434=VERTEX_POINT('',#46402);
#10435=VERTEX_POINT('',#46413);
#10436=VERTEX_POINT('',#46417);
#10437=VERTEX_POINT('',#46428);
#10438=VERTEX_POINT('',#46432);
#10439=VERTEX_POINT('',#46443);
#10440=VERTEX_POINT('',#46447);
#10441=VERTEX_POINT('',#46458);
#10442=VERTEX_POINT('',#46462);
#10443=VERTEX_POINT('',#46473);
#10444=VERTEX_POINT('',#46477);
#10445=VERTEX_POINT('',#46488);
#10446=VERTEX_POINT('',#46492);
#10447=VERTEX_POINT('',#46503);
#10448=VERTEX_POINT('',#46507);
#10449=VERTEX_POINT('',#46518);
#10450=VERTEX_POINT('',#46522);
#10451=VERTEX_POINT('',#46533);
#10452=VERTEX_POINT('',#46537);
#10453=VERTEX_POINT('',#46548);
#10454=VERTEX_POINT('',#46552);
#10455=VERTEX_POINT('',#46563);
#10456=VERTEX_POINT('',#46567);
#10457=VERTEX_POINT('',#46578);
#10458=VERTEX_POINT('',#46582);
#10459=VERTEX_POINT('',#46593);
#10460=VERTEX_POINT('',#46597);
#10461=VERTEX_POINT('',#46603);
#10462=VERTEX_POINT('',#46605);
#10463=VERTEX_POINT('',#46614);
#10464=VERTEX_POINT('',#46618);
#10465=VERTEX_POINT('',#46642);
#10466=VERTEX_POINT('',#46643);
#10467=VERTEX_POINT('',#46647);
#10468=VERTEX_POINT('',#46649);
#10469=VERTEX_POINT('',#46660);
#10470=VERTEX_POINT('',#46664);
#10471=VERTEX_POINT('',#46675);
#10472=VERTEX_POINT('',#46679);
#10473=VERTEX_POINT('',#46690);
#10474=VERTEX_POINT('',#46694);
#10475=VERTEX_POINT('',#46705);
#10476=VERTEX_POINT('',#46709);
#10477=VERTEX_POINT('',#46720);
#10478=VERTEX_POINT('',#46724);
#10479=VERTEX_POINT('',#46735);
#10480=VERTEX_POINT('',#46739);
#10481=VERTEX_POINT('',#46762);
#10482=VERTEX_POINT('',#46763);
#10483=VERTEX_POINT('',#46767);
#10484=VERTEX_POINT('',#46769);
#10485=VERTEX_POINT('',#46780);
#10486=VERTEX_POINT('',#46784);
#10487=VERTEX_POINT('',#46795);
#10488=VERTEX_POINT('',#46799);
#10489=VERTEX_POINT('',#46810);
#10490=VERTEX_POINT('',#46814);
#10491=VERTEX_POINT('',#46825);
#10492=VERTEX_POINT('',#46829);
#10493=VERTEX_POINT('',#46840);
#10494=VERTEX_POINT('',#46844);
#10495=VERTEX_POINT('',#46855);
#10496=VERTEX_POINT('',#46859);
#10497=VERTEX_POINT('',#46865);
#10498=VERTEX_POINT('',#46867);
#10499=VERTEX_POINT('',#46871);
#10500=VERTEX_POINT('',#46873);
#10501=VERTEX_POINT('',#46877);
#10502=VERTEX_POINT('',#46879);
#10503=VERTEX_POINT('',#46883);
#10504=VERTEX_POINT('',#46885);
#10505=VERTEX_POINT('',#46889);
#10506=VERTEX_POINT('',#46891);
#10507=VERTEX_POINT('',#46913);
#10508=VERTEX_POINT('',#46914);
#10509=VERTEX_POINT('',#46918);
#10510=VERTEX_POINT('',#46920);
#10511=VERTEX_POINT('',#46931);
#10512=VERTEX_POINT('',#46935);
#10513=VERTEX_POINT('',#46946);
#10514=VERTEX_POINT('',#46950);
#10515=VERTEX_POINT('',#46961);
#10516=VERTEX_POINT('',#46965);
#10517=VERTEX_POINT('',#46971);
#10518=VERTEX_POINT('',#46973);
#10519=VERTEX_POINT('',#46982);
#10520=VERTEX_POINT('',#46986);
#10521=VERTEX_POINT('',#46997);
#10522=VERTEX_POINT('',#47001);
#10523=VERTEX_POINT('',#47012);
#10524=VERTEX_POINT('',#47016);
#10525=VERTEX_POINT('',#47022);
#10526=VERTEX_POINT('',#47024);
#10527=VERTEX_POINT('',#47028);
#10528=VERTEX_POINT('',#47030);
#10529=VERTEX_POINT('',#47034);
#10530=VERTEX_POINT('',#47036);
#10531=VERTEX_POINT('',#47040);
#10532=VERTEX_POINT('',#47042);
#10533=VERTEX_POINT('',#47056);
#10534=VERTEX_POINT('',#47058);
#10535=VERTEX_POINT('',#47060);
#10536=VERTEX_POINT('',#47071);
#10537=VERTEX_POINT('',#47082);
#10538=VERTEX_POINT('',#47104);
#10539=VERTEX_POINT('',#47106);
#10540=VERTEX_POINT('',#47110);
#10541=VERTEX_POINT('',#47114);
#10542=VERTEX_POINT('',#47115);
#10543=VERTEX_POINT('',#47117);
#10544=VERTEX_POINT('',#47144);
#10545=VERTEX_POINT('',#47148);
#10546=VERTEX_POINT('',#47149);
#10547=VERTEX_POINT('',#47154);
#10548=VERTEX_POINT('',#47161);
#10549=VERTEX_POINT('',#47163);
#10550=VERTEX_POINT('',#47168);
#10551=VERTEX_POINT('',#47172);
#10552=VERTEX_POINT('',#47174);
#10553=VERTEX_POINT('',#47178);
#10554=VERTEX_POINT('',#47180);
#10555=VERTEX_POINT('',#47182);
#10556=VERTEX_POINT('',#47184);
#10557=VERTEX_POINT('',#47186);
#10558=VERTEX_POINT('',#47188);
#10559=VERTEX_POINT('',#47190);
#10560=VERTEX_POINT('',#47193);
#10561=VERTEX_POINT('',#47197);
#10562=VERTEX_POINT('',#47201);
#10563=VERTEX_POINT('',#47205);
#10564=VERTEX_POINT('',#47209);
#10565=VERTEX_POINT('',#47213);
#10566=VERTEX_POINT('',#47217);
#10567=VERTEX_POINT('',#47221);
#10568=VERTEX_POINT('',#47225);
#10569=VERTEX_POINT('',#47229);
#10570=VERTEX_POINT('',#47233);
#10571=VERTEX_POINT('',#47237);
#10572=VERTEX_POINT('',#47240);
#10573=VERTEX_POINT('',#47243);
#10574=VERTEX_POINT('',#47246);
#10575=VERTEX_POINT('',#47249);
#10576=VERTEX_POINT('',#47252);
#10577=VERTEX_POINT('',#47255);
#10578=VERTEX_POINT('',#47257);
#10579=VERTEX_POINT('',#47261);
#10580=VERTEX_POINT('',#47268);
#10581=VERTEX_POINT('',#47271);
#10582=VERTEX_POINT('',#47277);
#10583=VERTEX_POINT('',#47279);
#10584=VERTEX_POINT('',#47282);
#10585=VERTEX_POINT('',#47286);
#10586=VERTEX_POINT('',#47289);
#10587=VERTEX_POINT('',#47293);
#10588=VERTEX_POINT('',#47296);
#10589=VERTEX_POINT('',#47300);
#10590=VERTEX_POINT('',#47303);
#10591=VERTEX_POINT('',#47307);
#10592=VERTEX_POINT('',#47309);
#10593=VERTEX_POINT('',#47313);
#10594=VERTEX_POINT('',#47319);
#10595=VERTEX_POINT('',#47323);
#10596=VERTEX_POINT('',#47327);
#10597=VERTEX_POINT('',#47330);
#10598=VERTEX_POINT('',#47334);
#10599=VERTEX_POINT('',#47338);
#10600=VERTEX_POINT('',#47345);
#10601=VERTEX_POINT('',#47347);
#10602=VERTEX_POINT('',#47351);
#10603=VERTEX_POINT('',#47353);
#10604=VERTEX_POINT('',#47358);
#10605=VERTEX_POINT('',#47361);
#10606=VERTEX_POINT('',#47363);
#10607=VERTEX_POINT('',#47367);
#10608=VERTEX_POINT('',#47371);
#10609=VERTEX_POINT('',#47374);
#10610=VERTEX_POINT('',#47379);
#10611=VERTEX_POINT('',#47383);
#10612=VERTEX_POINT('',#47387);
#10613=VERTEX_POINT('',#47391);
#10614=VERTEX_POINT('',#47394);
#10615=VERTEX_POINT('',#47398);
#10616=VERTEX_POINT('',#47404);
#10617=VERTEX_POINT('',#47406);
#10618=VERTEX_POINT('',#47409);
#10619=VERTEX_POINT('',#47410);
#10620=VERTEX_POINT('',#47412);
#10621=VERTEX_POINT('',#47417);
#10622=VERTEX_POINT('',#47423);
#10623=VERTEX_POINT('',#47424);
#10624=VERTEX_POINT('',#47426);
#10625=VERTEX_POINT('',#47431);
#10626=VERTEX_POINT('',#47437);
#10627=VERTEX_POINT('',#47438);
#10628=VERTEX_POINT('',#47440);
#10629=VERTEX_POINT('',#47445);
#10630=VERTEX_POINT('',#47451);
#10631=VERTEX_POINT('',#47452);
#10632=VERTEX_POINT('',#47454);
#10633=VERTEX_POINT('',#47459);
#10634=VERTEX_POINT('',#47465);
#10635=VERTEX_POINT('',#47466);
#10636=VERTEX_POINT('',#47468);
#10637=VERTEX_POINT('',#47473);
#10638=VERTEX_POINT('',#47479);
#10639=VERTEX_POINT('',#47480);
#10640=VERTEX_POINT('',#47482);
#10641=VERTEX_POINT('',#47487);
#10642=VERTEX_POINT('',#47493);
#10643=VERTEX_POINT('',#47494);
#10644=VERTEX_POINT('',#47496);
#10645=VERTEX_POINT('',#47501);
#10646=VERTEX_POINT('',#47507);
#10647=VERTEX_POINT('',#47508);
#10648=VERTEX_POINT('',#47510);
#10649=VERTEX_POINT('',#47515);
#10650=VERTEX_POINT('',#47521);
#10651=VERTEX_POINT('',#47522);
#10652=VERTEX_POINT('',#47524);
#10653=VERTEX_POINT('',#47529);
#10654=VERTEX_POINT('',#47535);
#10655=VERTEX_POINT('',#47536);
#10656=VERTEX_POINT('',#47538);
#10657=VERTEX_POINT('',#47543);
#10658=VERTEX_POINT('',#47549);
#10659=VERTEX_POINT('',#47550);
#10660=VERTEX_POINT('',#47552);
#10661=VERTEX_POINT('',#47557);
#10662=VERTEX_POINT('',#47563);
#10663=VERTEX_POINT('',#47564);
#10664=VERTEX_POINT('',#47566);
#10665=VERTEX_POINT('',#47571);
#10666=VERTEX_POINT('',#47577);
#10667=VERTEX_POINT('',#47578);
#10668=VERTEX_POINT('',#47580);
#10669=VERTEX_POINT('',#47585);
#10670=VERTEX_POINT('',#47591);
#10671=VERTEX_POINT('',#47592);
#10672=VERTEX_POINT('',#47594);
#10673=VERTEX_POINT('',#47599);
#10674=VERTEX_POINT('',#47605);
#10675=VERTEX_POINT('',#47606);
#10676=VERTEX_POINT('',#47608);
#10677=VERTEX_POINT('',#47613);
#10678=VERTEX_POINT('',#47619);
#10679=VERTEX_POINT('',#47620);
#10680=VERTEX_POINT('',#47622);
#10681=VERTEX_POINT('',#47627);
#10682=VERTEX_POINT('',#47633);
#10683=VERTEX_POINT('',#47634);
#10684=VERTEX_POINT('',#47639);
#10685=VERTEX_POINT('',#47641);
#10686=VERTEX_POINT('',#47648);
#10687=VERTEX_POINT('',#47650);
#10688=VERTEX_POINT('',#47653);
#10689=VERTEX_POINT('',#47654);
#10690=VERTEX_POINT('',#47656);
#10691=VERTEX_POINT('',#47661);
#10692=VERTEX_POINT('',#47667);
#10693=VERTEX_POINT('',#47668);
#10694=VERTEX_POINT('',#47670);
#10695=VERTEX_POINT('',#47675);
#10696=VERTEX_POINT('',#47681);
#10697=VERTEX_POINT('',#47682);
#10698=VERTEX_POINT('',#47684);
#10699=VERTEX_POINT('',#47689);
#10700=VERTEX_POINT('',#47695);
#10701=VERTEX_POINT('',#47696);
#10702=VERTEX_POINT('',#47698);
#10703=VERTEX_POINT('',#47703);
#10704=VERTEX_POINT('',#47709);
#10705=VERTEX_POINT('',#47710);
#10706=VERTEX_POINT('',#47712);
#10707=VERTEX_POINT('',#47717);
#10708=VERTEX_POINT('',#47723);
#10709=VERTEX_POINT('',#47724);
#10710=VERTEX_POINT('',#47726);
#10711=VERTEX_POINT('',#47731);
#10712=VERTEX_POINT('',#47737);
#10713=VERTEX_POINT('',#47738);
#10714=VERTEX_POINT('',#47740);
#10715=VERTEX_POINT('',#47745);
#10716=VERTEX_POINT('',#47751);
#10717=VERTEX_POINT('',#47752);
#10718=VERTEX_POINT('',#47754);
#10719=VERTEX_POINT('',#47759);
#10720=VERTEX_POINT('',#47765);
#10721=VERTEX_POINT('',#47766);
#10722=VERTEX_POINT('',#47768);
#10723=VERTEX_POINT('',#47773);
#10724=VERTEX_POINT('',#47779);
#10725=VERTEX_POINT('',#47780);
#10726=VERTEX_POINT('',#47782);
#10727=VERTEX_POINT('',#47787);
#10728=VERTEX_POINT('',#47793);
#10729=VERTEX_POINT('',#47794);
#10730=VERTEX_POINT('',#47796);
#10731=VERTEX_POINT('',#47801);
#10732=VERTEX_POINT('',#47807);
#10733=VERTEX_POINT('',#47808);
#10734=VERTEX_POINT('',#47810);
#10735=VERTEX_POINT('',#47815);
#10736=VERTEX_POINT('',#47821);
#10737=VERTEX_POINT('',#47822);
#10738=VERTEX_POINT('',#47824);
#10739=VERTEX_POINT('',#47829);
#10740=VERTEX_POINT('',#47835);
#10741=VERTEX_POINT('',#47836);
#10742=VERTEX_POINT('',#47838);
#10743=VERTEX_POINT('',#47843);
#10744=VERTEX_POINT('',#47849);
#10745=VERTEX_POINT('',#47850);
#10746=VERTEX_POINT('',#47852);
#10747=VERTEX_POINT('',#47857);
#10748=VERTEX_POINT('',#47863);
#10749=VERTEX_POINT('',#47864);
#10750=VERTEX_POINT('',#47866);
#10751=VERTEX_POINT('',#47871);
#10752=VERTEX_POINT('',#47877);
#10753=VERTEX_POINT('',#47878);
#10754=VERTEX_POINT('',#47883);
#10755=VERTEX_POINT('',#47885);
#10756=VERTEX_POINT('',#47898);
#10757=VERTEX_POINT('',#47900);
#10758=VERTEX_POINT('',#47906);
#10759=VERTEX_POINT('',#47908);
#10760=VERTEX_POINT('',#47918);
#10761=VERTEX_POINT('',#47920);
#10762=VERTEX_POINT('',#47926);
#10763=VERTEX_POINT('',#47928);
#10764=VERTEX_POINT('',#47938);
#10765=VERTEX_POINT('',#47940);
#10766=VERTEX_POINT('',#47946);
#10767=VERTEX_POINT('',#47948);
#10768=VERTEX_POINT('',#47958);
#10769=VERTEX_POINT('',#47960);
#10770=VERTEX_POINT('',#47966);
#10771=VERTEX_POINT('',#47968);
#10772=VERTEX_POINT('',#47978);
#10773=VERTEX_POINT('',#47980);
#10774=VERTEX_POINT('',#47986);
#10775=VERTEX_POINT('',#47988);
#10776=VERTEX_POINT('',#47998);
#10777=VERTEX_POINT('',#48000);
#10778=VERTEX_POINT('',#48006);
#10779=VERTEX_POINT('',#48008);
#10780=VERTEX_POINT('',#48018);
#10781=VERTEX_POINT('',#48020);
#10782=VERTEX_POINT('',#48026);
#10783=VERTEX_POINT('',#48028);
#10784=VERTEX_POINT('',#48038);
#10785=VERTEX_POINT('',#48040);
#10786=VERTEX_POINT('',#48046);
#10787=VERTEX_POINT('',#48048);
#10788=VERTEX_POINT('',#48058);
#10789=VERTEX_POINT('',#48060);
#10790=VERTEX_POINT('',#48066);
#10791=VERTEX_POINT('',#48068);
#10792=VERTEX_POINT('',#48078);
#10793=VERTEX_POINT('',#48080);
#10794=VERTEX_POINT('',#48086);
#10795=VERTEX_POINT('',#48088);
#10796=VERTEX_POINT('',#48098);
#10797=VERTEX_POINT('',#48100);
#10798=VERTEX_POINT('',#48106);
#10799=VERTEX_POINT('',#48108);
#10800=VERTEX_POINT('',#48118);
#10801=VERTEX_POINT('',#48120);
#10802=VERTEX_POINT('',#48126);
#10803=VERTEX_POINT('',#48128);
#10804=VERTEX_POINT('',#48138);
#10805=VERTEX_POINT('',#48140);
#10806=VERTEX_POINT('',#48146);
#10807=VERTEX_POINT('',#48148);
#10808=VERTEX_POINT('',#48158);
#10809=VERTEX_POINT('',#48160);
#10810=VERTEX_POINT('',#48166);
#10811=VERTEX_POINT('',#48168);
#10812=VERTEX_POINT('',#48178);
#10813=VERTEX_POINT('',#48180);
#10814=VERTEX_POINT('',#48186);
#10815=VERTEX_POINT('',#48188);
#10816=VERTEX_POINT('',#48198);
#10817=VERTEX_POINT('',#48200);
#10818=VERTEX_POINT('',#48206);
#10819=VERTEX_POINT('',#48208);
#10820=VERTEX_POINT('',#48220);
#10821=VERTEX_POINT('',#48222);
#10822=VERTEX_POINT('',#48227);
#10823=VERTEX_POINT('',#48229);
#10824=VERTEX_POINT('',#48236);
#10825=VERTEX_POINT('',#48240);
#10826=VERTEX_POINT('',#48247);
#10827=VERTEX_POINT('',#48249);
#10828=VERTEX_POINT('',#48251);
#10829=VERTEX_POINT('',#48257);
#10830=VERTEX_POINT('',#48263);
#10831=VERTEX_POINT('',#48269);
#10832=VERTEX_POINT('',#48275);
#10833=VERTEX_POINT('',#48281);
#10834=VERTEX_POINT('',#48287);
#10835=VERTEX_POINT('',#48294);
#10836=VERTEX_POINT('',#48300);
#10837=VERTEX_POINT('',#48306);
#10838=VERTEX_POINT('',#48312);
#10839=VERTEX_POINT('',#48318);
#10840=VERTEX_POINT('',#48324);
#10841=VERTEX_POINT('',#48330);
#10842=VERTEX_POINT('',#48336);
#10843=VERTEX_POINT('',#48342);
#10844=VERTEX_POINT('',#48350);
#10845=VERTEX_POINT('',#48356);
#10846=VERTEX_POINT('',#48362);
#10847=VERTEX_POINT('',#48368);
#10848=VERTEX_POINT('',#48374);
#10849=VERTEX_POINT('',#48380);
#10850=VERTEX_POINT('',#48386);
#10851=VERTEX_POINT('',#48392);
#10852=VERTEX_POINT('',#48398);
#10853=VERTEX_POINT('',#48404);
#10854=VERTEX_POINT('',#48410);
#10855=VERTEX_POINT('',#48416);
#10856=VERTEX_POINT('',#48422);
#10857=VERTEX_POINT('',#48428);
#10858=VERTEX_POINT('',#48434);
#10859=VERTEX_POINT('',#48440);
#10860=VERTEX_POINT('',#48446);
#10861=VERTEX_POINT('',#48448);
#10862=VERTEX_POINT('',#48452);
#10863=VERTEX_POINT('',#48455);
#10864=VERTEX_POINT('',#48459);
#10865=VERTEX_POINT('',#48464);
#10866=VERTEX_POINT('',#48467);
#10867=VERTEX_POINT('',#48471);
#10868=VERTEX_POINT('',#48474);
#10869=VERTEX_POINT('',#48481);
#10870=VERTEX_POINT('',#48483);
#10871=VERTEX_POINT('',#48487);
#10872=VERTEX_POINT('',#48490);
#10873=VERTEX_POINT('',#48494);
#10874=VERTEX_POINT('',#48498);
#10875=VERTEX_POINT('',#48502);
#10876=VERTEX_POINT('',#48505);
#10877=VERTEX_POINT('',#48512);
#10878=VERTEX_POINT('',#48514);
#10879=VERTEX_POINT('',#48518);
#10880=VERTEX_POINT('',#48520);
#10881=VERTEX_POINT('',#48524);
#10882=VERTEX_POINT('',#48525);
#10883=VERTEX_POINT('',#48527);
#10884=VERTEX_POINT('',#48529);
#10885=VERTEX_POINT('',#48533);
#10886=VERTEX_POINT('',#48535);
#10887=VERTEX_POINT('',#48539);
#10888=VERTEX_POINT('',#48541);
#10889=VERTEX_POINT('',#48545);
#10890=VERTEX_POINT('',#48547);
#10891=VERTEX_POINT('',#48551);
#10892=VERTEX_POINT('',#48553);
#10893=VERTEX_POINT('',#48557);
#10894=VERTEX_POINT('',#48559);
#10895=VERTEX_POINT('',#48563);
#10896=VERTEX_POINT('',#48565);
#10897=VERTEX_POINT('',#48575);
#10898=VERTEX_POINT('',#48576);
#10899=VERTEX_POINT('',#48578);
#10900=VERTEX_POINT('',#48592);
#10901=VERTEX_POINT('',#48594);
#10902=VERTEX_POINT('',#48597);
#10903=VERTEX_POINT('',#48610);
#10904=VERTEX_POINT('',#48611);
#10905=VERTEX_POINT('',#48658);
#10906=VERTEX_POINT('',#48659);
#10907=VERTEX_POINT('',#48706);
#10908=VERTEX_POINT('',#48707);
#10909=VERTEX_POINT('',#48754);
#10910=VERTEX_POINT('',#48755);
#10911=VERTEX_POINT('',#48808);
#10912=VERTEX_POINT('',#48809);
#10913=VERTEX_POINT('',#48856);
#10914=VERTEX_POINT('',#48857);
#10915=VERTEX_POINT('',#48904);
#10916=VERTEX_POINT('',#48905);
#10917=VERTEX_POINT('',#48958);
#10918=VERTEX_POINT('',#48959);
#10919=VERTEX_POINT('',#49006);
#10920=VERTEX_POINT('',#49007);
#10921=VERTEX_POINT('',#49054);
#10922=VERTEX_POINT('',#49055);
#10923=VERTEX_POINT('',#49102);
#10924=VERTEX_POINT('',#49103);
#10925=VERTEX_POINT('',#49156);
#10926=VERTEX_POINT('',#49157);
#10927=VERTEX_POINT('',#49204);
#10928=VERTEX_POINT('',#49205);
#10929=VERTEX_POINT('',#49252);
#10930=VERTEX_POINT('',#49253);
#10931=VERTEX_POINT('',#49306);
#10932=VERTEX_POINT('',#49307);
#10933=VERTEX_POINT('',#49354);
#10934=VERTEX_POINT('',#49355);
#10935=VERTEX_POINT('',#49402);
#10936=VERTEX_POINT('',#49403);
#10937=VERTEX_POINT('',#49450);
#10938=VERTEX_POINT('',#49451);
#10939=VERTEX_POINT('',#49504);
#10940=VERTEX_POINT('',#49505);
#10941=VERTEX_POINT('',#49552);
#10942=VERTEX_POINT('',#49553);
#10943=VERTEX_POINT('',#49600);
#10944=VERTEX_POINT('',#49601);
#10945=VERTEX_POINT('',#49654);
#10946=VERTEX_POINT('',#49655);
#10947=VERTEX_POINT('',#49657);
#10948=VERTEX_POINT('',#49701);
#10949=VERTEX_POINT('',#49702);
#10950=VERTEX_POINT('',#49704);
#10951=VERTEX_POINT('',#49712);
#10952=VERTEX_POINT('',#49721);
#10953=VERTEX_POINT('',#49722);
#10954=VERTEX_POINT('',#49746);
#10955=VERTEX_POINT('',#49747);
#10956=VERTEX_POINT('',#49771);
#10957=VERTEX_POINT('',#49772);
#10958=VERTEX_POINT('',#49795);
#10959=VERTEX_POINT('',#49796);
#10960=VERTEX_POINT('',#49820);
#10961=VERTEX_POINT('',#49821);
#10962=VERTEX_POINT('',#49845);
#10963=VERTEX_POINT('',#49846);
#10964=VERTEX_POINT('',#49869);
#10965=VERTEX_POINT('',#49870);
#10966=VERTEX_POINT('',#49893);
#10967=VERTEX_POINT('',#49894);
#10968=VERTEX_POINT('',#49918);
#10969=VERTEX_POINT('',#49919);
#10970=VERTEX_POINT('',#49943);
#10971=VERTEX_POINT('',#49944);
#10972=VERTEX_POINT('',#49967);
#10973=VERTEX_POINT('',#49968);
#10974=VERTEX_POINT('',#49992);
#10975=VERTEX_POINT('',#49993);
#10976=VERTEX_POINT('',#50017);
#10977=VERTEX_POINT('',#50018);
#10978=VERTEX_POINT('',#50041);
#10979=VERTEX_POINT('',#50042);
#10980=VERTEX_POINT('',#50065);
#10981=VERTEX_POINT('',#50066);
#10982=VERTEX_POINT('',#50090);
#10983=VERTEX_POINT('',#50091);
#10984=VERTEX_POINT('',#50115);
#10985=VERTEX_POINT('',#50116);
#10986=VERTEX_POINT('',#50139);
#10987=VERTEX_POINT('',#50140);
#10988=VERTEX_POINT('',#50164);
#10989=VERTEX_POINT('',#50165);
#10990=VERTEX_POINT('',#50189);
#10991=VERTEX_POINT('',#50190);
#10992=VERTEX_POINT('',#50213);
#10993=VERTEX_POINT('',#50214);
#10994=VERTEX_POINT('',#50304);
#10995=VERTEX_POINT('',#50955);
#10996=VERTEX_POINT('',#51034);
#10997=VERTEX_POINT('',#51694);
#10998=VERTEX_POINT('',#51698);
#10999=VERTEX_POINT('',#51701);
#11000=VERTEX_POINT('',#51702);
#11001=VERTEX_POINT('',#51706);
#11002=VERTEX_POINT('',#51707);
#11003=VERTEX_POINT('',#51709);
#11004=VERTEX_POINT('',#51711);
#11005=VERTEX_POINT('',#51715);
#11006=VERTEX_POINT('',#51717);
#11007=VERTEX_POINT('',#51721);
#11008=VERTEX_POINT('',#51723);
#11009=VERTEX_POINT('',#51727);
#11010=VERTEX_POINT('',#51729);
#11011=VERTEX_POINT('',#51733);
#11012=VERTEX_POINT('',#51735);
#11013=VERTEX_POINT('',#51743);
#11014=VERTEX_POINT('',#51744);
#11015=VERTEX_POINT('',#51746);
#11016=VERTEX_POINT('',#51748);
#11017=VERTEX_POINT('',#51752);
#11018=VERTEX_POINT('',#51756);
#11019=VERTEX_POINT('',#51762);
#11020=VERTEX_POINT('',#51763);
#11021=VERTEX_POINT('',#51765);
#11022=VERTEX_POINT('',#51767);
#11023=VERTEX_POINT('',#51771);
#11024=VERTEX_POINT('',#51775);
#11025=VERTEX_POINT('',#51781);
#11026=VERTEX_POINT('',#51782);
#11027=VERTEX_POINT('',#51784);
#11028=VERTEX_POINT('',#51786);
#11029=VERTEX_POINT('',#51790);
#11030=VERTEX_POINT('',#51794);
#11031=VERTEX_POINT('',#51800);
#11032=VERTEX_POINT('',#51801);
#11033=VERTEX_POINT('',#51803);
#11034=VERTEX_POINT('',#51805);
#11035=VERTEX_POINT('',#51809);
#11036=VERTEX_POINT('',#51813);
#11037=VERTEX_POINT('',#51819);
#11038=VERTEX_POINT('',#51820);
#11039=VERTEX_POINT('',#51822);
#11040=VERTEX_POINT('',#51824);
#11041=VERTEX_POINT('',#51828);
#11042=VERTEX_POINT('',#51832);
#11043=VERTEX_POINT('',#51838);
#11044=VERTEX_POINT('',#51839);
#11045=VERTEX_POINT('',#51841);
#11046=VERTEX_POINT('',#51843);
#11047=VERTEX_POINT('',#51847);
#11048=VERTEX_POINT('',#51851);
#11049=VERTEX_POINT('',#51857);
#11050=VERTEX_POINT('',#51858);
#11051=VERTEX_POINT('',#51860);
#11052=VERTEX_POINT('',#51862);
#11053=VERTEX_POINT('',#51866);
#11054=VERTEX_POINT('',#51870);
#11055=VERTEX_POINT('',#51876);
#11056=VERTEX_POINT('',#51877);
#11057=VERTEX_POINT('',#51879);
#11058=VERTEX_POINT('',#51881);
#11059=VERTEX_POINT('',#51885);
#11060=VERTEX_POINT('',#51889);
#11061=VERTEX_POINT('',#51895);
#11062=VERTEX_POINT('',#51896);
#11063=VERTEX_POINT('',#51898);
#11064=VERTEX_POINT('',#51900);
#11065=VERTEX_POINT('',#51904);
#11066=VERTEX_POINT('',#51906);
#11067=VERTEX_POINT('',#51910);
#11068=VERTEX_POINT('',#51914);
#11069=VERTEX_POINT('',#51918);
#11070=VERTEX_POINT('',#51919);
#11071=VERTEX_POINT('',#51921);
#11072=VERTEX_POINT('',#51923);
#11073=VERTEX_POINT('',#51927);
#11074=VERTEX_POINT('',#51931);
#11075=VERTEX_POINT('',#51937);
#11076=VERTEX_POINT('',#51938);
#11077=VERTEX_POINT('',#51940);
#11078=VERTEX_POINT('',#51942);
#11079=VERTEX_POINT('',#51946);
#11080=VERTEX_POINT('',#51950);
#11081=VERTEX_POINT('',#51956);
#11082=VERTEX_POINT('',#51957);
#11083=VERTEX_POINT('',#51959);
#11084=VERTEX_POINT('',#51961);
#11085=VERTEX_POINT('',#51965);
#11086=VERTEX_POINT('',#51969);
#11087=VERTEX_POINT('',#51975);
#11088=VERTEX_POINT('',#51976);
#11089=VERTEX_POINT('',#51978);
#11090=VERTEX_POINT('',#51980);
#11091=VERTEX_POINT('',#51984);
#11092=VERTEX_POINT('',#51988);
#11093=VERTEX_POINT('',#51994);
#11094=VERTEX_POINT('',#51995);
#11095=VERTEX_POINT('',#51997);
#11096=VERTEX_POINT('',#51999);
#11097=VERTEX_POINT('',#52003);
#11098=VERTEX_POINT('',#52007);
#11099=VERTEX_POINT('',#52013);
#11100=VERTEX_POINT('',#52014);
#11101=VERTEX_POINT('',#52016);
#11102=VERTEX_POINT('',#52018);
#11103=VERTEX_POINT('',#52022);
#11104=VERTEX_POINT('',#52026);
#11105=VERTEX_POINT('',#52032);
#11106=VERTEX_POINT('',#52033);
#11107=VERTEX_POINT('',#52035);
#11108=VERTEX_POINT('',#52037);
#11109=VERTEX_POINT('',#52041);
#11110=VERTEX_POINT('',#52045);
#11111=VERTEX_POINT('',#52051);
#11112=VERTEX_POINT('',#52052);
#11113=VERTEX_POINT('',#52054);
#11114=VERTEX_POINT('',#52056);
#11115=VERTEX_POINT('',#52060);
#11116=VERTEX_POINT('',#52064);
#11117=VERTEX_POINT('',#52070);
#11118=VERTEX_POINT('',#52071);
#11119=VERTEX_POINT('',#52073);
#11120=VERTEX_POINT('',#52075);
#11121=VERTEX_POINT('',#52079);
#11122=VERTEX_POINT('',#52083);
#11123=VERTEX_POINT('',#52089);
#11124=VERTEX_POINT('',#52090);
#11125=VERTEX_POINT('',#52092);
#11126=VERTEX_POINT('',#52094);
#11127=VERTEX_POINT('',#52098);
#11128=VERTEX_POINT('',#52102);
#11129=VERTEX_POINT('',#52108);
#11130=VERTEX_POINT('',#52109);
#11131=VERTEX_POINT('',#52111);
#11132=VERTEX_POINT('',#52113);
#11133=VERTEX_POINT('',#52117);
#11134=VERTEX_POINT('',#52121);
#11135=VERTEX_POINT('',#52127);
#11136=VERTEX_POINT('',#52128);
#11137=VERTEX_POINT('',#52130);
#11138=VERTEX_POINT('',#52132);
#11139=VERTEX_POINT('',#52136);
#11140=VERTEX_POINT('',#52140);
#11141=VERTEX_POINT('',#52146);
#11142=VERTEX_POINT('',#52147);
#11143=VERTEX_POINT('',#52149);
#11144=VERTEX_POINT('',#52151);
#11145=VERTEX_POINT('',#52155);
#11146=VERTEX_POINT('',#52159);
#11147=VERTEX_POINT('',#52165);
#11148=VERTEX_POINT('',#52166);
#11149=VERTEX_POINT('',#52168);
#11150=VERTEX_POINT('',#52170);
#11151=VERTEX_POINT('',#52174);
#11152=VERTEX_POINT('',#52178);
#11153=VERTEX_POINT('',#52184);
#11154=VERTEX_POINT('',#52185);
#11155=VERTEX_POINT('',#52187);
#11156=VERTEX_POINT('',#52189);
#11157=VERTEX_POINT('',#52193);
#11158=VERTEX_POINT('',#52197);
#11159=VERTEX_POINT('',#52203);
#11160=VERTEX_POINT('',#52204);
#11161=VERTEX_POINT('',#52206);
#11162=VERTEX_POINT('',#52208);
#11163=VERTEX_POINT('',#52212);
#11164=VERTEX_POINT('',#52216);
#11165=VERTEX_POINT('',#52222);
#11166=VERTEX_POINT('',#52223);
#11167=VERTEX_POINT('',#52225);
#11168=VERTEX_POINT('',#52227);
#11169=VERTEX_POINT('',#52231);
#11170=VERTEX_POINT('',#52235);
#11171=VERTEX_POINT('',#52241);
#11172=VERTEX_POINT('',#52242);
#11173=VERTEX_POINT('',#52244);
#11174=VERTEX_POINT('',#52248);
#11175=VERTEX_POINT('',#52250);
#11176=VERTEX_POINT('',#52254);
#11177=VERTEX_POINT('',#52260);
#11178=VERTEX_POINT('',#52261);
#11179=VERTEX_POINT('',#52263);
#11180=VERTEX_POINT('',#52265);
#11181=VERTEX_POINT('',#52269);
#11182=VERTEX_POINT('',#52273);
#11183=VERTEX_POINT('',#52279);
#11184=VERTEX_POINT('',#52280);
#11185=VERTEX_POINT('',#52282);
#11186=VERTEX_POINT('',#52284);
#11187=VERTEX_POINT('',#52288);
#11188=VERTEX_POINT('',#52292);
#11189=VERTEX_POINT('',#52298);
#11190=VERTEX_POINT('',#52299);
#11191=VERTEX_POINT('',#52301);
#11192=VERTEX_POINT('',#52303);
#11193=VERTEX_POINT('',#52307);
#11194=VERTEX_POINT('',#52311);
#11195=VERTEX_POINT('',#52317);
#11196=VERTEX_POINT('',#52318);
#11197=VERTEX_POINT('',#52320);
#11198=VERTEX_POINT('',#52322);
#11199=VERTEX_POINT('',#52326);
#11200=VERTEX_POINT('',#52330);
#11201=VERTEX_POINT('',#52336);
#11202=VERTEX_POINT('',#52337);
#11203=VERTEX_POINT('',#52339);
#11204=VERTEX_POINT('',#52341);
#11205=VERTEX_POINT('',#52345);
#11206=VERTEX_POINT('',#52349);
#11207=VERTEX_POINT('',#52355);
#11208=VERTEX_POINT('',#52356);
#11209=VERTEX_POINT('',#52358);
#11210=VERTEX_POINT('',#52360);
#11211=VERTEX_POINT('',#52364);
#11212=VERTEX_POINT('',#52368);
#11213=VERTEX_POINT('',#52374);
#11214=VERTEX_POINT('',#52375);
#11215=VERTEX_POINT('',#52377);
#11216=VERTEX_POINT('',#52379);
#11217=VERTEX_POINT('',#52383);
#11218=VERTEX_POINT('',#52387);
#11219=VERTEX_POINT('',#52393);
#11220=VERTEX_POINT('',#52394);
#11221=VERTEX_POINT('',#52396);
#11222=VERTEX_POINT('',#52398);
#11223=VERTEX_POINT('',#52402);
#11224=VERTEX_POINT('',#52406);
#11225=VERTEX_POINT('',#52412);
#11226=VERTEX_POINT('',#52413);
#11227=VERTEX_POINT('',#52415);
#11228=VERTEX_POINT('',#52417);
#11229=VERTEX_POINT('',#52421);
#11230=VERTEX_POINT('',#52425);
#11231=VERTEX_POINT('',#52431);
#11232=VERTEX_POINT('',#52436);
#11233=VERTEX_POINT('',#52478);
#11234=VERTEX_POINT('',#52484);
#11235=VERTEX_POINT('',#52485);
#11236=VERTEX_POINT('',#52487);
#11237=VERTEX_POINT('',#52499);
#11238=VERTEX_POINT('',#52512);
#11239=VERTEX_POINT('',#52513);
#11240=VERTEX_POINT('',#52550);
#11241=VERTEX_POINT('',#52551);
#11242=VERTEX_POINT('',#52588);
#11243=VERTEX_POINT('',#52589);
#11244=VERTEX_POINT('',#52625);
#11245=VERTEX_POINT('',#52626);
#11246=VERTEX_POINT('',#52662);
#11247=VERTEX_POINT('',#52663);
#11248=VERTEX_POINT('',#52700);
#11249=VERTEX_POINT('',#52701);
#11250=VERTEX_POINT('',#52738);
#11251=VERTEX_POINT('',#52739);
#11252=VERTEX_POINT('',#52741);
#11253=VERTEX_POINT('',#52777);
#11254=VERTEX_POINT('',#52778);
#11255=VERTEX_POINT('',#52780);
#11256=VERTEX_POINT('',#52797);
#11257=VERTEX_POINT('',#52810);
#11258=VERTEX_POINT('',#52811);
#11259=VERTEX_POINT('',#52894);
#11260=VERTEX_POINT('',#52895);
#11261=VERTEX_POINT('',#52984);
#11262=VERTEX_POINT('',#52985);
#11263=VERTEX_POINT('',#53074);
#11264=VERTEX_POINT('',#53075);
#11265=VERTEX_POINT('',#53158);
#11266=VERTEX_POINT('',#53159);
#11267=VERTEX_POINT('',#53248);
#11268=VERTEX_POINT('',#53249);
#11269=VERTEX_POINT('',#53338);
#11270=VERTEX_POINT('',#53339);
#11271=VERTEX_POINT('',#53422);
#11272=VERTEX_POINT('',#53423);
#11273=VERTEX_POINT('',#53512);
#11274=VERTEX_POINT('',#53513);
#11275=VERTEX_POINT('',#53515);
#11276=VERTEX_POINT('',#53524);
#11277=VERTEX_POINT('',#53532);
#11278=VERTEX_POINT('',#53533);
#11279=VERTEX_POINT('',#53570);
#11280=VERTEX_POINT('',#53571);
#11281=VERTEX_POINT('',#53607);
#11282=VERTEX_POINT('',#53608);
#11283=VERTEX_POINT('',#53644);
#11284=VERTEX_POINT('',#53645);
#11285=VERTEX_POINT('',#53682);
#11286=VERTEX_POINT('',#53683);
#11287=VERTEX_POINT('',#53719);
#11288=VERTEX_POINT('',#53720);
#11289=VERTEX_POINT('',#53756);
#11290=VERTEX_POINT('',#53757);
#11291=VERTEX_POINT('',#53794);
#11292=VERTEX_POINT('',#53795);
#11293=VERTEX_POINT('',#53831);
#11294=VERTEX_POINT('',#53908);
#11295=VERTEX_POINT('',#53910);
#11296=VERTEX_POINT('',#54506);
#11297=VERTEX_POINT('',#54598);
#11298=VERTEX_POINT('',#55707);
#11299=VERTEX_POINT('',#55708);
#11300=VERTEX_POINT('',#55717);
#11301=VERTEX_POINT('',#56010);
#11302=VERTEX_POINT('',#56523);
#11303=VERTEX_POINT('',#56576);
#11304=VERTEX_POINT('',#57238);
#11305=VERTEX_POINT('',#57252);
#11306=VERTEX_POINT('',#57255);
#11307=VERTEX_POINT('',#57264);
#11308=VERTEX_POINT('',#57827);
#11309=VERTEX_POINT('',#58338);
#11310=VERTEX_POINT('',#59004);
#11311=VERTEX_POINT('',#59006);
#11312=VERTEX_POINT('',#59008);
#11313=VERTEX_POINT('',#59012);
#11314=VERTEX_POINT('',#59016);
#11315=VERTEX_POINT('',#59020);
#11316=VERTEX_POINT('',#59024);
#11317=VERTEX_POINT('',#59028);
#11318=VERTEX_POINT('',#59036);
#11319=VERTEX_POINT('',#59038);
#11320=VERTEX_POINT('',#59044);
#11321=VERTEX_POINT('',#59050);
#11322=VERTEX_POINT('',#59056);
#11323=VERTEX_POINT('',#59060);
#11324=VERTEX_POINT('',#59064);
#11325=VERTEX_POINT('',#59067);
#11326=VERTEX_POINT('',#59078);
#11327=VERTEX_POINT('',#59081);
#11328=VERTEX_POINT('',#59084);
#11329=VERTEX_POINT('',#59090);
#11330=VERTEX_POINT('',#59094);
#11331=VERTEX_POINT('',#59098);
#11332=VERTEX_POINT('',#59103);
#11333=VERTEX_POINT('',#59108);
#11334=VERTEX_POINT('',#59112);
#11335=EDGE_CURVE('',#9192,#9192,#8356,.T.);
#11336=EDGE_CURVE('',#9192,#9193,#5490,.T.);
#11337=EDGE_CURVE('',#9193,#9193,#8357,.T.);
#11338=EDGE_CURVE('',#9193,#9194,#5491,.T.);
#11339=EDGE_CURVE('',#9194,#9194,#8358,.T.);
#11340=EDGE_CURVE('',#9195,#9195,#8359,.T.);
#11341=EDGE_CURVE('',#9196,#9196,#8360,.T.);
#11342=EDGE_CURVE('',#9197,#9197,#8361,.T.);
#11343=EDGE_CURVE('',#9198,#9198,#8362,.T.);
#11344=EDGE_CURVE('',#9199,#9199,#8363,.T.);
#11345=EDGE_CURVE('',#9200,#9200,#8364,.T.);
#11346=EDGE_CURVE('',#9201,#9201,#8365,.T.);
#11347=EDGE_CURVE('',#9202,#9202,#8366,.T.);
#11348=EDGE_CURVE('',#9203,#9203,#8367,.T.);
#11349=EDGE_CURVE('',#9204,#9204,#8368,.T.);
#11350=EDGE_CURVE('',#9205,#9205,#8369,.T.);
#11351=EDGE_CURVE('',#9205,#9194,#5492,.T.);
#11352=EDGE_CURVE('',#9206,#9206,#8370,.T.);
#11353=EDGE_CURVE('',#9207,#9207,#8371,.T.);
#11354=EDGE_CURVE('',#9208,#9208,#8372,.T.);
#11355=EDGE_CURVE('',#9209,#9209,#8373,.T.);
#11356=EDGE_CURVE('',#9210,#9210,#8374,.T.);
#11357=EDGE_CURVE('',#9211,#9211,#8375,.T.);
#11358=EDGE_CURVE('',#9212,#9212,#8376,.T.);
#11359=EDGE_CURVE('',#9213,#9213,#8377,.T.);
#11360=EDGE_CURVE('',#9214,#9214,#8378,.T.);
#11361=EDGE_CURVE('',#9215,#9215,#8379,.T.);
#11362=EDGE_CURVE('',#9196,#9216,#5493,.T.);
#11363=EDGE_CURVE('',#9216,#9216,#8380,.T.);
#11364=EDGE_CURVE('',#9216,#9217,#5494,.T.);
#11365=EDGE_CURVE('',#9217,#9217,#8381,.T.);
#11366=EDGE_CURVE('',#9207,#9217,#5495,.T.);
#11367=EDGE_CURVE('',#9204,#9218,#5496,.T.);
#11368=EDGE_CURVE('',#9218,#9218,#8382,.T.);
#11369=EDGE_CURVE('',#9218,#9219,#5497,.T.);
#11370=EDGE_CURVE('',#9219,#9219,#8383,.T.);
#11371=EDGE_CURVE('',#9215,#9219,#5498,.T.);
#11372=EDGE_CURVE('',#9197,#9220,#5499,.T.);
#11373=EDGE_CURVE('',#9220,#9220,#8384,.T.);
#11374=EDGE_CURVE('',#9220,#9221,#5500,.T.);
#11375=EDGE_CURVE('',#9221,#9221,#8385,.T.);
#11376=EDGE_CURVE('',#9208,#9221,#5501,.T.);
#11377=EDGE_CURVE('',#9203,#9222,#5502,.T.);
#11378=EDGE_CURVE('',#9222,#9222,#8386,.T.);
#11379=EDGE_CURVE('',#9222,#9223,#5503,.T.);
#11380=EDGE_CURVE('',#9223,#9223,#8387,.T.);
#11381=EDGE_CURVE('',#9214,#9223,#5504,.T.);
#11382=EDGE_CURVE('',#9198,#9224,#5505,.T.);
#11383=EDGE_CURVE('',#9224,#9224,#8388,.T.);
#11384=EDGE_CURVE('',#9224,#9225,#5506,.T.);
#11385=EDGE_CURVE('',#9225,#9225,#8389,.T.);
#11386=EDGE_CURVE('',#9209,#9225,#5507,.T.);
#11387=EDGE_CURVE('',#9202,#9226,#5508,.T.);
#11388=EDGE_CURVE('',#9226,#9226,#8390,.T.);
#11389=EDGE_CURVE('',#9226,#9227,#5509,.T.);
#11390=EDGE_CURVE('',#9227,#9227,#8391,.T.);
#11391=EDGE_CURVE('',#9213,#9227,#5510,.T.);
#11392=EDGE_CURVE('',#9199,#9228,#5511,.T.);
#11393=EDGE_CURVE('',#9228,#9228,#8392,.T.);
#11394=EDGE_CURVE('',#9228,#9229,#5512,.T.);
#11395=EDGE_CURVE('',#9229,#9229,#8393,.T.);
#11396=EDGE_CURVE('',#9210,#9229,#5513,.T.);
#11397=EDGE_CURVE('',#9201,#9230,#5514,.T.);
#11398=EDGE_CURVE('',#9230,#9230,#8394,.T.);
#11399=EDGE_CURVE('',#9230,#9231,#5515,.T.);
#11400=EDGE_CURVE('',#9231,#9231,#8395,.T.);
#11401=EDGE_CURVE('',#9212,#9231,#5516,.T.);
#11402=EDGE_CURVE('',#9211,#9200,#8396,.T.);
#11403=EDGE_CURVE('',#9232,#9232,#8397,.T.);
#11404=EDGE_CURVE('',#9232,#9195,#5517,.T.);
#11405=EDGE_CURVE('',#9233,#9233,#8398,.T.);
#11406=EDGE_CURVE('',#9233,#9232,#5518,.T.);
#11407=EDGE_CURVE('',#9206,#9233,#5519,.T.);
#11408=EDGE_CURVE('',#9234,#9234,#8399,.T.);
#11409=EDGE_CURVE('',#9234,#9235,#5520,.T.);
#11410=EDGE_CURVE('',#9235,#9235,#8400,.T.);
#11411=EDGE_CURVE('',#9236,#9236,#8401,.T.);
#11412=EDGE_CURVE('',#9237,#9237,#8402,.T.);
#11413=EDGE_CURVE('',#9237,#9236,#5521,.T.);
#11414=EDGE_CURVE('',#9238,#9238,#8403,.T.);
#11415=EDGE_CURVE('',#9238,#9237,#5522,.T.);
#11416=EDGE_CURVE('',#9239,#9239,#8404,.T.);
#11417=EDGE_CURVE('',#9239,#9240,#5523,.T.);
#11418=EDGE_CURVE('',#9240,#9240,#8405,.T.);
#11419=EDGE_CURVE('',#9240,#9241,#5524,.T.);
#11420=EDGE_CURVE('',#9241,#9241,#8406,.T.);
#11421=EDGE_CURVE('',#9241,#9242,#5525,.T.);
#11422=EDGE_CURVE('',#9242,#9242,#8407,.T.);
#11423=EDGE_CURVE('',#9243,#9243,#8408,.T.);
#11424=EDGE_CURVE('',#9235,#9243,#8409,.T.);
#11425=EDGE_CURVE('',#9244,#9245,#1452,.T.);
#11426=EDGE_CURVE('',#9246,#9244,#5526,.T.);
#11427=EDGE_CURVE('',#9246,#9247,#5527,.T.);
#11428=EDGE_CURVE('',#9248,#9247,#5528,.T.);
#11429=EDGE_CURVE('',#9249,#9248,#569,.T.);
#11430=EDGE_CURVE('',#9250,#9249,#5529,.T.);
#11431=EDGE_CURVE('',#9251,#9250,#5530,.T.);
#11432=EDGE_CURVE('',#9252,#9251,#5531,.T.);
#11433=EDGE_CURVE('',#9245,#9252,#5532,.T.);
#11434=EDGE_CURVE('',#9253,#9254,#1453,.T.);
#11435=EDGE_CURVE('',#9255,#9253,#5533,.T.);
#11436=EDGE_CURVE('',#9256,#9255,#5534,.T.);
#11437=EDGE_CURVE('',#9257,#9256,#5535,.T.);
#11438=EDGE_CURVE('',#9258,#9257,#5536,.T.);
#11439=EDGE_CURVE('',#9259,#9258,#570,.T.);
#11440=EDGE_CURVE('',#9260,#9259,#5537,.T.);
#11441=EDGE_CURVE('',#9261,#9260,#5538,.T.);
#11442=EDGE_CURVE('',#9254,#9261,#5539,.T.);
#11443=EDGE_CURVE('',#9247,#9260,#5540,.T.);
#11444=EDGE_CURVE('',#9261,#9246,#5541,.T.);
#11445=EDGE_CURVE('',#9254,#9244,#8410,.T.);
#11446=EDGE_CURVE('',#9262,#9262,#8411,.T.);
#11447=EDGE_CURVE('',#9253,#9245,#8412,.T.);
#11448=EDGE_CURVE('',#9248,#9263,#571,.T.);
#11449=EDGE_CURVE('',#9264,#9263,#5542,.T.);
#11450=EDGE_CURVE('',#9264,#9249,#572,.T.);
#11451=EDGE_CURVE('',#9262,#9265,#5543,.T.);
#11452=EDGE_CURVE('',#9265,#9266,#8413,.T.);
#11453=EDGE_CURVE('',#9266,#9265,#8414,.T.);
#11454=EDGE_CURVE('',#9267,#9267,#573,.T.);
#11455=EDGE_CURVE('',#9267,#9266,#5544,.T.);
#11456=EDGE_CURVE('',#9258,#9264,#574,.T.);
#11457=EDGE_CURVE('',#9263,#9259,#575,.T.);
#11458=EDGE_CURVE('',#9268,#9268,#576,.T.);
#11459=EDGE_CURVE('',#9257,#9250,#8415,.T.);
#11460=EDGE_CURVE('',#9267,#9268,#5545,.T.);
#11461=EDGE_CURVE('',#9255,#9252,#8416,.T.);
#11462=EDGE_CURVE('',#9256,#9251,#8417,.T.);
#11463=EDGE_CURVE('',#9269,#9270,#577,.T.);
#11464=EDGE_CURVE('',#9270,#9269,#5546,.T.);
#11465=EDGE_CURVE('',#9269,#9271,#8418,.T.);
#11466=EDGE_CURVE('',#9271,#9270,#8419,.T.);
#11467=EDGE_CURVE('',#9272,#9273,#578,.T.);
#11468=EDGE_CURVE('',#9274,#9272,#5547,.T.);
#11469=EDGE_CURVE('',#9273,#9274,#579,.T.);
#11470=EDGE_CURVE('',#9274,#9272,#8420,.T.);
#11471=EDGE_CURVE('',#9273,#9271,#580,.T.);
#11472=EDGE_CURVE('',#9275,#9276,#5548,.T.);
#11473=EDGE_CURVE('',#9276,#9277,#5549,.T.);
#11474=EDGE_CURVE('',#9277,#9278,#5550,.T.);
#11475=EDGE_CURVE('',#9278,#9275,#5551,.T.);
#11476=EDGE_CURVE('',#9279,#9280,#5552,.T.);
#11477=EDGE_CURVE('',#9280,#9276,#8421,.T.);
#11478=EDGE_CURVE('',#9275,#9279,#8422,.T.);
#11479=EDGE_CURVE('',#9281,#9282,#5553,.T.);
#11480=EDGE_CURVE('',#9282,#9280,#5554,.T.);
#11481=EDGE_CURVE('',#9279,#9281,#5555,.T.);
#11482=EDGE_CURVE('',#9277,#9282,#8423,.T.);
#11483=EDGE_CURVE('',#9281,#9278,#8424,.T.);
#11484=EDGE_CURVE('',#9283,#9275,#5556,.T.);
#11485=EDGE_CURVE('',#9283,#9284,#8425,.T.);
#11486=EDGE_CURVE('',#9284,#9279,#5557,.T.);
#11487=EDGE_CURVE('',#9285,#9278,#5558,.T.);
#11488=EDGE_CURVE('',#9283,#9285,#5559,.T.);
#11489=EDGE_CURVE('',#9286,#9281,#5560,.T.);
#11490=EDGE_CURVE('',#9286,#9285,#8426,.T.);
#11491=EDGE_CURVE('',#9286,#9284,#5561,.T.);
#11492=EDGE_CURVE('',#9287,#9287,#8427,.T.);
#11493=EDGE_CURVE('',#9287,#9288,#5562,.T.);
#11494=EDGE_CURVE('',#9288,#9288,#8428,.T.);
#11495=EDGE_CURVE('',#9289,#9289,#8429,.T.);
#11496=EDGE_CURVE('',#9289,#9290,#5563,.T.);
#11497=EDGE_CURVE('',#9290,#9290,#8430,.T.);
#11498=EDGE_CURVE('',#9291,#9291,#8431,.T.);
#11499=EDGE_CURVE('',#9292,#9292,#8432,.T.);
#11500=EDGE_CURVE('',#9292,#9293,#5564,.T.);
#11501=EDGE_CURVE('',#9293,#9294,#8433,.T.);
#11502=EDGE_CURVE('',#9294,#9293,#8434,.T.);
#11503=EDGE_CURVE('',#9294,#9295,#5565,.T.);
#11504=EDGE_CURVE('',#9296,#9295,#8435,.T.);
#11505=EDGE_CURVE('',#9295,#9296,#8436,.T.);
#11506=EDGE_CURVE('',#9296,#9297,#5566,.T.);
#11507=EDGE_CURVE('',#9297,#9297,#8437,.T.);
#11508=EDGE_CURVE('',#9298,#9298,#8438,.T.);
#11509=EDGE_CURVE('',#9299,#9299,#8439,.T.);
#11510=EDGE_CURVE('',#9299,#9298,#5567,.T.);
#11511=EDGE_CURVE('',#9291,#9300,#5568,.T.);
#11512=EDGE_CURVE('',#9300,#9300,#8440,.T.);
#11513=EDGE_CURVE('',#9300,#9301,#5569,.T.);
#11514=EDGE_CURVE('',#9301,#9301,#8441,.T.);
#11515=EDGE_CURVE('',#9301,#9302,#5570,.T.);
#11516=EDGE_CURVE('',#9302,#9302,#8442,.T.);
#11517=EDGE_CURVE('',#9302,#9303,#5571,.T.);
#11518=EDGE_CURVE('',#9303,#9303,#8443,.T.);
#11519=EDGE_CURVE('',#9303,#9304,#5572,.T.);
#11520=EDGE_CURVE('',#9304,#9304,#8444,.T.);
#11521=EDGE_CURVE('',#9304,#9305,#5573,.T.);
#11522=EDGE_CURVE('',#9305,#9305,#8445,.T.);
#11523=EDGE_CURVE('',#9306,#9307,#5574,.T.);
#11524=EDGE_CURVE('',#9306,#9308,#581,.T.);
#11525=EDGE_CURVE('',#9309,#9308,#8446,.T.);
#11526=EDGE_CURVE('',#9307,#9309,#582,.T.);
#11527=EDGE_CURVE('',#9310,#9311,#5575,.T.);
#11528=EDGE_CURVE('',#9310,#9306,#583,.T.);
#11529=EDGE_CURVE('',#9311,#9307,#584,.T.);
#11530=EDGE_CURVE('',#9312,#9313,#5576,.T.);
#11531=EDGE_CURVE('',#9312,#9310,#585,.T.);
#11532=EDGE_CURVE('',#9313,#9311,#586,.T.);
#11533=EDGE_CURVE('',#9314,#9315,#5577,.T.);
#11534=EDGE_CURVE('',#9314,#9312,#587,.T.);
#11535=EDGE_CURVE('',#9315,#9313,#588,.T.);
#11536=EDGE_CURVE('',#9316,#9317,#5578,.T.);
#11537=EDGE_CURVE('',#9316,#9314,#589,.T.);
#11538=EDGE_CURVE('',#9317,#9315,#590,.T.);
#11539=EDGE_CURVE('',#9318,#9319,#5579,.T.);
#11540=EDGE_CURVE('',#9318,#9316,#591,.T.);
#11541=EDGE_CURVE('',#9319,#9317,#592,.T.);
#11542=EDGE_CURVE('',#9320,#9321,#5580,.T.);
#11543=EDGE_CURVE('',#9320,#9318,#593,.T.);
#11544=EDGE_CURVE('',#9321,#9319,#594,.T.);
#11545=EDGE_CURVE('',#9322,#9323,#5581,.T.);
#11546=EDGE_CURVE('',#9324,#9322,#8447,.T.);
#11547=EDGE_CURVE('',#9324,#9320,#595,.T.);
#11548=EDGE_CURVE('',#9323,#9321,#596,.T.);
#11549=EDGE_CURVE('',#9325,#9326,#597,.T.);
#11550=EDGE_CURVE('',#9327,#9325,#598,.T.);
#11551=EDGE_CURVE('',#9328,#9327,#599,.T.);
#11552=EDGE_CURVE('',#9328,#9326,#600,.T.);
#11553=EDGE_CURVE('',#9326,#9329,#601,.T.);
#11554=EDGE_CURVE('',#9330,#9328,#602,.T.);
#11555=EDGE_CURVE('',#9330,#9329,#603,.T.);
#11556=EDGE_CURVE('',#9329,#9309,#604,.T.);
#11557=EDGE_CURVE('',#9331,#9330,#605,.T.);
#11558=EDGE_CURVE('',#9331,#9323,#606,.T.);
#11559=EDGE_CURVE('',#9327,#9332,#8448,.T.);
#11560=EDGE_CURVE('',#9332,#9327,#8449,.T.);
#11561=EDGE_CURVE('',#9327,#9333,#607,.T.);
#11562=EDGE_CURVE('',#9333,#9334,#608,.T.);
#11563=EDGE_CURVE('',#9334,#9324,#609,.T.);
#11564=EDGE_CURVE('',#9322,#9331,#8450,.T.);
#11565=EDGE_CURVE('',#9308,#9335,#610,.T.);
#11566=EDGE_CURVE('',#9334,#9335,#611,.T.);
#11567=EDGE_CURVE('',#9335,#9336,#612,.T.);
#11568=EDGE_CURVE('',#9333,#9336,#613,.T.);
#11569=EDGE_CURVE('',#9336,#9325,#614,.T.);
#11570=EDGE_CURVE('',#9337,#9338,#5582,.T.);
#11571=EDGE_CURVE('',#9337,#9339,#5583,.T.);
#11572=EDGE_CURVE('',#9339,#9340,#5584,.T.);
#11573=EDGE_CURVE('',#9338,#9340,#5585,.T.);
#11574=EDGE_CURVE('',#9341,#9337,#5586,.T.);
#11575=EDGE_CURVE('',#9341,#9342,#5587,.T.);
#11576=EDGE_CURVE('',#9342,#9339,#5588,.T.);
#11577=EDGE_CURVE('',#9343,#9341,#5589,.T.);
#11578=EDGE_CURVE('',#9343,#9344,#5590,.T.);
#11579=EDGE_CURVE('',#9344,#9342,#5591,.T.);
#11580=EDGE_CURVE('',#9345,#9343,#5592,.T.);
#11581=EDGE_CURVE('',#9345,#9346,#5593,.T.);
#11582=EDGE_CURVE('',#9346,#9344,#5594,.T.);
#11583=EDGE_CURVE('',#9347,#9345,#5595,.T.);
#11584=EDGE_CURVE('',#9347,#9348,#5596,.T.);
#11585=EDGE_CURVE('',#9348,#9346,#5597,.T.);
#11586=EDGE_CURVE('',#9338,#9347,#5598,.T.);
#11587=EDGE_CURVE('',#9340,#9348,#5599,.T.);
#11588=EDGE_CURVE('',#9349,#9350,#5600,.T.);
#11589=EDGE_CURVE('',#9349,#9351,#5601,.T.);
#11590=EDGE_CURVE('',#9352,#9351,#5602,.T.);
#11591=EDGE_CURVE('',#9350,#9352,#5603,.T.);
#11592=EDGE_CURVE('',#9350,#9353,#8451,.T.);
#11593=EDGE_CURVE('',#9352,#9353,#5604,.T.);
#11594=EDGE_CURVE('',#9353,#9354,#5605,.T.);
#11595=EDGE_CURVE('',#9351,#9354,#5606,.T.);
#11596=EDGE_CURVE('',#9354,#9349,#8452,.T.);
#11597=EDGE_CURVE('',#9355,#9356,#5607,.T.);
#11598=EDGE_CURVE('',#9355,#9357,#5608,.T.);
#11599=EDGE_CURVE('',#9358,#9357,#5609,.T.);
#11600=EDGE_CURVE('',#9356,#9358,#5610,.T.);
#11601=EDGE_CURVE('',#9356,#9359,#8453,.T.);
#11602=EDGE_CURVE('',#9358,#9359,#5611,.T.);
#11603=EDGE_CURVE('',#9359,#9360,#5612,.T.);
#11604=EDGE_CURVE('',#9357,#9360,#5613,.T.);
#11605=EDGE_CURVE('',#9360,#9355,#8454,.T.);
#11606=EDGE_CURVE('',#9361,#9362,#5614,.T.);
#11607=EDGE_CURVE('',#9361,#9363,#5615,.T.);
#11608=EDGE_CURVE('',#9364,#9363,#5616,.T.);
#11609=EDGE_CURVE('',#9362,#9364,#5617,.T.);
#11610=EDGE_CURVE('',#9362,#9365,#8455,.T.);
#11611=EDGE_CURVE('',#9364,#9365,#5618,.T.);
#11612=EDGE_CURVE('',#9365,#9366,#5619,.T.);
#11613=EDGE_CURVE('',#9363,#9366,#5620,.T.);
#11614=EDGE_CURVE('',#9366,#9361,#8456,.T.);
#11615=EDGE_CURVE('',#9367,#9368,#5621,.T.);
#11616=EDGE_CURVE('',#9367,#9369,#5622,.T.);
#11617=EDGE_CURVE('',#9370,#9369,#5623,.T.);
#11618=EDGE_CURVE('',#9368,#9370,#5624,.T.);
#11619=EDGE_CURVE('',#9368,#9371,#8457,.T.);
#11620=EDGE_CURVE('',#9370,#9371,#5625,.T.);
#11621=EDGE_CURVE('',#9371,#9372,#5626,.T.);
#11622=EDGE_CURVE('',#9369,#9372,#5627,.T.);
#11623=EDGE_CURVE('',#9372,#9367,#8458,.T.);
#11624=EDGE_CURVE('',#9373,#9374,#5628,.T.);
#11625=EDGE_CURVE('',#9373,#9375,#5629,.T.);
#11626=EDGE_CURVE('',#9376,#9375,#5630,.T.);
#11627=EDGE_CURVE('',#9374,#9376,#5631,.T.);
#11628=EDGE_CURVE('',#9374,#9377,#8459,.T.);
#11629=EDGE_CURVE('',#9376,#9377,#5632,.T.);
#11630=EDGE_CURVE('',#9377,#9378,#5633,.T.);
#11631=EDGE_CURVE('',#9375,#9378,#5634,.T.);
#11632=EDGE_CURVE('',#9378,#9373,#8460,.T.);
#11633=EDGE_CURVE('',#9379,#9380,#5635,.T.);
#11634=EDGE_CURVE('',#9379,#9381,#5636,.T.);
#11635=EDGE_CURVE('',#9382,#9381,#5637,.T.);
#11636=EDGE_CURVE('',#9380,#9382,#5638,.T.);
#11637=EDGE_CURVE('',#9380,#9383,#8461,.T.);
#11638=EDGE_CURVE('',#9382,#9383,#5639,.T.);
#11639=EDGE_CURVE('',#9383,#9384,#5640,.T.);
#11640=EDGE_CURVE('',#9381,#9384,#5641,.T.);
#11641=EDGE_CURVE('',#9384,#9379,#8462,.T.);
#11642=EDGE_CURVE('',#9385,#9386,#5642,.T.);
#11643=EDGE_CURVE('',#9385,#9387,#5643,.T.);
#11644=EDGE_CURVE('',#9388,#9387,#5644,.T.);
#11645=EDGE_CURVE('',#9386,#9388,#5645,.T.);
#11646=EDGE_CURVE('',#9386,#9389,#8463,.T.);
#11647=EDGE_CURVE('',#9388,#9389,#5646,.T.);
#11648=EDGE_CURVE('',#9389,#9390,#5647,.T.);
#11649=EDGE_CURVE('',#9387,#9390,#5648,.T.);
#11650=EDGE_CURVE('',#9390,#9385,#8464,.T.);
#11651=EDGE_CURVE('',#9391,#9392,#8465,.T.);
#11652=EDGE_CURVE('',#9391,#9393,#5649,.T.);
#11653=EDGE_CURVE('',#9393,#9392,#5650,.T.);
#11654=EDGE_CURVE('',#9394,#9391,#5651,.T.);
#11655=EDGE_CURVE('',#9394,#9395,#5652,.T.);
#11656=EDGE_CURVE('',#9393,#9395,#5653,.T.);
#11657=EDGE_CURVE('',#9392,#9396,#5654,.T.);
#11658=EDGE_CURVE('',#9395,#9396,#5655,.T.);
#11659=EDGE_CURVE('',#9396,#9394,#8466,.T.);
#11660=EDGE_CURVE('',#9397,#9398,#5656,.T.);
#11661=EDGE_CURVE('',#9397,#9399,#5657,.T.);
#11662=EDGE_CURVE('',#9400,#9399,#5658,.T.);
#11663=EDGE_CURVE('',#9398,#9400,#5659,.T.);
#11664=EDGE_CURVE('',#9398,#9401,#8467,.T.);
#11665=EDGE_CURVE('',#9400,#9401,#5660,.T.);
#11666=EDGE_CURVE('',#9401,#9402,#5661,.T.);
#11667=EDGE_CURVE('',#9399,#9402,#5662,.T.);
#11668=EDGE_CURVE('',#9402,#9397,#8468,.T.);
#11669=EDGE_CURVE('',#9403,#9404,#5663,.T.);
#11670=EDGE_CURVE('',#9403,#9405,#5664,.T.);
#11671=EDGE_CURVE('',#9406,#9405,#5665,.T.);
#11672=EDGE_CURVE('',#9404,#9406,#5666,.T.);
#11673=EDGE_CURVE('',#9404,#9407,#8469,.T.);
#11674=EDGE_CURVE('',#9406,#9407,#5667,.T.);
#11675=EDGE_CURVE('',#9407,#9408,#5668,.T.);
#11676=EDGE_CURVE('',#9405,#9408,#5669,.T.);
#11677=EDGE_CURVE('',#9408,#9403,#8470,.T.);
#11678=EDGE_CURVE('',#9409,#9410,#5670,.T.);
#11679=EDGE_CURVE('',#9409,#9411,#5671,.T.);
#11680=EDGE_CURVE('',#9412,#9411,#5672,.T.);
#11681=EDGE_CURVE('',#9410,#9412,#5673,.T.);
#11682=EDGE_CURVE('',#9410,#9413,#8471,.T.);
#11683=EDGE_CURVE('',#9412,#9413,#5674,.T.);
#11684=EDGE_CURVE('',#9413,#9414,#5675,.T.);
#11685=EDGE_CURVE('',#9411,#9414,#5676,.T.);
#11686=EDGE_CURVE('',#9414,#9409,#8472,.T.);
#11687=EDGE_CURVE('',#9415,#9416,#5677,.T.);
#11688=EDGE_CURVE('',#9415,#9417,#5678,.T.);
#11689=EDGE_CURVE('',#9418,#9417,#5679,.T.);
#11690=EDGE_CURVE('',#9416,#9418,#5680,.T.);
#11691=EDGE_CURVE('',#9416,#9419,#8473,.T.);
#11692=EDGE_CURVE('',#9418,#9419,#5681,.T.);
#11693=EDGE_CURVE('',#9419,#9420,#5682,.T.);
#11694=EDGE_CURVE('',#9417,#9420,#5683,.T.);
#11695=EDGE_CURVE('',#9420,#9415,#8474,.T.);
#11696=EDGE_CURVE('',#9421,#9422,#5684,.T.);
#11697=EDGE_CURVE('',#9421,#9423,#5685,.T.);
#11698=EDGE_CURVE('',#9424,#9423,#5686,.T.);
#11699=EDGE_CURVE('',#9422,#9424,#5687,.T.);
#11700=EDGE_CURVE('',#9422,#9425,#8475,.T.);
#11701=EDGE_CURVE('',#9424,#9425,#5688,.T.);
#11702=EDGE_CURVE('',#9425,#9426,#5689,.T.);
#11703=EDGE_CURVE('',#9423,#9426,#5690,.T.);
#11704=EDGE_CURVE('',#9426,#9421,#8476,.T.);
#11705=EDGE_CURVE('',#9427,#9428,#5691,.T.);
#11706=EDGE_CURVE('',#9427,#9429,#5692,.T.);
#11707=EDGE_CURVE('',#9430,#9429,#5693,.T.);
#11708=EDGE_CURVE('',#9428,#9430,#5694,.T.);
#11709=EDGE_CURVE('',#9428,#9431,#8477,.T.);
#11710=EDGE_CURVE('',#9430,#9431,#5695,.T.);
#11711=EDGE_CURVE('',#9431,#9432,#5696,.T.);
#11712=EDGE_CURVE('',#9429,#9432,#5697,.T.);
#11713=EDGE_CURVE('',#9432,#9427,#8478,.T.);
#11714=EDGE_CURVE('',#9433,#9434,#5698,.T.);
#11715=EDGE_CURVE('',#9433,#9435,#5699,.T.);
#11716=EDGE_CURVE('',#9436,#9435,#5700,.T.);
#11717=EDGE_CURVE('',#9434,#9436,#5701,.T.);
#11718=EDGE_CURVE('',#9434,#9437,#8479,.T.);
#11719=EDGE_CURVE('',#9436,#9437,#5702,.T.);
#11720=EDGE_CURVE('',#9437,#9438,#5703,.T.);
#11721=EDGE_CURVE('',#9435,#9438,#5704,.T.);
#11722=EDGE_CURVE('',#9438,#9433,#8480,.T.);
#11723=EDGE_CURVE('',#9439,#9440,#5705,.T.);
#11724=EDGE_CURVE('',#9439,#9441,#5706,.T.);
#11725=EDGE_CURVE('',#9442,#9441,#5707,.T.);
#11726=EDGE_CURVE('',#9440,#9442,#5708,.T.);
#11727=EDGE_CURVE('',#9440,#9443,#8481,.T.);
#11728=EDGE_CURVE('',#9442,#9443,#5709,.T.);
#11729=EDGE_CURVE('',#9443,#9444,#5710,.T.);
#11730=EDGE_CURVE('',#9441,#9444,#5711,.T.);
#11731=EDGE_CURVE('',#9444,#9439,#8482,.T.);
#11732=EDGE_CURVE('',#9445,#9446,#5712,.T.);
#11733=EDGE_CURVE('',#9445,#9447,#5713,.T.);
#11734=EDGE_CURVE('',#9448,#9447,#5714,.T.);
#11735=EDGE_CURVE('',#9446,#9448,#5715,.T.);
#11736=EDGE_CURVE('',#9446,#9449,#8483,.T.);
#11737=EDGE_CURVE('',#9448,#9449,#5716,.T.);
#11738=EDGE_CURVE('',#9449,#9450,#5717,.T.);
#11739=EDGE_CURVE('',#9447,#9450,#5718,.T.);
#11740=EDGE_CURVE('',#9450,#9445,#8484,.T.);
#11741=EDGE_CURVE('',#9451,#9452,#5719,.T.);
#11742=EDGE_CURVE('',#9451,#9453,#5720,.T.);
#11743=EDGE_CURVE('',#9454,#9453,#5721,.T.);
#11744=EDGE_CURVE('',#9452,#9454,#5722,.T.);
#11745=EDGE_CURVE('',#9452,#9455,#8485,.T.);
#11746=EDGE_CURVE('',#9454,#9455,#5723,.T.);
#11747=EDGE_CURVE('',#9455,#9456,#5724,.T.);
#11748=EDGE_CURVE('',#9453,#9456,#5725,.T.);
#11749=EDGE_CURVE('',#9456,#9451,#8486,.T.);
#11750=EDGE_CURVE('',#9457,#9458,#5726,.T.);
#11751=EDGE_CURVE('',#9457,#9459,#5727,.T.);
#11752=EDGE_CURVE('',#9460,#9459,#5728,.T.);
#11753=EDGE_CURVE('',#9458,#9460,#5729,.T.);
#11754=EDGE_CURVE('',#9458,#9461,#8487,.T.);
#11755=EDGE_CURVE('',#9460,#9461,#5730,.T.);
#11756=EDGE_CURVE('',#9461,#9462,#5731,.T.);
#11757=EDGE_CURVE('',#9459,#9462,#5732,.T.);
#11758=EDGE_CURVE('',#9462,#9457,#8488,.T.);
#11759=EDGE_CURVE('',#9463,#9464,#5733,.T.);
#11760=EDGE_CURVE('',#9463,#9465,#5734,.T.);
#11761=EDGE_CURVE('',#9466,#9465,#5735,.T.);
#11762=EDGE_CURVE('',#9464,#9466,#5736,.T.);
#11763=EDGE_CURVE('',#9464,#9467,#8489,.T.);
#11764=EDGE_CURVE('',#9466,#9467,#5737,.T.);
#11765=EDGE_CURVE('',#9467,#9468,#5738,.T.);
#11766=EDGE_CURVE('',#9465,#9468,#5739,.T.);
#11767=EDGE_CURVE('',#9468,#9463,#8490,.T.);
#11768=EDGE_CURVE('',#9469,#9470,#5740,.T.);
#11769=EDGE_CURVE('',#9469,#9471,#5741,.T.);
#11770=EDGE_CURVE('',#9472,#9471,#5742,.T.);
#11771=EDGE_CURVE('',#9470,#9472,#5743,.T.);
#11772=EDGE_CURVE('',#9470,#9473,#8491,.T.);
#11773=EDGE_CURVE('',#9472,#9473,#5744,.T.);
#11774=EDGE_CURVE('',#9473,#9474,#5745,.T.);
#11775=EDGE_CURVE('',#9471,#9474,#5746,.T.);
#11776=EDGE_CURVE('',#9474,#9469,#8492,.T.);
#11777=EDGE_CURVE('',#9475,#9476,#5747,.T.);
#11778=EDGE_CURVE('',#9475,#9477,#5748,.T.);
#11779=EDGE_CURVE('',#9478,#9477,#5749,.T.);
#11780=EDGE_CURVE('',#9476,#9478,#5750,.T.);
#11781=EDGE_CURVE('',#9476,#9479,#8493,.T.);
#11782=EDGE_CURVE('',#9478,#9479,#5751,.T.);
#11783=EDGE_CURVE('',#9479,#9480,#5752,.T.);
#11784=EDGE_CURVE('',#9477,#9480,#5753,.T.);
#11785=EDGE_CURVE('',#9480,#9475,#8494,.T.);
#11786=EDGE_CURVE('',#9481,#9482,#5754,.T.);
#11787=EDGE_CURVE('',#9481,#9483,#5755,.T.);
#11788=EDGE_CURVE('',#9484,#9483,#5756,.T.);
#11789=EDGE_CURVE('',#9482,#9484,#5757,.T.);
#11790=EDGE_CURVE('',#9482,#9485,#8495,.T.);
#11791=EDGE_CURVE('',#9484,#9486,#5758,.T.);
#11792=EDGE_CURVE('',#9485,#9486,#8496,.T.);
#11793=EDGE_CURVE('',#9486,#9487,#5759,.T.);
#11794=EDGE_CURVE('',#9483,#9487,#5760,.T.);
#11795=EDGE_CURVE('',#9487,#9488,#8497,.T.);
#11796=EDGE_CURVE('',#9488,#9481,#8498,.T.);
#11797=EDGE_CURVE('',#9489,#9490,#5761,.T.);
#11798=EDGE_CURVE('',#9489,#9491,#5762,.T.);
#11799=EDGE_CURVE('',#9492,#9491,#5763,.T.);
#11800=EDGE_CURVE('',#9490,#9492,#5764,.T.);
#11801=EDGE_CURVE('',#9490,#9493,#8499,.T.);
#11802=EDGE_CURVE('',#9492,#9493,#5765,.T.);
#11803=EDGE_CURVE('',#9493,#9494,#5766,.T.);
#11804=EDGE_CURVE('',#9491,#9494,#5767,.T.);
#11805=EDGE_CURVE('',#9494,#9489,#8500,.T.);
#11806=EDGE_CURVE('',#9495,#9496,#5768,.T.);
#11807=EDGE_CURVE('',#9495,#9497,#5769,.T.);
#11808=EDGE_CURVE('',#9498,#9497,#5770,.T.);
#11809=EDGE_CURVE('',#9496,#9498,#5771,.T.);
#11810=EDGE_CURVE('',#9496,#9499,#8501,.T.);
#11811=EDGE_CURVE('',#9498,#9499,#5772,.T.);
#11812=EDGE_CURVE('',#9499,#9500,#5773,.T.);
#11813=EDGE_CURVE('',#9497,#9500,#5774,.T.);
#11814=EDGE_CURVE('',#9500,#9495,#8502,.T.);
#11815=EDGE_CURVE('',#9501,#9502,#5775,.T.);
#11816=EDGE_CURVE('',#9501,#9503,#5776,.T.);
#11817=EDGE_CURVE('',#9504,#9503,#5777,.T.);
#11818=EDGE_CURVE('',#9502,#9504,#5778,.T.);
#11819=EDGE_CURVE('',#9502,#9505,#8503,.T.);
#11820=EDGE_CURVE('',#9504,#9505,#5779,.T.);
#11821=EDGE_CURVE('',#9505,#9506,#5780,.T.);
#11822=EDGE_CURVE('',#9503,#9506,#5781,.T.);
#11823=EDGE_CURVE('',#9506,#9501,#8504,.T.);
#11824=EDGE_CURVE('',#9507,#9508,#5782,.T.);
#11825=EDGE_CURVE('',#9507,#9509,#5783,.T.);
#11826=EDGE_CURVE('',#9510,#9509,#5784,.T.);
#11827=EDGE_CURVE('',#9508,#9510,#5785,.T.);
#11828=EDGE_CURVE('',#9508,#9511,#8505,.T.);
#11829=EDGE_CURVE('',#9510,#9511,#5786,.T.);
#11830=EDGE_CURVE('',#9511,#9512,#5787,.T.);
#11831=EDGE_CURVE('',#9509,#9512,#5788,.T.);
#11832=EDGE_CURVE('',#9512,#9507,#8506,.T.);
#11833=EDGE_CURVE('',#9513,#9514,#5789,.T.);
#11834=EDGE_CURVE('',#9513,#9515,#5790,.T.);
#11835=EDGE_CURVE('',#9516,#9515,#5791,.T.);
#11836=EDGE_CURVE('',#9514,#9516,#5792,.T.);
#11837=EDGE_CURVE('',#9514,#9517,#8507,.T.);
#11838=EDGE_CURVE('',#9516,#9517,#5793,.T.);
#11839=EDGE_CURVE('',#9517,#9518,#5794,.T.);
#11840=EDGE_CURVE('',#9515,#9518,#5795,.T.);
#11841=EDGE_CURVE('',#9518,#9513,#8508,.T.);
#11842=EDGE_CURVE('',#9519,#9520,#5796,.T.);
#11843=EDGE_CURVE('',#9519,#9521,#5797,.T.);
#11844=EDGE_CURVE('',#9522,#9521,#5798,.T.);
#11845=EDGE_CURVE('',#9520,#9522,#5799,.T.);
#11846=EDGE_CURVE('',#9520,#9523,#8509,.T.);
#11847=EDGE_CURVE('',#9522,#9523,#5800,.T.);
#11848=EDGE_CURVE('',#9523,#9524,#5801,.T.);
#11849=EDGE_CURVE('',#9521,#9524,#5802,.T.);
#11850=EDGE_CURVE('',#9524,#9519,#8510,.T.);
#11851=EDGE_CURVE('',#9525,#9526,#5803,.T.);
#11852=EDGE_CURVE('',#9525,#9527,#5804,.T.);
#11853=EDGE_CURVE('',#9528,#9527,#5805,.T.);
#11854=EDGE_CURVE('',#9526,#9528,#5806,.T.);
#11855=EDGE_CURVE('',#9526,#9529,#8511,.T.);
#11856=EDGE_CURVE('',#9528,#9529,#5807,.T.);
#11857=EDGE_CURVE('',#9529,#9530,#5808,.T.);
#11858=EDGE_CURVE('',#9527,#9530,#5809,.T.);
#11859=EDGE_CURVE('',#9530,#9525,#8512,.T.);
#11860=EDGE_CURVE('',#9531,#9531,#8513,.T.);
#11861=EDGE_CURVE('',#9531,#9532,#5810,.T.);
#11862=EDGE_CURVE('',#9533,#9532,#1454,.T.);
#11863=EDGE_CURVE('',#9534,#9533,#1455,.T.);
#11864=EDGE_CURVE('',#9535,#9534,#1456,.T.);
#11865=EDGE_CURVE('',#9536,#9535,#1457,.T.);
#11866=EDGE_CURVE('',#9537,#9536,#1458,.T.);
#11867=EDGE_CURVE('',#9538,#9537,#1459,.T.);
#11868=EDGE_CURVE('',#9532,#9538,#1460,.T.);
#11869=EDGE_CURVE('',#9536,#9539,#5811,.T.);
#11870=EDGE_CURVE('',#9539,#9540,#1461,.T.);
#11871=EDGE_CURVE('',#9537,#9540,#5812,.T.);
#11872=EDGE_CURVE('',#9535,#9541,#5813,.T.);
#11873=EDGE_CURVE('',#9541,#9539,#1462,.T.);
#11874=EDGE_CURVE('',#9534,#9542,#5814,.T.);
#11875=EDGE_CURVE('',#9542,#9541,#1463,.T.);
#11876=EDGE_CURVE('',#9543,#9542,#1464,.T.);
#11877=EDGE_CURVE('',#9544,#9543,#1465,.T.);
#11878=EDGE_CURVE('',#9544,#9545,#5815,.T.);
#11879=EDGE_CURVE('',#9545,#9545,#8514,.T.);
#11880=EDGE_CURVE('',#9546,#9544,#1466,.T.);
#11881=EDGE_CURVE('',#9540,#9546,#1467,.T.);
#11882=EDGE_CURVE('',#9533,#9543,#5816,.T.);
#11883=EDGE_CURVE('',#9547,#9547,#8515,.T.);
#11884=EDGE_CURVE('',#9548,#9548,#8516,.T.);
#11885=EDGE_CURVE('',#9538,#9546,#5817,.T.);
#11886=EDGE_CURVE('',#9549,#9549,#8517,.T.);
#11887=EDGE_CURVE('',#9549,#9550,#5818,.T.);
#11888=EDGE_CURVE('',#9550,#9550,#8518,.T.);
#11889=EDGE_CURVE('',#9550,#9551,#5819,.T.);
#11890=EDGE_CURVE('',#9552,#9552,#8519,.T.);
#11891=EDGE_CURVE('',#9332,#9552,#5820,.T.);
#11892=EDGE_CURVE('',#9553,#9553,#8520,.T.);
#11893=EDGE_CURVE('',#9548,#9553,#5821,.T.);
#11894=EDGE_CURVE('',#9523,#9350,#8521,.T.);
#11895=EDGE_CURVE('',#9359,#9520,#8522,.T.);
#11896=EDGE_CURVE('',#9517,#9356,#8523,.T.);
#11897=EDGE_CURVE('',#9365,#9514,#8524,.T.);
#11898=EDGE_CURVE('',#9511,#9362,#8525,.T.);
#11899=EDGE_CURVE('',#9371,#9508,#8526,.T.);
#11900=EDGE_CURVE('',#9505,#9368,#8527,.T.);
#11901=EDGE_CURVE('',#9377,#9502,#8528,.T.);
#11902=EDGE_CURVE('',#9499,#9374,#8529,.T.);
#11903=EDGE_CURVE('',#9383,#9496,#8530,.T.);
#11904=EDGE_CURVE('',#9493,#9380,#8531,.T.);
#11905=EDGE_CURVE('',#9389,#9490,#8532,.T.);
#11906=EDGE_CURVE('',#9486,#9386,#8533,.T.);
#11907=EDGE_CURVE('',#9488,#9547,#5822,.T.);
#11908=EDGE_CURVE('',#9479,#9482,#8534,.T.);
#11909=EDGE_CURVE('',#9401,#9476,#8535,.T.);
#11910=EDGE_CURVE('',#9473,#9398,#8536,.T.);
#11911=EDGE_CURVE('',#9407,#9470,#8537,.T.);
#11912=EDGE_CURVE('',#9467,#9404,#8538,.T.);
#11913=EDGE_CURVE('',#9413,#9464,#8539,.T.);
#11914=EDGE_CURVE('',#9461,#9410,#8540,.T.);
#11915=EDGE_CURVE('',#9419,#9458,#8541,.T.);
#11916=EDGE_CURVE('',#9455,#9416,#8542,.T.);
#11917=EDGE_CURVE('',#9425,#9452,#8543,.T.);
#11918=EDGE_CURVE('',#9449,#9422,#8544,.T.);
#11919=EDGE_CURVE('',#9431,#9446,#8545,.T.);
#11920=EDGE_CURVE('',#9443,#9428,#8546,.T.);
#11921=EDGE_CURVE('',#9437,#9440,#8547,.T.);
#11922=EDGE_CURVE('',#9392,#9434,#8548,.T.);
#11923=EDGE_CURVE('',#9529,#9391,#8549,.T.);
#11924=EDGE_CURVE('',#9353,#9526,#8550,.T.);
#11925=EDGE_CURVE('',#9554,#9554,#8551,.T.);
#11926=EDGE_CURVE('',#9554,#9485,#5823,.T.);
#11927=EDGE_CURVE('',#9555,#9556,#5824,.T.);
#11928=EDGE_CURVE('',#9555,#9557,#615,.T.);
#11929=EDGE_CURVE('',#9558,#9557,#8552,.T.);
#11930=EDGE_CURVE('',#9556,#9558,#616,.T.);
#11931=EDGE_CURVE('',#9559,#9560,#5825,.T.);
#11932=EDGE_CURVE('',#9559,#9555,#617,.T.);
#11933=EDGE_CURVE('',#9560,#9556,#618,.T.);
#11934=EDGE_CURVE('',#9561,#9562,#5826,.T.);
#11935=EDGE_CURVE('',#9561,#9559,#619,.T.);
#11936=EDGE_CURVE('',#9562,#9560,#620,.T.);
#11937=EDGE_CURVE('',#9563,#9564,#5827,.T.);
#11938=EDGE_CURVE('',#9563,#9561,#621,.T.);
#11939=EDGE_CURVE('',#9564,#9562,#622,.T.);
#11940=EDGE_CURVE('',#9565,#9566,#5828,.T.);
#11941=EDGE_CURVE('',#9567,#9565,#8553,.T.);
#11942=EDGE_CURVE('',#9567,#9563,#623,.T.);
#11943=EDGE_CURVE('',#9566,#9564,#624,.T.);
#11944=EDGE_CURVE('',#9568,#9569,#5829,.T.);
#11945=EDGE_CURVE('',#9568,#9570,#625,.T.);
#11946=EDGE_CURVE('',#9570,#9571,#8554,.F.);
#11947=EDGE_CURVE('',#9571,#9569,#626,.T.);
#11948=EDGE_CURVE('',#9572,#9573,#5830,.T.);
#11949=EDGE_CURVE('',#9572,#9568,#627,.T.);
#11950=EDGE_CURVE('',#9569,#9573,#628,.T.);
#11951=EDGE_CURVE('',#9574,#9575,#5831,.T.);
#11952=EDGE_CURVE('',#9574,#9572,#629,.T.);
#11953=EDGE_CURVE('',#9573,#9575,#630,.T.);
#11954=EDGE_CURVE('',#9576,#9577,#5832,.T.);
#11955=EDGE_CURVE('',#9576,#9574,#631,.T.);
#11956=EDGE_CURVE('',#9575,#9577,#632,.T.);
#11957=EDGE_CURVE('',#9578,#9579,#5833,.T.);
#11958=EDGE_CURVE('',#9578,#9576,#633,.T.);
#11959=EDGE_CURVE('',#9577,#9579,#634,.T.);
#11960=EDGE_CURVE('',#9580,#9581,#5834,.T.);
#11961=EDGE_CURVE('',#9580,#9578,#635,.T.);
#11962=EDGE_CURVE('',#9579,#9581,#636,.T.);
#11963=EDGE_CURVE('',#9582,#9583,#5835,.T.);
#11964=EDGE_CURVE('',#9582,#9580,#637,.T.);
#11965=EDGE_CURVE('',#9581,#9583,#638,.T.);
#11966=EDGE_CURVE('',#9584,#9585,#5836,.T.);
#11967=EDGE_CURVE('',#9584,#9586,#639,.T.);
#11968=EDGE_CURVE('',#9587,#9586,#8555,.T.);
#11969=EDGE_CURVE('',#9585,#9587,#640,.T.);
#11970=EDGE_CURVE('',#9588,#9589,#5837,.T.);
#11971=EDGE_CURVE('',#9588,#9584,#641,.T.);
#11972=EDGE_CURVE('',#9589,#9585,#642,.T.);
#11973=EDGE_CURVE('',#9590,#9591,#5838,.T.);
#11974=EDGE_CURVE('',#9590,#9588,#643,.T.);
#11975=EDGE_CURVE('',#9591,#9589,#644,.T.);
#11976=EDGE_CURVE('',#9592,#9593,#5839,.T.);
#11977=EDGE_CURVE('',#9592,#9590,#645,.T.);
#11978=EDGE_CURVE('',#9593,#9591,#646,.T.);
#11979=EDGE_CURVE('',#9594,#9595,#5840,.T.);
#11980=EDGE_CURVE('',#9594,#9592,#647,.T.);
#11981=EDGE_CURVE('',#9595,#9593,#648,.T.);
#11982=EDGE_CURVE('',#9596,#9597,#5841,.T.);
#11983=EDGE_CURVE('',#9596,#9594,#649,.T.);
#11984=EDGE_CURVE('',#9597,#9595,#650,.T.);
#11985=EDGE_CURVE('',#9598,#9599,#5842,.T.);
#11986=EDGE_CURVE('',#9598,#9596,#651,.T.);
#11987=EDGE_CURVE('',#9599,#9597,#652,.T.);
#11988=EDGE_CURVE('',#9586,#9600,#653,.T.);
#11989=EDGE_CURVE('',#9601,#9600,#8556,.F.);
#11990=EDGE_CURVE('',#9602,#9601,#8557,.F.);
#11991=EDGE_CURVE('',#9602,#9587,#654,.T.);
#11992=EDGE_CURVE('',#9583,#9602,#655,.T.);
#11993=EDGE_CURVE('',#9603,#9571,#656,.T.);
#11994=EDGE_CURVE('',#9603,#9599,#657,.T.);
#11995=EDGE_CURVE('',#9604,#9603,#8558,.T.);
#11996=EDGE_CURVE('',#9604,#9598,#658,.T.);
#11997=EDGE_CURVE('',#9570,#9604,#659,.T.);
#11998=EDGE_CURVE('',#9600,#9582,#660,.T.);
#11999=EDGE_CURVE('',#9600,#9602,#8559,.F.);
#12000=EDGE_CURVE('',#9605,#9606,#661,.T.);
#12001=EDGE_CURVE('',#9607,#9605,#662,.T.);
#12002=EDGE_CURVE('',#9608,#9607,#663,.T.);
#12003=EDGE_CURVE('',#9608,#9606,#664,.T.);
#12004=EDGE_CURVE('',#9606,#9609,#665,.T.);
#12005=EDGE_CURVE('',#9610,#9608,#666,.T.);
#12006=EDGE_CURVE('',#9610,#9609,#667,.T.);
#12007=EDGE_CURVE('',#9609,#9558,#668,.T.);
#12008=EDGE_CURVE('',#9611,#9610,#669,.T.);
#12009=EDGE_CURVE('',#9611,#9566,#670,.T.);
#12010=EDGE_CURVE('',#9607,#9612,#8560,.T.);
#12011=EDGE_CURVE('',#9612,#9607,#8561,.T.);
#12012=EDGE_CURVE('',#9607,#9613,#671,.T.);
#12013=EDGE_CURVE('',#9613,#9614,#672,.T.);
#12014=EDGE_CURVE('',#9614,#9567,#673,.T.);
#12015=EDGE_CURVE('',#9565,#9611,#8562,.T.);
#12016=EDGE_CURVE('',#9557,#9615,#674,.T.);
#12017=EDGE_CURVE('',#9614,#9615,#675,.T.);
#12018=EDGE_CURVE('',#9615,#9616,#676,.T.);
#12019=EDGE_CURVE('',#9613,#9616,#677,.T.);
#12020=EDGE_CURVE('',#9616,#9605,#678,.T.);
#12021=EDGE_CURVE('',#9617,#9617,#8563,.T.);
#12022=EDGE_CURVE('',#9617,#9618,#5843,.T.);
#12023=EDGE_CURVE('',#9619,#9618,#1468,.T.);
#12024=EDGE_CURVE('',#9620,#9619,#1469,.T.);
#12025=EDGE_CURVE('',#9621,#9620,#1470,.T.);
#12026=EDGE_CURVE('',#9622,#9621,#1471,.T.);
#12027=EDGE_CURVE('',#9623,#9622,#1472,.T.);
#12028=EDGE_CURVE('',#9624,#9623,#1473,.T.);
#12029=EDGE_CURVE('',#9618,#9624,#1474,.T.);
#12030=EDGE_CURVE('',#9622,#9625,#5844,.T.);
#12031=EDGE_CURVE('',#9625,#9626,#1475,.T.);
#12032=EDGE_CURVE('',#9623,#9626,#5845,.T.);
#12033=EDGE_CURVE('',#9621,#9627,#5846,.T.);
#12034=EDGE_CURVE('',#9627,#9625,#1476,.T.);
#12035=EDGE_CURVE('',#9620,#9628,#5847,.T.);
#12036=EDGE_CURVE('',#9628,#9627,#1477,.T.);
#12037=EDGE_CURVE('',#9629,#9628,#1478,.T.);
#12038=EDGE_CURVE('',#9630,#9629,#1479,.T.);
#12039=EDGE_CURVE('',#9630,#9631,#5848,.T.);
#12040=EDGE_CURVE('',#9631,#9631,#8564,.T.);
#12041=EDGE_CURVE('',#9632,#9630,#1480,.T.);
#12042=EDGE_CURVE('',#9626,#9632,#1481,.T.);
#12043=EDGE_CURVE('',#9619,#9629,#5849,.T.);
#12044=EDGE_CURVE('',#9633,#9633,#8565,.T.);
#12045=EDGE_CURVE('',#9634,#9634,#8566,.T.);
#12046=EDGE_CURVE('',#9635,#9635,#8567,.T.);
#12047=EDGE_CURVE('',#9624,#9632,#5850,.T.);
#12048=EDGE_CURVE('',#9635,#9636,#5851,.T.);
#12049=EDGE_CURVE('',#9636,#9636,#8568,.T.);
#12050=EDGE_CURVE('',#9637,#9637,#8569,.T.);
#12051=EDGE_CURVE('',#9637,#9633,#5852,.T.);
#12052=EDGE_CURVE('',#9638,#9638,#8570,.T.);
#12053=EDGE_CURVE('',#9612,#9638,#5853,.T.);
#12054=EDGE_CURVE('',#9639,#9639,#8571,.T.);
#12055=EDGE_CURVE('',#9634,#9639,#5854,.T.);
#12056=EDGE_CURVE('',#9640,#9640,#8572,.T.);
#12057=EDGE_CURVE('',#9640,#9601,#5855,.T.);
#12058=EDGE_CURVE('',#9641,#9641,#8573,.T.);
#12059=EDGE_CURVE('',#9641,#9637,#5856,.T.);
#12060=EDGE_CURVE('',#9642,#9642,#8574,.T.);
#12061=EDGE_CURVE('',#9642,#9643,#5857,.T.);
#12062=EDGE_CURVE('',#9643,#9643,#8575,.T.);
#12063=EDGE_CURVE('',#9643,#9644,#5858,.T.);
#12064=EDGE_CURVE('',#9645,#9646,#5859,.T.);
#12065=EDGE_CURVE('',#9647,#9645,#5860,.T.);
#12066=EDGE_CURVE('',#9647,#9648,#5861,.T.);
#12067=EDGE_CURVE('',#9648,#9646,#5862,.T.);
#12068=EDGE_CURVE('',#9646,#9649,#679,.T.);
#12069=EDGE_CURVE('',#9650,#9648,#8576,.T.);
#12070=EDGE_CURVE('',#9650,#9649,#5863,.T.);
#12071=EDGE_CURVE('',#9649,#9651,#5864,.T.);
#12072=EDGE_CURVE('',#9650,#9652,#5865,.T.);
#12073=EDGE_CURVE('',#9652,#9651,#5866,.T.);
#12074=EDGE_CURVE('',#9651,#9645,#680,.T.);
#12075=EDGE_CURVE('',#9647,#9652,#8577,.T.);
#12076=EDGE_CURVE('',#9653,#9654,#5867,.T.);
#12077=EDGE_CURVE('',#9655,#9653,#5868,.T.);
#12078=EDGE_CURVE('',#9655,#9656,#5869,.T.);
#12079=EDGE_CURVE('',#9656,#9654,#5870,.T.);
#12080=EDGE_CURVE('',#9654,#9657,#681,.T.);
#12081=EDGE_CURVE('',#9658,#9656,#8578,.T.);
#12082=EDGE_CURVE('',#9658,#9657,#5871,.T.);
#12083=EDGE_CURVE('',#9657,#9659,#5872,.T.);
#12084=EDGE_CURVE('',#9658,#9660,#5873,.T.);
#12085=EDGE_CURVE('',#9660,#9659,#5874,.T.);
#12086=EDGE_CURVE('',#9659,#9653,#682,.T.);
#12087=EDGE_CURVE('',#9655,#9660,#8579,.T.);
#12088=EDGE_CURVE('',#9661,#9661,#8580,.T.);
#12089=EDGE_CURVE('',#9662,#9662,#8581,.T.);
#12090=EDGE_CURVE('',#9662,#9661,#5875,.T.);
#12091=EDGE_CURVE('',#9663,#9663,#8582,.T.);
#12092=EDGE_CURVE('',#9663,#9662,#5876,.T.);
#12093=EDGE_CURVE('',#9664,#9664,#8583,.T.);
#12094=EDGE_CURVE('',#9665,#9665,#8584,.T.);
#12095=EDGE_CURVE('',#9665,#9664,#5877,.T.);
#12096=EDGE_CURVE('',#9666,#9666,#8585,.T.);
#12097=EDGE_CURVE('',#9666,#9665,#5878,.T.);
#12098=EDGE_CURVE('',#9667,#9667,#8586,.T.);
#12099=EDGE_CURVE('',#9668,#9668,#8587,.T.);
#12100=EDGE_CURVE('',#9668,#9667,#5879,.T.);
#12101=EDGE_CURVE('',#9669,#9669,#8588,.T.);
#12102=EDGE_CURVE('',#9670,#9670,#8589,.T.);
#12103=EDGE_CURVE('',#9670,#9669,#5880,.T.);
#12104=EDGE_CURVE('',#9671,#9671,#8590,.T.);
#12105=EDGE_CURVE('',#9672,#9672,#8591,.T.);
#12106=EDGE_CURVE('',#9672,#9671,#5881,.T.);
#12107=EDGE_CURVE('',#9673,#9673,#8592,.T.);
#12108=EDGE_CURVE('',#9674,#9674,#8593,.T.);
#12109=EDGE_CURVE('',#9674,#9673,#5882,.T.);
#12110=EDGE_CURVE('',#9675,#9675,#8594,.T.);
#12111=EDGE_CURVE('',#9675,#9674,#5883,.T.);
#12112=EDGE_CURVE('',#9676,#9676,#8595,.T.);
#12113=EDGE_CURVE('',#9677,#9677,#8596,.T.);
#12114=EDGE_CURVE('',#9678,#9678,#8597,.T.);
#12115=EDGE_CURVE('',#9678,#9677,#5884,.T.);
#12116=EDGE_CURVE('',#9679,#9679,#8598,.T.);
#12117=EDGE_CURVE('',#9679,#9680,#5885,.T.);
#12118=EDGE_CURVE('',#9680,#9680,#8599,.T.);
#12119=EDGE_CURVE('',#9681,#9682,#5886,.T.);
#12120=EDGE_CURVE('',#9683,#9681,#5887,.T.);
#12121=EDGE_CURVE('',#9683,#9684,#5888,.T.);
#12122=EDGE_CURVE('',#9682,#9684,#5889,.T.);
#12123=EDGE_CURVE('',#9684,#9685,#5890,.T.);
#12124=EDGE_CURVE('',#9686,#9683,#5891,.T.);
#12125=EDGE_CURVE('',#9686,#9685,#5892,.T.);
#12126=EDGE_CURVE('',#9687,#9688,#5893,.T.);
#12127=EDGE_CURVE('',#9685,#9687,#5894,.T.);
#12128=EDGE_CURVE('',#9688,#9686,#5895,.T.);
#12129=EDGE_CURVE('',#9689,#9689,#8600,.T.);
#12130=EDGE_CURVE('',#9681,#9688,#8601,.T.);
#12131=EDGE_CURVE('',#9690,#9690,#8602,.T.);
#12132=EDGE_CURVE('',#9690,#9691,#5896,.T.);
#12133=EDGE_CURVE('',#9691,#9691,#8603,.T.);
#12134=EDGE_CURVE('',#9692,#9692,#8604,.T.);
#12135=EDGE_CURVE('',#9692,#9693,#5897,.T.);
#12136=EDGE_CURVE('',#9693,#9693,#8605,.T.);
#12137=EDGE_CURVE('',#9694,#9694,#8606,.T.);
#12138=EDGE_CURVE('',#9694,#9695,#5898,.T.);
#12139=EDGE_CURVE('',#9695,#9695,#8607,.T.);
#12140=EDGE_CURVE('',#9696,#9696,#8608,.T.);
#12141=EDGE_CURVE('',#9696,#9697,#5899,.T.);
#12142=EDGE_CURVE('',#9697,#9697,#8609,.T.);
#12143=EDGE_CURVE('',#9698,#9698,#8610,.T.);
#12144=EDGE_CURVE('',#9698,#9699,#5900,.T.);
#12145=EDGE_CURVE('',#9699,#9699,#8611,.T.);
#12146=EDGE_CURVE('',#9700,#9700,#8612,.T.);
#12147=EDGE_CURVE('',#9700,#9701,#5901,.T.);
#12148=EDGE_CURVE('',#9701,#9701,#8613,.T.);
#12149=EDGE_CURVE('',#9702,#9702,#8614,.T.);
#12150=EDGE_CURVE('',#9702,#9703,#5902,.T.);
#12151=EDGE_CURVE('',#9703,#9703,#8615,.T.);
#12152=EDGE_CURVE('',#9704,#9704,#8616,.T.);
#12153=EDGE_CURVE('',#9704,#9705,#5903,.T.);
#12154=EDGE_CURVE('',#9705,#9705,#8617,.T.);
#12155=EDGE_CURVE('',#9706,#9706,#8618,.T.);
#12156=EDGE_CURVE('',#9706,#9707,#5904,.T.);
#12157=EDGE_CURVE('',#9707,#9707,#8619,.T.);
#12158=EDGE_CURVE('',#9708,#9709,#683,.T.);
#12159=EDGE_CURVE('',#9710,#9708,#8620,.T.);
#12160=EDGE_CURVE('',#9710,#9711,#5905,.T.);
#12161=EDGE_CURVE('',#9711,#9711,#8621,.T.);
#12162=EDGE_CURVE('',#9709,#9710,#8622,.T.);
#12163=EDGE_CURVE('',#9712,#9713,#684,.T.);
#12164=EDGE_CURVE('',#9714,#9712,#8623,.T.);
#12165=EDGE_CURVE('',#9714,#9715,#5906,.T.);
#12166=EDGE_CURVE('',#9715,#9715,#8624,.T.);
#12167=EDGE_CURVE('',#9713,#9714,#8625,.T.);
#12168=EDGE_CURVE('',#9716,#9717,#685,.T.);
#12169=EDGE_CURVE('',#9718,#9716,#8626,.T.);
#12170=EDGE_CURVE('',#9718,#9719,#5907,.T.);
#12171=EDGE_CURVE('',#9719,#9719,#8627,.T.);
#12172=EDGE_CURVE('',#9717,#9718,#8628,.T.);
#12173=EDGE_CURVE('',#9720,#9721,#686,.T.);
#12174=EDGE_CURVE('',#9722,#9720,#8629,.T.);
#12175=EDGE_CURVE('',#9722,#9723,#5908,.T.);
#12176=EDGE_CURVE('',#9723,#9723,#8630,.T.);
#12177=EDGE_CURVE('',#9721,#9722,#8631,.T.);
#12178=EDGE_CURVE('',#9724,#9725,#687,.T.);
#12179=EDGE_CURVE('',#9726,#9724,#8632,.T.);
#12180=EDGE_CURVE('',#9726,#9727,#5909,.T.);
#12181=EDGE_CURVE('',#9727,#9727,#8633,.T.);
#12182=EDGE_CURVE('',#9725,#9726,#8634,.T.);
#12183=EDGE_CURVE('',#9728,#9729,#688,.T.);
#12184=EDGE_CURVE('',#9730,#9728,#8635,.T.);
#12185=EDGE_CURVE('',#9730,#9731,#5910,.T.);
#12186=EDGE_CURVE('',#9731,#9731,#8636,.T.);
#12187=EDGE_CURVE('',#9729,#9730,#8637,.T.);
#12188=EDGE_CURVE('',#9732,#9733,#689,.T.);
#12189=EDGE_CURVE('',#9734,#9732,#8638,.T.);
#12190=EDGE_CURVE('',#9734,#9735,#5911,.T.);
#12191=EDGE_CURVE('',#9735,#9735,#8639,.T.);
#12192=EDGE_CURVE('',#9733,#9734,#8640,.T.);
#12193=EDGE_CURVE('',#9736,#9737,#690,.T.);
#12194=EDGE_CURVE('',#9738,#9736,#8641,.T.);
#12195=EDGE_CURVE('',#9738,#9739,#5912,.T.);
#12196=EDGE_CURVE('',#9739,#9739,#8642,.T.);
#12197=EDGE_CURVE('',#9737,#9738,#8643,.T.);
#12198=EDGE_CURVE('',#9740,#9741,#691,.T.);
#12199=EDGE_CURVE('',#9742,#9740,#8644,.T.);
#12200=EDGE_CURVE('',#9742,#9743,#5913,.T.);
#12201=EDGE_CURVE('',#9743,#9743,#8645,.T.);
#12202=EDGE_CURVE('',#9741,#9742,#8646,.T.);
#12203=EDGE_CURVE('',#9737,#9708,#8647,.T.);
#12204=EDGE_CURVE('',#9713,#9736,#8648,.T.);
#12205=EDGE_CURVE('',#9744,#9712,#8649,.T.);
#12206=EDGE_CURVE('',#9717,#9744,#8650,.T.);
#12207=EDGE_CURVE('',#9729,#9716,#8651,.T.);
#12208=EDGE_CURVE('',#9721,#9728,#8652,.T.);
#12209=EDGE_CURVE('',#9725,#9720,#8653,.T.);
#12210=EDGE_CURVE('',#9733,#9724,#8654,.T.);
#12211=EDGE_CURVE('',#9741,#9732,#8655,.T.);
#12212=EDGE_CURVE('',#9709,#9740,#8656,.T.);
#12213=EDGE_CURVE('',#9745,#9745,#8657,.T.);
#12214=EDGE_CURVE('',#9689,#9746,#5914,.T.);
#12215=EDGE_CURVE('',#9746,#9746,#8658,.T.);
#12216=EDGE_CURVE('',#9746,#9745,#5915,.T.);
#12217=EDGE_CURVE('',#9680,#9744,#5916,.T.);
#12218=EDGE_CURVE('',#9747,#9747,#8659,.T.);
#12219=EDGE_CURVE('',#9747,#9676,#5917,.T.);
#12220=EDGE_CURVE('',#9748,#9748,#8660,.T.);
#12221=EDGE_CURVE('',#9748,#9747,#5918,.T.);
#12222=EDGE_CURVE('',#9682,#9687,#8661,.T.);
#12223=EDGE_CURVE('',#9749,#9750,#5919,.T.);
#12224=EDGE_CURVE('',#9749,#9751,#5920,.T.);
#12225=EDGE_CURVE('',#9751,#9752,#5921,.T.);
#12226=EDGE_CURVE('',#9750,#9752,#5922,.T.);
#12227=EDGE_CURVE('',#9753,#9749,#5923,.T.);
#12228=EDGE_CURVE('',#9753,#9754,#5924,.T.);
#12229=EDGE_CURVE('',#9754,#9751,#5925,.T.);
#12230=EDGE_CURVE('',#9755,#9753,#5926,.T.);
#12231=EDGE_CURVE('',#9755,#9756,#5927,.T.);
#12232=EDGE_CURVE('',#9756,#9754,#5928,.T.);
#12233=EDGE_CURVE('',#9757,#9755,#5929,.T.);
#12234=EDGE_CURVE('',#9757,#9758,#5930,.T.);
#12235=EDGE_CURVE('',#9758,#9756,#5931,.T.);
#12236=EDGE_CURVE('',#9759,#9757,#8662,.T.);
#12237=EDGE_CURVE('',#9759,#9760,#5932,.T.);
#12238=EDGE_CURVE('',#9760,#9758,#8663,.T.);
#12239=EDGE_CURVE('',#9761,#9759,#5933,.T.);
#12240=EDGE_CURVE('',#9761,#9762,#5934,.T.);
#12241=EDGE_CURVE('',#9762,#9760,#5935,.T.);
#12242=EDGE_CURVE('',#9750,#9761,#8664,.T.);
#12243=EDGE_CURVE('',#9752,#9762,#8665,.T.);
#12244=EDGE_CURVE('',#9763,#9763,#8666,.T.);
#12245=EDGE_CURVE('',#9763,#9764,#5936,.T.);
#12246=EDGE_CURVE('',#9764,#9765,#8667,.T.);
#12247=EDGE_CURVE('',#9765,#9764,#8668,.T.);
#12248=EDGE_CURVE('',#9766,#9766,#8669,.T.);
#12249=EDGE_CURVE('',#9765,#9767,#5937,.T.);
#12250=EDGE_CURVE('',#9767,#9767,#8670,.T.);
#12251=EDGE_CURVE('',#9768,#9768,#8671,.T.);
#12252=EDGE_CURVE('',#9768,#9769,#5938,.T.);
#12253=EDGE_CURVE('',#9769,#9770,#8672,.T.);
#12254=EDGE_CURVE('',#9770,#9769,#8673,.T.);
#12255=EDGE_CURVE('',#9771,#9771,#8674,.T.);
#12256=EDGE_CURVE('',#9770,#9772,#5939,.T.);
#12257=EDGE_CURVE('',#9772,#9772,#8675,.T.);
#12258=EDGE_CURVE('',#9773,#9773,#8676,.T.);
#12259=EDGE_CURVE('',#9773,#9774,#5940,.T.);
#12260=EDGE_CURVE('',#9774,#9775,#8677,.T.);
#12261=EDGE_CURVE('',#9775,#9774,#8678,.T.);
#12262=EDGE_CURVE('',#9776,#9776,#8679,.T.);
#12263=EDGE_CURVE('',#9775,#9777,#5941,.T.);
#12264=EDGE_CURVE('',#9777,#9777,#8680,.T.);
#12265=EDGE_CURVE('',#9778,#9778,#8681,.T.);
#12266=EDGE_CURVE('',#9778,#9779,#5942,.T.);
#12267=EDGE_CURVE('',#9779,#9780,#8682,.T.);
#12268=EDGE_CURVE('',#9780,#9779,#8683,.T.);
#12269=EDGE_CURVE('',#9781,#9781,#8684,.T.);
#12270=EDGE_CURVE('',#9780,#9782,#5943,.T.);
#12271=EDGE_CURVE('',#9782,#9782,#8685,.T.);
#12272=EDGE_CURVE('',#9783,#9783,#8686,.T.);
#12273=EDGE_CURVE('',#9783,#9784,#5944,.T.);
#12274=EDGE_CURVE('',#9784,#9785,#8687,.T.);
#12275=EDGE_CURVE('',#9785,#9784,#8688,.T.);
#12276=EDGE_CURVE('',#9786,#9786,#8689,.T.);
#12277=EDGE_CURVE('',#9785,#9787,#5945,.T.);
#12278=EDGE_CURVE('',#9787,#9787,#8690,.T.);
#12279=EDGE_CURVE('',#9788,#9788,#8691,.T.);
#12280=EDGE_CURVE('',#9788,#9789,#5946,.T.);
#12281=EDGE_CURVE('',#9789,#9790,#8692,.T.);
#12282=EDGE_CURVE('',#9790,#9789,#8693,.T.);
#12283=EDGE_CURVE('',#9791,#9791,#8694,.T.);
#12284=EDGE_CURVE('',#9790,#9792,#5947,.T.);
#12285=EDGE_CURVE('',#9792,#9792,#8695,.T.);
#12286=EDGE_CURVE('',#9793,#9794,#8696,.T.);
#12287=EDGE_CURVE('',#9795,#9793,#692,.T.);
#12288=EDGE_CURVE('',#9794,#9795,#8697,.T.);
#12289=EDGE_CURVE('',#9794,#9791,#5948,.T.);
#12290=EDGE_CURVE('',#9796,#9796,#8698,.T.);
#12291=EDGE_CURVE('',#9796,#9797,#8699,.T.);
#12292=EDGE_CURVE('',#9797,#9798,#693,.T.);
#12293=EDGE_CURVE('',#9798,#9799,#8700,.T.);
#12294=EDGE_CURVE('',#9799,#9800,#694,.T.);
#12295=EDGE_CURVE('',#9800,#9801,#8701,.T.);
#12296=EDGE_CURVE('',#9801,#9802,#695,.T.);
#12297=EDGE_CURVE('',#9802,#9803,#8702,.T.);
#12298=EDGE_CURVE('',#9803,#9804,#696,.T.);
#12299=EDGE_CURVE('',#9804,#9805,#697,.T.);
#12300=EDGE_CURVE('',#9805,#9795,#8703,.T.);
#12301=EDGE_CURVE('',#9793,#9806,#8704,.T.);
#12302=EDGE_CURVE('',#9806,#9807,#698,.T.);
#12303=EDGE_CURVE('',#9807,#9808,#8705,.T.);
#12304=EDGE_CURVE('',#9808,#9797,#699,.T.);
#12305=EDGE_CURVE('',#9809,#9806,#8706,.T.);
#12306=EDGE_CURVE('',#9809,#9786,#5949,.T.);
#12307=EDGE_CURVE('',#9807,#9809,#8707,.T.);
#12308=EDGE_CURVE('',#9810,#9810,#8708,.T.);
#12309=EDGE_CURVE('',#9805,#9803,#8709,.T.);
#12310=EDGE_CURVE('',#9802,#9811,#8710,.T.);
#12311=EDGE_CURVE('',#9811,#9801,#8711,.T.);
#12312=EDGE_CURVE('',#9800,#9812,#8712,.T.);
#12313=EDGE_CURVE('',#9812,#9799,#8713,.T.);
#12314=EDGE_CURVE('',#9798,#9813,#8714,.T.);
#12315=EDGE_CURVE('',#9813,#9808,#8715,.T.);
#12316=EDGE_CURVE('',#9813,#9781,#5950,.T.);
#12317=EDGE_CURVE('',#9812,#9776,#5951,.T.);
#12318=EDGE_CURVE('',#9811,#9771,#5952,.T.);
#12319=EDGE_CURVE('',#9804,#9766,#5953,.T.);
#12320=EDGE_CURVE('',#9814,#9814,#8716,.T.);
#12321=EDGE_CURVE('',#9814,#9815,#5954,.T.);
#12322=EDGE_CURVE('',#9815,#9815,#8717,.T.);
#12323=EDGE_CURVE('',#9815,#9816,#5955,.T.);
#12324=EDGE_CURVE('',#9817,#9816,#700,.T.);
#12325=EDGE_CURVE('',#9816,#9817,#701,.T.);
#12326=EDGE_CURVE('',#9818,#9818,#8718,.T.);
#12327=EDGE_CURVE('',#9818,#9819,#5956,.T.);
#12328=EDGE_CURVE('',#9819,#9819,#8719,.T.);
#12329=EDGE_CURVE('',#9819,#9820,#5957,.T.);
#12330=EDGE_CURVE('',#9821,#9820,#702,.T.);
#12331=EDGE_CURVE('',#9820,#9821,#703,.T.);
#12332=EDGE_CURVE('',#9822,#9823,#8720,.T.);
#12333=EDGE_CURVE('',#9823,#9822,#8721,.T.);
#12334=EDGE_CURVE('',#9822,#9824,#5958,.T.);
#12335=EDGE_CURVE('',#9824,#9824,#8722,.T.);
#12336=EDGE_CURVE('',#9825,#9825,#8723,.T.);
#12337=EDGE_CURVE('',#9823,#9826,#5959,.T.);
#12338=EDGE_CURVE('',#9826,#9826,#8724,.T.);
#12339=EDGE_CURVE('',#9827,#9827,#8725,.T.);
#12340=EDGE_CURVE('',#9827,#9828,#5960,.T.);
#12341=EDGE_CURVE('',#9828,#9829,#8726,.T.);
#12342=EDGE_CURVE('',#9829,#9828,#8727,.T.);
#12343=EDGE_CURVE('',#9830,#9830,#8728,.T.);
#12344=EDGE_CURVE('',#9830,#9829,#5961,.T.);
#12345=EDGE_CURVE('',#9831,#9831,#8729,.T.);
#12346=EDGE_CURVE('',#9832,#9832,#8730,.T.);
#12347=EDGE_CURVE('',#9832,#9833,#8731,.T.);
#12348=EDGE_CURVE('',#9833,#9833,#8732,.T.);
#12349=EDGE_CURVE('',#9796,#9832,#5962,.T.);
#12350=EDGE_CURVE('',#9833,#9834,#5963,.T.);
#12351=EDGE_CURVE('',#9834,#9834,#8733,.T.);
#12352=EDGE_CURVE('',#9835,#9835,#8734,.T.);
#12353=EDGE_CURVE('',#9835,#9831,#5964,.T.);
#12354=EDGE_CURVE('',#9834,#9835,#5965,.T.);
#12355=EDGE_CURVE('',#9836,#9836,#8735,.T.);
#12356=EDGE_CURVE('',#9836,#9810,#5966,.T.);
#12357=EDGE_CURVE('',#9837,#9837,#8736,.T.);
#12358=EDGE_CURVE('',#9837,#9836,#5967,.T.);
#12359=EDGE_CURVE('',#9825,#9837,#5968,.T.);
#12360=EDGE_CURVE('',#9838,#9838,#8737,.T.);
#12361=EDGE_CURVE('',#9838,#9839,#5969,.T.);
#12362=EDGE_CURVE('',#9839,#9839,#8738,.T.);
#12363=EDGE_CURVE('',#9840,#9840,#8739,.T.);
#12364=EDGE_CURVE('',#9840,#9841,#5970,.T.);
#12365=EDGE_CURVE('',#9841,#9841,#8740,.T.);
#12366=EDGE_CURVE('',#9842,#9842,#8741,.T.);
#12367=EDGE_CURVE('',#9842,#9843,#5971,.T.);
#12368=EDGE_CURVE('',#9843,#9843,#8742,.T.);
#12369=EDGE_CURVE('',#9844,#9844,#8743,.T.);
#12370=EDGE_CURVE('',#9844,#9845,#5972,.T.);
#12371=EDGE_CURVE('',#9845,#9845,#8744,.T.);
#12372=EDGE_CURVE('',#9846,#9846,#8745,.T.);
#12373=EDGE_CURVE('',#9846,#9847,#5973,.T.);
#12374=EDGE_CURVE('',#9847,#9847,#8746,.T.);
#12375=EDGE_CURVE('',#9848,#9848,#8747,.T.);
#12376=EDGE_CURVE('',#9848,#9847,#5974,.T.);
#12377=EDGE_CURVE('',#9849,#9850,#5975,.T.);
#12378=EDGE_CURVE('',#9850,#9851,#8748,.T.);
#12379=EDGE_CURVE('',#9851,#9852,#5976,.T.);
#12380=EDGE_CURVE('',#9852,#9849,#8749,.T.);
#12381=EDGE_CURVE('',#9853,#9853,#8750,.T.);
#12382=EDGE_CURVE('',#9854,#9854,#8751,.T.);
#12383=EDGE_CURVE('',#9855,#9855,#8752,.T.);
#12384=EDGE_CURVE('',#9856,#9856,#8753,.T.);
#12385=EDGE_CURVE('',#9857,#9857,#8754,.T.);
#12386=EDGE_CURVE('',#9858,#9858,#8755,.T.);
#12387=EDGE_CURVE('',#9859,#9859,#8756,.T.);
#12388=EDGE_CURVE('',#9860,#9860,#8757,.T.);
#12389=EDGE_CURVE('',#9860,#9848,#5977,.T.);
#12390=EDGE_CURVE('',#9861,#9862,#5978,.T.);
#12391=EDGE_CURVE('',#9863,#9862,#8758,.T.);
#12392=EDGE_CURVE('',#9863,#9864,#5979,.T.);
#12393=EDGE_CURVE('',#9861,#9864,#8759,.T.);
#12394=EDGE_CURVE('',#9865,#9865,#8760,.T.);
#12395=EDGE_CURVE('',#9866,#9866,#8761,.T.);
#12396=EDGE_CURVE('',#9867,#9867,#8762,.T.);
#12397=EDGE_CURVE('',#9868,#9869,#8763,.T.);
#12398=EDGE_CURVE('',#9869,#9870,#8764,.T.);
#12399=EDGE_CURVE('',#9870,#9871,#8765,.T.);
#12400=EDGE_CURVE('',#9871,#9868,#8766,.T.);
#12401=EDGE_CURVE('',#9872,#9873,#8767,.T.);
#12402=EDGE_CURVE('',#9873,#9874,#8768,.T.);
#12403=EDGE_CURVE('',#9874,#9875,#8769,.T.);
#12404=EDGE_CURVE('',#9875,#9872,#8770,.T.);
#12405=EDGE_CURVE('',#9876,#9876,#8771,.T.);
#12406=EDGE_CURVE('',#9877,#9877,#8772,.T.);
#12407=EDGE_CURVE('',#9878,#9878,#8773,.T.);
#12408=EDGE_CURVE('',#9853,#9879,#5980,.T.);
#12409=EDGE_CURVE('',#9879,#9879,#8774,.T.);
#12410=EDGE_CURVE('',#9880,#9880,#8775,.T.);
#12411=EDGE_CURVE('',#9880,#9879,#5981,.T.);
#12412=EDGE_CURVE('',#9865,#9880,#5982,.T.);
#12413=EDGE_CURVE('',#9859,#9881,#5983,.T.);
#12414=EDGE_CURVE('',#9881,#9881,#8776,.T.);
#12415=EDGE_CURVE('',#9882,#9882,#8777,.T.);
#12416=EDGE_CURVE('',#9882,#9881,#5984,.T.);
#12417=EDGE_CURVE('',#9878,#9882,#5985,.T.);
#12418=EDGE_CURVE('',#9854,#9883,#5986,.T.);
#12419=EDGE_CURVE('',#9883,#9883,#8778,.T.);
#12420=EDGE_CURVE('',#9884,#9884,#8779,.T.);
#12421=EDGE_CURVE('',#9884,#9883,#5987,.T.);
#12422=EDGE_CURVE('',#9866,#9884,#5988,.T.);
#12423=EDGE_CURVE('',#9858,#9885,#5989,.T.);
#12424=EDGE_CURVE('',#9885,#9885,#8780,.T.);
#12425=EDGE_CURVE('',#9886,#9886,#8781,.T.);
#12426=EDGE_CURVE('',#9886,#9885,#5990,.T.);
#12427=EDGE_CURVE('',#9877,#9886,#5991,.T.);
#12428=EDGE_CURVE('',#9855,#9887,#5992,.T.);
#12429=EDGE_CURVE('',#9887,#9887,#8782,.T.);
#12430=EDGE_CURVE('',#9888,#9888,#8783,.T.);
#12431=EDGE_CURVE('',#9888,#9887,#5993,.T.);
#12432=EDGE_CURVE('',#9867,#9888,#5994,.T.);
#12433=EDGE_CURVE('',#9889,#9890,#704,.T.);
#12434=EDGE_CURVE('',#9890,#9889,#705,.T.);
#12435=EDGE_CURVE('',#9890,#9857,#5995,.T.);
#12436=EDGE_CURVE('',#9891,#9891,#8784,.T.);
#12437=EDGE_CURVE('',#9891,#9892,#5996,.T.);
#12438=EDGE_CURVE('',#9892,#9892,#8785,.T.);
#12439=EDGE_CURVE('',#9893,#9893,#8786,.T.);
#12440=EDGE_CURVE('',#9893,#9892,#5997,.T.);
#12441=EDGE_CURVE('',#9894,#9851,#1482,.T.);
#12442=EDGE_CURVE('',#9895,#9894,#5998,.T.);
#12443=EDGE_CURVE('',#9864,#9895,#1483,.T.);
#12444=EDGE_CURVE('',#9896,#9863,#1484,.T.);
#12445=EDGE_CURVE('',#9897,#9896,#5999,.T.);
#12446=EDGE_CURVE('',#9852,#9897,#1485,.T.);
#12447=EDGE_CURVE('',#9898,#9898,#8787,.T.);
#12448=EDGE_CURVE('',#9898,#9899,#6000,.T.);
#12449=EDGE_CURVE('',#9899,#9899,#8788,.T.);
#12450=EDGE_CURVE('',#9899,#9900,#6001,.T.);
#12451=EDGE_CURVE('',#9900,#9900,#8789,.T.);
#12452=EDGE_CURVE('',#9901,#9849,#1486,.T.);
#12453=EDGE_CURVE('',#9902,#9901,#6002,.T.);
#12454=EDGE_CURVE('',#9862,#9902,#1487,.T.);
#12455=EDGE_CURVE('',#9903,#9861,#1488,.T.);
#12456=EDGE_CURVE('',#9904,#9903,#6003,.T.);
#12457=EDGE_CURVE('',#9850,#9904,#1489,.T.);
#12458=EDGE_CURVE('',#9905,#9905,#8790,.T.);
#12459=EDGE_CURVE('',#9905,#9906,#6004,.T.);
#12460=EDGE_CURVE('',#9907,#9906,#706,.T.);
#12461=EDGE_CURVE('',#9908,#9907,#6005,.T.);
#12462=EDGE_CURVE('',#9908,#9909,#8791,.T.);
#12463=EDGE_CURVE('',#9910,#9909,#6006,.T.);
#12464=EDGE_CURVE('',#9906,#9910,#707,.T.);
#12465=EDGE_CURVE('',#9911,#9912,#708,.T.);
#12466=EDGE_CURVE('',#9911,#9913,#8792,.T.);
#12467=EDGE_CURVE('',#9913,#9912,#8793,.T.);
#12468=EDGE_CURVE('',#9914,#9911,#709,.T.);
#12469=EDGE_CURVE('',#9909,#9914,#1490,.T.);
#12470=EDGE_CURVE('',#9915,#9908,#1491,.T.);
#12471=EDGE_CURVE('',#9912,#9915,#710,.T.);
#12472=EDGE_CURVE('',#9913,#9916,#6007,.T.);
#12473=EDGE_CURVE('',#9915,#9917,#8794,.T.);
#12474=EDGE_CURVE('',#9873,#9917,#6008,.T.);
#12475=EDGE_CURVE('',#9872,#9918,#6009,.T.);
#12476=EDGE_CURVE('',#9918,#9914,#8795,.T.);
#12477=EDGE_CURVE('',#9919,#9907,#8796,.T.);
#12478=EDGE_CURVE('',#9917,#9919,#8797,.T.);
#12479=EDGE_CURVE('',#9896,#9902,#8798,.T.);
#12480=EDGE_CURVE('',#9897,#9901,#8799,.T.);
#12481=EDGE_CURVE('',#9920,#9921,#6010,.T.);
#12482=EDGE_CURVE('',#9922,#9920,#711,.T.);
#12483=EDGE_CURVE('',#9922,#9923,#6011,.T.);
#12484=EDGE_CURVE('',#9923,#9923,#8800,.T.);
#12485=EDGE_CURVE('',#9924,#9922,#712,.T.);
#12486=EDGE_CURVE('',#9925,#9924,#6012,.T.);
#12487=EDGE_CURVE('',#9921,#9925,#8801,.T.);
#12488=EDGE_CURVE('',#9926,#9927,#713,.T.);
#12489=EDGE_CURVE('',#9928,#9926,#8802,.T.);
#12490=EDGE_CURVE('',#9927,#9928,#8803,.T.);
#12491=EDGE_CURVE('',#9929,#9928,#6013,.T.);
#12492=EDGE_CURVE('',#9930,#9926,#714,.T.);
#12493=EDGE_CURVE('',#9921,#9930,#1492,.T.);
#12494=EDGE_CURVE('',#9931,#9925,#1493,.T.);
#12495=EDGE_CURVE('',#9927,#9931,#715,.T.);
#12496=EDGE_CURVE('',#9931,#9932,#8804,.T.);
#12497=EDGE_CURVE('',#9869,#9932,#6014,.T.);
#12498=EDGE_CURVE('',#9868,#9933,#6015,.T.);
#12499=EDGE_CURVE('',#9933,#9930,#8805,.T.);
#12500=EDGE_CURVE('',#9934,#9924,#8806,.T.);
#12501=EDGE_CURVE('',#9932,#9934,#8807,.T.);
#12502=EDGE_CURVE('',#9871,#9935,#6016,.T.);
#12503=EDGE_CURVE('',#9935,#9933,#8808,.T.);
#12504=EDGE_CURVE('',#9920,#9935,#8809,.T.);
#12505=EDGE_CURVE('',#9870,#9934,#6017,.T.);
#12506=EDGE_CURVE('',#9875,#9936,#6018,.T.);
#12507=EDGE_CURVE('',#9936,#9918,#8810,.T.);
#12508=EDGE_CURVE('',#9910,#9936,#8811,.T.);
#12509=EDGE_CURVE('',#9874,#9919,#6019,.T.);
#12510=EDGE_CURVE('',#9876,#9937,#6020,.T.);
#12511=EDGE_CURVE('',#9937,#9938,#8812,.T.);
#12512=EDGE_CURVE('',#9938,#9937,#8813,.T.);
#12513=EDGE_CURVE('',#9939,#9940,#8814,.T.);
#12514=EDGE_CURVE('',#9940,#9939,#8815,.T.);
#12515=EDGE_CURVE('',#9940,#9938,#6021,.T.);
#12516=EDGE_CURVE('',#9939,#9856,#6022,.T.);
#12517=EDGE_CURVE('',#9903,#9895,#8816,.T.);
#12518=EDGE_CURVE('',#9904,#9894,#8817,.T.);
#12519=EDGE_CURVE('',#9941,#9942,#716,.T.);
#12520=EDGE_CURVE('',#9941,#9943,#6023,.T.);
#12521=EDGE_CURVE('',#9943,#9944,#717,.T.);
#12522=EDGE_CURVE('',#9942,#9944,#6024,.T.);
#12523=EDGE_CURVE('',#9945,#9941,#718,.T.);
#12524=EDGE_CURVE('',#9945,#9946,#6025,.T.);
#12525=EDGE_CURVE('',#9946,#9943,#719,.T.);
#12526=EDGE_CURVE('',#9947,#9945,#720,.T.);
#12527=EDGE_CURVE('',#9947,#9948,#6026,.T.);
#12528=EDGE_CURVE('',#9948,#9946,#721,.T.);
#12529=EDGE_CURVE('',#9949,#9947,#722,.T.);
#12530=EDGE_CURVE('',#9949,#9950,#6027,.T.);
#12531=EDGE_CURVE('',#9950,#9948,#723,.T.);
#12532=EDGE_CURVE('',#9951,#9949,#724,.T.);
#12533=EDGE_CURVE('',#9951,#9952,#6028,.T.);
#12534=EDGE_CURVE('',#9952,#9950,#725,.T.);
#12535=EDGE_CURVE('',#9953,#9951,#726,.T.);
#12536=EDGE_CURVE('',#9953,#9954,#6029,.T.);
#12537=EDGE_CURVE('',#9954,#9952,#727,.T.);
#12538=EDGE_CURVE('',#9955,#9953,#728,.T.);
#12539=EDGE_CURVE('',#9955,#9956,#6030,.T.);
#12540=EDGE_CURVE('',#9956,#9954,#729,.T.);
#12541=EDGE_CURVE('',#9957,#9955,#730,.T.);
#12542=EDGE_CURVE('',#9957,#9958,#6031,.T.);
#12543=EDGE_CURVE('',#9958,#9956,#731,.T.);
#12544=EDGE_CURVE('',#9959,#9957,#732,.T.);
#12545=EDGE_CURVE('',#9959,#9960,#6032,.T.);
#12546=EDGE_CURVE('',#9960,#9958,#733,.T.);
#12547=EDGE_CURVE('',#9942,#9959,#6033,.T.);
#12548=EDGE_CURVE('',#9944,#9960,#6034,.T.);
#12549=EDGE_CURVE('',#9961,#9962,#734,.T.);
#12550=EDGE_CURVE('',#9961,#9963,#6035,.T.);
#12551=EDGE_CURVE('',#9963,#9964,#735,.T.);
#12552=EDGE_CURVE('',#9962,#9964,#6036,.T.);
#12553=EDGE_CURVE('',#9965,#9961,#736,.T.);
#12554=EDGE_CURVE('',#9965,#9966,#6037,.T.);
#12555=EDGE_CURVE('',#9966,#9963,#737,.T.);
#12556=EDGE_CURVE('',#9967,#9965,#6038,.T.);
#12557=EDGE_CURVE('',#9967,#9968,#6039,.T.);
#12558=EDGE_CURVE('',#9968,#9966,#6040,.T.);
#12559=EDGE_CURVE('',#9969,#9967,#738,.T.);
#12560=EDGE_CURVE('',#9969,#9970,#6041,.T.);
#12561=EDGE_CURVE('',#9970,#9968,#739,.T.);
#12562=EDGE_CURVE('',#9971,#9969,#740,.T.);
#12563=EDGE_CURVE('',#9971,#9972,#6042,.T.);
#12564=EDGE_CURVE('',#9972,#9970,#741,.T.);
#12565=EDGE_CURVE('',#9973,#9971,#742,.T.);
#12566=EDGE_CURVE('',#9973,#9974,#6043,.T.);
#12567=EDGE_CURVE('',#9974,#9972,#743,.T.);
#12568=EDGE_CURVE('',#9975,#9973,#744,.T.);
#12569=EDGE_CURVE('',#9975,#9976,#6044,.T.);
#12570=EDGE_CURVE('',#9976,#9974,#745,.T.);
#12571=EDGE_CURVE('',#9977,#9975,#746,.T.);
#12572=EDGE_CURVE('',#9977,#9978,#6045,.T.);
#12573=EDGE_CURVE('',#9978,#9976,#747,.T.);
#12574=EDGE_CURVE('',#9979,#9977,#748,.T.);
#12575=EDGE_CURVE('',#9979,#9980,#6046,.T.);
#12576=EDGE_CURVE('',#9980,#9978,#749,.T.);
#12577=EDGE_CURVE('',#9981,#9979,#750,.T.);
#12578=EDGE_CURVE('',#9981,#9982,#6047,.T.);
#12579=EDGE_CURVE('',#9982,#9980,#751,.T.);
#12580=EDGE_CURVE('',#9983,#9981,#6048,.T.);
#12581=EDGE_CURVE('',#9983,#9984,#6049,.T.);
#12582=EDGE_CURVE('',#9984,#9982,#6050,.T.);
#12583=EDGE_CURVE('',#9985,#9983,#752,.T.);
#12584=EDGE_CURVE('',#9985,#9986,#6051,.T.);
#12585=EDGE_CURVE('',#9986,#9984,#753,.T.);
#12586=EDGE_CURVE('',#9987,#9985,#754,.T.);
#12587=EDGE_CURVE('',#9987,#9988,#6052,.T.);
#12588=EDGE_CURVE('',#9988,#9986,#755,.T.);
#12589=EDGE_CURVE('',#9989,#9987,#756,.T.);
#12590=EDGE_CURVE('',#9989,#9990,#6053,.T.);
#12591=EDGE_CURVE('',#9990,#9988,#757,.T.);
#12592=EDGE_CURVE('',#9991,#9989,#758,.T.);
#12593=EDGE_CURVE('',#9991,#9992,#6054,.T.);
#12594=EDGE_CURVE('',#9992,#9990,#759,.T.);
#12595=EDGE_CURVE('',#9993,#9991,#760,.T.);
#12596=EDGE_CURVE('',#9993,#9994,#6055,.T.);
#12597=EDGE_CURVE('',#9994,#9992,#761,.T.);
#12598=EDGE_CURVE('',#9995,#9993,#762,.T.);
#12599=EDGE_CURVE('',#9995,#9996,#6056,.T.);
#12600=EDGE_CURVE('',#9996,#9994,#763,.T.);
#12601=EDGE_CURVE('',#9997,#9995,#764,.T.);
#12602=EDGE_CURVE('',#9997,#9998,#6057,.T.);
#12603=EDGE_CURVE('',#9998,#9996,#765,.T.);
#12604=EDGE_CURVE('',#9999,#9997,#766,.T.);
#12605=EDGE_CURVE('',#9999,#10000,#6058,.T.);
#12606=EDGE_CURVE('',#10000,#9998,#767,.T.);
#12607=EDGE_CURVE('',#10001,#9999,#768,.T.);
#12608=EDGE_CURVE('',#10001,#10002,#6059,.T.);
#12609=EDGE_CURVE('',#10002,#10000,#769,.T.);
#12610=EDGE_CURVE('',#10003,#10001,#770,.T.);
#12611=EDGE_CURVE('',#10003,#10004,#6060,.T.);
#12612=EDGE_CURVE('',#10004,#10002,#771,.T.);
#12613=EDGE_CURVE('',#10005,#10003,#772,.T.);
#12614=EDGE_CURVE('',#10005,#10006,#6061,.T.);
#12615=EDGE_CURVE('',#10006,#10004,#773,.T.);
#12616=EDGE_CURVE('',#10007,#10005,#774,.T.);
#12617=EDGE_CURVE('',#10007,#10008,#6062,.T.);
#12618=EDGE_CURVE('',#10008,#10006,#775,.T.);
#12619=EDGE_CURVE('',#10009,#10007,#776,.T.);
#12620=EDGE_CURVE('',#10009,#10010,#6063,.T.);
#12621=EDGE_CURVE('',#10010,#10008,#777,.T.);
#12622=EDGE_CURVE('',#10011,#10009,#778,.T.);
#12623=EDGE_CURVE('',#10011,#10012,#6064,.T.);
#12624=EDGE_CURVE('',#10012,#10010,#779,.T.);
#12625=EDGE_CURVE('',#10013,#10011,#780,.T.);
#12626=EDGE_CURVE('',#10013,#10014,#6065,.T.);
#12627=EDGE_CURVE('',#10014,#10012,#781,.T.);
#12628=EDGE_CURVE('',#9962,#10013,#6066,.T.);
#12629=EDGE_CURVE('',#9964,#10014,#6067,.T.);
#12630=EDGE_CURVE('',#10015,#10016,#782,.T.);
#12631=EDGE_CURVE('',#10015,#10017,#6068,.T.);
#12632=EDGE_CURVE('',#10017,#10018,#783,.T.);
#12633=EDGE_CURVE('',#10016,#10018,#6069,.T.);
#12634=EDGE_CURVE('',#10019,#10015,#784,.T.);
#12635=EDGE_CURVE('',#10019,#10020,#6070,.T.);
#12636=EDGE_CURVE('',#10020,#10017,#785,.T.);
#12637=EDGE_CURVE('',#10021,#10019,#786,.T.);
#12638=EDGE_CURVE('',#10021,#10022,#6071,.T.);
#12639=EDGE_CURVE('',#10022,#10020,#787,.T.);
#12640=EDGE_CURVE('',#10023,#10021,#788,.T.);
#12641=EDGE_CURVE('',#10023,#10024,#6072,.T.);
#12642=EDGE_CURVE('',#10024,#10022,#789,.T.);
#12643=EDGE_CURVE('',#10025,#10023,#790,.T.);
#12644=EDGE_CURVE('',#10025,#10026,#6073,.T.);
#12645=EDGE_CURVE('',#10026,#10024,#791,.T.);
#12646=EDGE_CURVE('',#10027,#10025,#792,.T.);
#12647=EDGE_CURVE('',#10027,#10028,#6074,.T.);
#12648=EDGE_CURVE('',#10028,#10026,#793,.T.);
#12649=EDGE_CURVE('',#10029,#10027,#794,.T.);
#12650=EDGE_CURVE('',#10029,#10030,#6075,.T.);
#12651=EDGE_CURVE('',#10030,#10028,#795,.T.);
#12652=EDGE_CURVE('',#10016,#10029,#796,.T.);
#12653=EDGE_CURVE('',#10018,#10030,#797,.T.);
#12654=EDGE_CURVE('',#10031,#10032,#798,.T.);
#12655=EDGE_CURVE('',#10031,#10033,#6076,.T.);
#12656=EDGE_CURVE('',#10033,#10034,#799,.T.);
#12657=EDGE_CURVE('',#10032,#10034,#6077,.T.);
#12658=EDGE_CURVE('',#10035,#10031,#800,.T.);
#12659=EDGE_CURVE('',#10035,#10036,#6078,.T.);
#12660=EDGE_CURVE('',#10036,#10033,#801,.T.);
#12661=EDGE_CURVE('',#10037,#10035,#802,.T.);
#12662=EDGE_CURVE('',#10037,#10038,#6079,.T.);
#12663=EDGE_CURVE('',#10038,#10036,#803,.T.);
#12664=EDGE_CURVE('',#10039,#10037,#804,.T.);
#12665=EDGE_CURVE('',#10039,#10040,#6080,.T.);
#12666=EDGE_CURVE('',#10040,#10038,#805,.T.);
#12667=EDGE_CURVE('',#10041,#10039,#806,.T.);
#12668=EDGE_CURVE('',#10041,#10042,#6081,.T.);
#12669=EDGE_CURVE('',#10042,#10040,#807,.T.);
#12670=EDGE_CURVE('',#10043,#10041,#808,.T.);
#12671=EDGE_CURVE('',#10043,#10044,#6082,.T.);
#12672=EDGE_CURVE('',#10044,#10042,#809,.T.);
#12673=EDGE_CURVE('',#10045,#10043,#810,.T.);
#12674=EDGE_CURVE('',#10045,#10046,#6083,.T.);
#12675=EDGE_CURVE('',#10046,#10044,#811,.T.);
#12676=EDGE_CURVE('',#10047,#10045,#812,.T.);
#12677=EDGE_CURVE('',#10047,#10048,#6084,.T.);
#12678=EDGE_CURVE('',#10048,#10046,#813,.T.);
#12679=EDGE_CURVE('',#10049,#10047,#814,.T.);
#12680=EDGE_CURVE('',#10049,#10050,#6085,.T.);
#12681=EDGE_CURVE('',#10050,#10048,#815,.T.);
#12682=EDGE_CURVE('',#10051,#10049,#816,.T.);
#12683=EDGE_CURVE('',#10051,#10052,#6086,.T.);
#12684=EDGE_CURVE('',#10052,#10050,#817,.T.);
#12685=EDGE_CURVE('',#10053,#10051,#818,.T.);
#12686=EDGE_CURVE('',#10053,#10054,#6087,.T.);
#12687=EDGE_CURVE('',#10054,#10052,#819,.T.);
#12688=EDGE_CURVE('',#10032,#10053,#820,.T.);
#12689=EDGE_CURVE('',#10034,#10054,#821,.T.);
#12690=EDGE_CURVE('',#10055,#10056,#822,.T.);
#12691=EDGE_CURVE('',#10055,#10057,#6088,.T.);
#12692=EDGE_CURVE('',#10057,#10058,#823,.T.);
#12693=EDGE_CURVE('',#10056,#10058,#6089,.T.);
#12694=EDGE_CURVE('',#10059,#10055,#824,.T.);
#12695=EDGE_CURVE('',#10059,#10060,#6090,.T.);
#12696=EDGE_CURVE('',#10060,#10057,#825,.T.);
#12697=EDGE_CURVE('',#10061,#10059,#6091,.T.);
#12698=EDGE_CURVE('',#10061,#10062,#6092,.T.);
#12699=EDGE_CURVE('',#10062,#10060,#6093,.T.);
#12700=EDGE_CURVE('',#10063,#10061,#826,.T.);
#12701=EDGE_CURVE('',#10063,#10064,#6094,.T.);
#12702=EDGE_CURVE('',#10064,#10062,#827,.T.);
#12703=EDGE_CURVE('',#10065,#10063,#828,.T.);
#12704=EDGE_CURVE('',#10065,#10066,#6095,.T.);
#12705=EDGE_CURVE('',#10066,#10064,#829,.T.);
#12706=EDGE_CURVE('',#10067,#10065,#6096,.T.);
#12707=EDGE_CURVE('',#10067,#10068,#6097,.T.);
#12708=EDGE_CURVE('',#10068,#10066,#6098,.T.);
#12709=EDGE_CURVE('',#10069,#10067,#6099,.T.);
#12710=EDGE_CURVE('',#10069,#10070,#6100,.T.);
#12711=EDGE_CURVE('',#10070,#10068,#6101,.T.);
#12712=EDGE_CURVE('',#10071,#10069,#6102,.T.);
#12713=EDGE_CURVE('',#10071,#10072,#6103,.T.);
#12714=EDGE_CURVE('',#10072,#10070,#6104,.T.);
#12715=EDGE_CURVE('',#10056,#10071,#6105,.T.);
#12716=EDGE_CURVE('',#10058,#10072,#6106,.T.);
#12717=EDGE_CURVE('',#10073,#10074,#6107,.T.);
#12718=EDGE_CURVE('',#10073,#10075,#6108,.T.);
#12719=EDGE_CURVE('',#10075,#10076,#6109,.T.);
#12720=EDGE_CURVE('',#10074,#10076,#6110,.T.);
#12721=EDGE_CURVE('',#10077,#10073,#6111,.T.);
#12722=EDGE_CURVE('',#10077,#10078,#6112,.T.);
#12723=EDGE_CURVE('',#10078,#10075,#6113,.T.);
#12724=EDGE_CURVE('',#10079,#10077,#6114,.T.);
#12725=EDGE_CURVE('',#10079,#10080,#6115,.T.);
#12726=EDGE_CURVE('',#10080,#10078,#6116,.T.);
#12727=EDGE_CURVE('',#10081,#10079,#6117,.T.);
#12728=EDGE_CURVE('',#10081,#10082,#6118,.T.);
#12729=EDGE_CURVE('',#10082,#10080,#6119,.T.);
#12730=EDGE_CURVE('',#10083,#10081,#6120,.T.);
#12731=EDGE_CURVE('',#10083,#10084,#6121,.T.);
#12732=EDGE_CURVE('',#10084,#10082,#6122,.T.);
#12733=EDGE_CURVE('',#10085,#10083,#6123,.T.);
#12734=EDGE_CURVE('',#10085,#10086,#6124,.T.);
#12735=EDGE_CURVE('',#10086,#10084,#6125,.T.);
#12736=EDGE_CURVE('',#10087,#10085,#6126,.T.);
#12737=EDGE_CURVE('',#10087,#10088,#6127,.T.);
#12738=EDGE_CURVE('',#10088,#10086,#6128,.T.);
#12739=EDGE_CURVE('',#10089,#10087,#6129,.T.);
#12740=EDGE_CURVE('',#10089,#10090,#6130,.T.);
#12741=EDGE_CURVE('',#10090,#10088,#6131,.T.);
#12742=EDGE_CURVE('',#10091,#10089,#830,.T.);
#12743=EDGE_CURVE('',#10091,#10092,#6132,.T.);
#12744=EDGE_CURVE('',#10092,#10090,#831,.T.);
#12745=EDGE_CURVE('',#10093,#10091,#832,.T.);
#12746=EDGE_CURVE('',#10093,#10094,#6133,.T.);
#12747=EDGE_CURVE('',#10094,#10092,#833,.T.);
#12748=EDGE_CURVE('',#10095,#10093,#6134,.T.);
#12749=EDGE_CURVE('',#10095,#10096,#6135,.T.);
#12750=EDGE_CURVE('',#10096,#10094,#6136,.T.);
#12751=EDGE_CURVE('',#10097,#10095,#6137,.T.);
#12752=EDGE_CURVE('',#10097,#10098,#6138,.T.);
#12753=EDGE_CURVE('',#10098,#10096,#6139,.T.);
#12754=EDGE_CURVE('',#10099,#10097,#6140,.T.);
#12755=EDGE_CURVE('',#10099,#10100,#6141,.T.);
#12756=EDGE_CURVE('',#10100,#10098,#6142,.T.);
#12757=EDGE_CURVE('',#10101,#10099,#6143,.T.);
#12758=EDGE_CURVE('',#10101,#10102,#6144,.T.);
#12759=EDGE_CURVE('',#10102,#10100,#6145,.T.);
#12760=EDGE_CURVE('',#10074,#10101,#6146,.T.);
#12761=EDGE_CURVE('',#10076,#10102,#6147,.T.);
#12762=EDGE_CURVE('',#10103,#10104,#834,.T.);
#12763=EDGE_CURVE('',#10103,#10105,#6148,.T.);
#12764=EDGE_CURVE('',#10105,#10106,#835,.T.);
#12765=EDGE_CURVE('',#10104,#10106,#6149,.T.);
#12766=EDGE_CURVE('',#10107,#10103,#836,.T.);
#12767=EDGE_CURVE('',#10107,#10108,#6150,.T.);
#12768=EDGE_CURVE('',#10108,#10105,#837,.T.);
#12769=EDGE_CURVE('',#10109,#10107,#838,.T.);
#12770=EDGE_CURVE('',#10109,#10110,#6151,.T.);
#12771=EDGE_CURVE('',#10110,#10108,#839,.T.);
#12772=EDGE_CURVE('',#10111,#10109,#840,.T.);
#12773=EDGE_CURVE('',#10111,#10112,#6152,.T.);
#12774=EDGE_CURVE('',#10112,#10110,#841,.T.);
#12775=EDGE_CURVE('',#10113,#10111,#842,.T.);
#12776=EDGE_CURVE('',#10113,#10114,#6153,.T.);
#12777=EDGE_CURVE('',#10114,#10112,#843,.T.);
#12778=EDGE_CURVE('',#10115,#10113,#844,.T.);
#12779=EDGE_CURVE('',#10115,#10116,#6154,.T.);
#12780=EDGE_CURVE('',#10116,#10114,#845,.T.);
#12781=EDGE_CURVE('',#10117,#10115,#846,.T.);
#12782=EDGE_CURVE('',#10117,#10118,#6155,.T.);
#12783=EDGE_CURVE('',#10118,#10116,#847,.T.);
#12784=EDGE_CURVE('',#10119,#10117,#848,.T.);
#12785=EDGE_CURVE('',#10119,#10120,#6156,.T.);
#12786=EDGE_CURVE('',#10120,#10118,#849,.T.);
#12787=EDGE_CURVE('',#10121,#10119,#850,.T.);
#12788=EDGE_CURVE('',#10121,#10122,#6157,.T.);
#12789=EDGE_CURVE('',#10122,#10120,#851,.T.);
#12790=EDGE_CURVE('',#10123,#10121,#852,.T.);
#12791=EDGE_CURVE('',#10123,#10124,#6158,.T.);
#12792=EDGE_CURVE('',#10124,#10122,#853,.T.);
#12793=EDGE_CURVE('',#10125,#10123,#854,.T.);
#12794=EDGE_CURVE('',#10125,#10126,#6159,.T.);
#12795=EDGE_CURVE('',#10126,#10124,#855,.T.);
#12796=EDGE_CURVE('',#10127,#10125,#6160,.T.);
#12797=EDGE_CURVE('',#10127,#10128,#6161,.T.);
#12798=EDGE_CURVE('',#10128,#10126,#6162,.T.);
#12799=EDGE_CURVE('',#10129,#10127,#856,.T.);
#12800=EDGE_CURVE('',#10129,#10130,#6163,.T.);
#12801=EDGE_CURVE('',#10130,#10128,#857,.T.);
#12802=EDGE_CURVE('',#10131,#10129,#858,.T.);
#12803=EDGE_CURVE('',#10131,#10132,#6164,.T.);
#12804=EDGE_CURVE('',#10132,#10130,#859,.T.);
#12805=EDGE_CURVE('',#10133,#10131,#860,.T.);
#12806=EDGE_CURVE('',#10133,#10134,#6165,.T.);
#12807=EDGE_CURVE('',#10134,#10132,#861,.T.);
#12808=EDGE_CURVE('',#10135,#10133,#862,.T.);
#12809=EDGE_CURVE('',#10135,#10136,#6166,.T.);
#12810=EDGE_CURVE('',#10136,#10134,#863,.T.);
#12811=EDGE_CURVE('',#10137,#10135,#864,.T.);
#12812=EDGE_CURVE('',#10137,#10138,#6167,.T.);
#12813=EDGE_CURVE('',#10138,#10136,#865,.T.);
#12814=EDGE_CURVE('',#10139,#10137,#866,.T.);
#12815=EDGE_CURVE('',#10139,#10140,#6168,.T.);
#12816=EDGE_CURVE('',#10140,#10138,#867,.T.);
#12817=EDGE_CURVE('',#10141,#10139,#868,.T.);
#12818=EDGE_CURVE('',#10141,#10142,#6169,.T.);
#12819=EDGE_CURVE('',#10142,#10140,#869,.T.);
#12820=EDGE_CURVE('',#10143,#10141,#6170,.T.);
#12821=EDGE_CURVE('',#10143,#10144,#6171,.T.);
#12822=EDGE_CURVE('',#10144,#10142,#6172,.T.);
#12823=EDGE_CURVE('',#10145,#10143,#870,.T.);
#12824=EDGE_CURVE('',#10145,#10146,#6173,.T.);
#12825=EDGE_CURVE('',#10146,#10144,#871,.T.);
#12826=EDGE_CURVE('',#10147,#10145,#872,.T.);
#12827=EDGE_CURVE('',#10147,#10148,#6174,.T.);
#12828=EDGE_CURVE('',#10148,#10146,#873,.T.);
#12829=EDGE_CURVE('',#10149,#10147,#874,.T.);
#12830=EDGE_CURVE('',#10149,#10150,#6175,.T.);
#12831=EDGE_CURVE('',#10150,#10148,#875,.T.);
#12832=EDGE_CURVE('',#10151,#10149,#876,.T.);
#12833=EDGE_CURVE('',#10151,#10152,#6176,.T.);
#12834=EDGE_CURVE('',#10152,#10150,#877,.T.);
#12835=EDGE_CURVE('',#10153,#10151,#878,.T.);
#12836=EDGE_CURVE('',#10153,#10154,#6177,.T.);
#12837=EDGE_CURVE('',#10154,#10152,#879,.T.);
#12838=EDGE_CURVE('',#10155,#10153,#880,.T.);
#12839=EDGE_CURVE('',#10155,#10156,#6178,.T.);
#12840=EDGE_CURVE('',#10156,#10154,#881,.T.);
#12841=EDGE_CURVE('',#10157,#10155,#882,.T.);
#12842=EDGE_CURVE('',#10157,#10158,#6179,.T.);
#12843=EDGE_CURVE('',#10158,#10156,#883,.T.);
#12844=EDGE_CURVE('',#10159,#10157,#6180,.T.);
#12845=EDGE_CURVE('',#10159,#10160,#6181,.T.);
#12846=EDGE_CURVE('',#10160,#10158,#6182,.T.);
#12847=EDGE_CURVE('',#10161,#10159,#884,.T.);
#12848=EDGE_CURVE('',#10161,#10162,#6183,.T.);
#12849=EDGE_CURVE('',#10162,#10160,#885,.T.);
#12850=EDGE_CURVE('',#10104,#10161,#886,.T.);
#12851=EDGE_CURVE('',#10106,#10162,#887,.T.);
#12852=EDGE_CURVE('',#10163,#10164,#6184,.T.);
#12853=EDGE_CURVE('',#10163,#10165,#6185,.T.);
#12854=EDGE_CURVE('',#10165,#10166,#6186,.T.);
#12855=EDGE_CURVE('',#10164,#10166,#6187,.T.);
#12856=EDGE_CURVE('',#10167,#10163,#6188,.T.);
#12857=EDGE_CURVE('',#10167,#10168,#6189,.T.);
#12858=EDGE_CURVE('',#10168,#10165,#6190,.T.);
#12859=EDGE_CURVE('',#10169,#10167,#6191,.T.);
#12860=EDGE_CURVE('',#10169,#10170,#6192,.T.);
#12861=EDGE_CURVE('',#10170,#10168,#6193,.T.);
#12862=EDGE_CURVE('',#10164,#10169,#6194,.T.);
#12863=EDGE_CURVE('',#10166,#10170,#6195,.T.);
#12864=EDGE_CURVE('',#10171,#10172,#888,.T.);
#12865=EDGE_CURVE('',#10171,#10173,#6196,.T.);
#12866=EDGE_CURVE('',#10173,#10174,#889,.T.);
#12867=EDGE_CURVE('',#10172,#10174,#6197,.T.);
#12868=EDGE_CURVE('',#10175,#10171,#890,.T.);
#12869=EDGE_CURVE('',#10175,#10176,#6198,.T.);
#12870=EDGE_CURVE('',#10176,#10173,#891,.T.);
#12871=EDGE_CURVE('',#10177,#10175,#6199,.T.);
#12872=EDGE_CURVE('',#10177,#10178,#6200,.T.);
#12873=EDGE_CURVE('',#10178,#10176,#6201,.T.);
#12874=EDGE_CURVE('',#10179,#10177,#6202,.T.);
#12875=EDGE_CURVE('',#10179,#10180,#6203,.T.);
#12876=EDGE_CURVE('',#10180,#10178,#6204,.T.);
#12877=EDGE_CURVE('',#10172,#10179,#6205,.T.);
#12878=EDGE_CURVE('',#10174,#10180,#6206,.T.);
#12879=EDGE_CURVE('',#10181,#10182,#6207,.T.);
#12880=EDGE_CURVE('',#10181,#10183,#6208,.T.);
#12881=EDGE_CURVE('',#10183,#10184,#6209,.T.);
#12882=EDGE_CURVE('',#10182,#10184,#6210,.T.);
#12883=EDGE_CURVE('',#10185,#10181,#6211,.T.);
#12884=EDGE_CURVE('',#10185,#10186,#6212,.T.);
#12885=EDGE_CURVE('',#10186,#10183,#6213,.T.);
#12886=EDGE_CURVE('',#10187,#10185,#6214,.T.);
#12887=EDGE_CURVE('',#10187,#10188,#6215,.T.);
#12888=EDGE_CURVE('',#10188,#10186,#6216,.T.);
#12889=EDGE_CURVE('',#10189,#10187,#6217,.T.);
#12890=EDGE_CURVE('',#10189,#10190,#6218,.T.);
#12891=EDGE_CURVE('',#10190,#10188,#6219,.T.);
#12892=EDGE_CURVE('',#10191,#10189,#6220,.T.);
#12893=EDGE_CURVE('',#10191,#10192,#6221,.T.);
#12894=EDGE_CURVE('',#10192,#10190,#6222,.T.);
#12895=EDGE_CURVE('',#10193,#10191,#6223,.T.);
#12896=EDGE_CURVE('',#10193,#10194,#6224,.T.);
#12897=EDGE_CURVE('',#10194,#10192,#6225,.T.);
#12898=EDGE_CURVE('',#10195,#10193,#6226,.T.);
#12899=EDGE_CURVE('',#10195,#10196,#6227,.T.);
#12900=EDGE_CURVE('',#10196,#10194,#6228,.T.);
#12901=EDGE_CURVE('',#10182,#10195,#6229,.T.);
#12902=EDGE_CURVE('',#10184,#10196,#6230,.T.);
#12903=EDGE_CURVE('',#10197,#10198,#892,.T.);
#12904=EDGE_CURVE('',#10197,#10199,#6231,.T.);
#12905=EDGE_CURVE('',#10199,#10200,#893,.T.);
#12906=EDGE_CURVE('',#10198,#10200,#6232,.T.);
#12907=EDGE_CURVE('',#10201,#10197,#894,.T.);
#12908=EDGE_CURVE('',#10201,#10202,#6233,.T.);
#12909=EDGE_CURVE('',#10202,#10199,#895,.T.);
#12910=EDGE_CURVE('',#10203,#10201,#896,.T.);
#12911=EDGE_CURVE('',#10203,#10204,#6234,.T.);
#12912=EDGE_CURVE('',#10204,#10202,#897,.T.);
#12913=EDGE_CURVE('',#10205,#10203,#898,.T.);
#12914=EDGE_CURVE('',#10205,#10206,#6235,.T.);
#12915=EDGE_CURVE('',#10206,#10204,#899,.T.);
#12916=EDGE_CURVE('',#10207,#10205,#900,.T.);
#12917=EDGE_CURVE('',#10207,#10208,#6236,.T.);
#12918=EDGE_CURVE('',#10208,#10206,#901,.T.);
#12919=EDGE_CURVE('',#10209,#10207,#902,.T.);
#12920=EDGE_CURVE('',#10209,#10210,#6237,.T.);
#12921=EDGE_CURVE('',#10210,#10208,#903,.T.);
#12922=EDGE_CURVE('',#10211,#10209,#904,.T.);
#12923=EDGE_CURVE('',#10211,#10212,#6238,.T.);
#12924=EDGE_CURVE('',#10212,#10210,#905,.T.);
#12925=EDGE_CURVE('',#10213,#10211,#906,.T.);
#12926=EDGE_CURVE('',#10213,#10214,#6239,.T.);
#12927=EDGE_CURVE('',#10214,#10212,#907,.T.);
#12928=EDGE_CURVE('',#10215,#10213,#908,.T.);
#12929=EDGE_CURVE('',#10215,#10216,#6240,.T.);
#12930=EDGE_CURVE('',#10216,#10214,#909,.T.);
#12931=EDGE_CURVE('',#10217,#10215,#910,.T.);
#12932=EDGE_CURVE('',#10217,#10218,#6241,.T.);
#12933=EDGE_CURVE('',#10218,#10216,#911,.T.);
#12934=EDGE_CURVE('',#10219,#10217,#912,.T.);
#12935=EDGE_CURVE('',#10219,#10220,#6242,.T.);
#12936=EDGE_CURVE('',#10220,#10218,#913,.T.);
#12937=EDGE_CURVE('',#10221,#10219,#914,.T.);
#12938=EDGE_CURVE('',#10221,#10222,#6243,.T.);
#12939=EDGE_CURVE('',#10222,#10220,#915,.T.);
#12940=EDGE_CURVE('',#10223,#10221,#916,.T.);
#12941=EDGE_CURVE('',#10223,#10224,#6244,.T.);
#12942=EDGE_CURVE('',#10224,#10222,#917,.T.);
#12943=EDGE_CURVE('',#10225,#10223,#6245,.T.);
#12944=EDGE_CURVE('',#10225,#10226,#6246,.T.);
#12945=EDGE_CURVE('',#10226,#10224,#6247,.T.);
#12946=EDGE_CURVE('',#10227,#10225,#918,.T.);
#12947=EDGE_CURVE('',#10227,#10228,#6248,.T.);
#12948=EDGE_CURVE('',#10228,#10226,#919,.T.);
#12949=EDGE_CURVE('',#10229,#10227,#920,.T.);
#12950=EDGE_CURVE('',#10229,#10230,#6249,.T.);
#12951=EDGE_CURVE('',#10230,#10228,#921,.T.);
#12952=EDGE_CURVE('',#10231,#10229,#922,.T.);
#12953=EDGE_CURVE('',#10231,#10232,#6250,.T.);
#12954=EDGE_CURVE('',#10232,#10230,#923,.T.);
#12955=EDGE_CURVE('',#10233,#10231,#924,.T.);
#12956=EDGE_CURVE('',#10233,#10234,#6251,.T.);
#12957=EDGE_CURVE('',#10234,#10232,#925,.T.);
#12958=EDGE_CURVE('',#10235,#10233,#926,.T.);
#12959=EDGE_CURVE('',#10235,#10236,#6252,.T.);
#12960=EDGE_CURVE('',#10236,#10234,#927,.T.);
#12961=EDGE_CURVE('',#10237,#10235,#928,.T.);
#12962=EDGE_CURVE('',#10237,#10238,#6253,.T.);
#12963=EDGE_CURVE('',#10238,#10236,#929,.T.);
#12964=EDGE_CURVE('',#10239,#10237,#930,.T.);
#12965=EDGE_CURVE('',#10239,#10240,#6254,.T.);
#12966=EDGE_CURVE('',#10240,#10238,#931,.T.);
#12967=EDGE_CURVE('',#10241,#10239,#932,.T.);
#12968=EDGE_CURVE('',#10241,#10242,#6255,.T.);
#12969=EDGE_CURVE('',#10242,#10240,#933,.T.);
#12970=EDGE_CURVE('',#10243,#10241,#934,.T.);
#12971=EDGE_CURVE('',#10243,#10244,#6256,.T.);
#12972=EDGE_CURVE('',#10244,#10242,#935,.T.);
#12973=EDGE_CURVE('',#10245,#10243,#936,.T.);
#12974=EDGE_CURVE('',#10245,#10246,#6257,.T.);
#12975=EDGE_CURVE('',#10246,#10244,#937,.T.);
#12976=EDGE_CURVE('',#10247,#10245,#938,.T.);
#12977=EDGE_CURVE('',#10247,#10248,#6258,.T.);
#12978=EDGE_CURVE('',#10248,#10246,#939,.T.);
#12979=EDGE_CURVE('',#10249,#10247,#940,.T.);
#12980=EDGE_CURVE('',#10249,#10250,#6259,.T.);
#12981=EDGE_CURVE('',#10250,#10248,#941,.T.);
#12982=EDGE_CURVE('',#10251,#10249,#942,.T.);
#12983=EDGE_CURVE('',#10251,#10252,#6260,.T.);
#12984=EDGE_CURVE('',#10252,#10250,#943,.T.);
#12985=EDGE_CURVE('',#10253,#10251,#944,.T.);
#12986=EDGE_CURVE('',#10253,#10254,#6261,.T.);
#12987=EDGE_CURVE('',#10254,#10252,#945,.T.);
#12988=EDGE_CURVE('',#10255,#10253,#946,.T.);
#12989=EDGE_CURVE('',#10255,#10256,#6262,.T.);
#12990=EDGE_CURVE('',#10256,#10254,#947,.T.);
#12991=EDGE_CURVE('',#10257,#10255,#948,.T.);
#12992=EDGE_CURVE('',#10257,#10258,#6263,.T.);
#12993=EDGE_CURVE('',#10258,#10256,#949,.T.);
#12994=EDGE_CURVE('',#10259,#10257,#950,.T.);
#12995=EDGE_CURVE('',#10259,#10260,#6264,.T.);
#12996=EDGE_CURVE('',#10260,#10258,#951,.T.);
#12997=EDGE_CURVE('',#10261,#10259,#952,.T.);
#12998=EDGE_CURVE('',#10261,#10262,#6265,.T.);
#12999=EDGE_CURVE('',#10262,#10260,#953,.T.);
#13000=EDGE_CURVE('',#10263,#10261,#6266,.T.);
#13001=EDGE_CURVE('',#10263,#10264,#6267,.T.);
#13002=EDGE_CURVE('',#10264,#10262,#6268,.T.);
#13003=EDGE_CURVE('',#10265,#10263,#954,.T.);
#13004=EDGE_CURVE('',#10265,#10266,#6269,.T.);
#13005=EDGE_CURVE('',#10266,#10264,#955,.T.);
#13006=EDGE_CURVE('',#10198,#10265,#956,.T.);
#13007=EDGE_CURVE('',#10200,#10266,#957,.T.);
#13008=EDGE_CURVE('',#10267,#10268,#958,.T.);
#13009=EDGE_CURVE('',#10267,#10269,#6270,.T.);
#13010=EDGE_CURVE('',#10269,#10270,#959,.T.);
#13011=EDGE_CURVE('',#10268,#10270,#6271,.T.);
#13012=EDGE_CURVE('',#10271,#10267,#960,.T.);
#13013=EDGE_CURVE('',#10271,#10272,#6272,.T.);
#13014=EDGE_CURVE('',#10272,#10269,#961,.T.);
#13015=EDGE_CURVE('',#10273,#10271,#962,.T.);
#13016=EDGE_CURVE('',#10273,#10274,#6273,.T.);
#13017=EDGE_CURVE('',#10274,#10272,#963,.T.);
#13018=EDGE_CURVE('',#10275,#10273,#964,.T.);
#13019=EDGE_CURVE('',#10275,#10276,#6274,.T.);
#13020=EDGE_CURVE('',#10276,#10274,#965,.T.);
#13021=EDGE_CURVE('',#10277,#10275,#966,.T.);
#13022=EDGE_CURVE('',#10277,#10278,#6275,.T.);
#13023=EDGE_CURVE('',#10278,#10276,#967,.T.);
#13024=EDGE_CURVE('',#10279,#10277,#968,.T.);
#13025=EDGE_CURVE('',#10279,#10280,#6276,.T.);
#13026=EDGE_CURVE('',#10280,#10278,#969,.T.);
#13027=EDGE_CURVE('',#10281,#10279,#970,.T.);
#13028=EDGE_CURVE('',#10281,#10282,#6277,.T.);
#13029=EDGE_CURVE('',#10282,#10280,#971,.T.);
#13030=EDGE_CURVE('',#10283,#10281,#972,.T.);
#13031=EDGE_CURVE('',#10283,#10284,#6278,.T.);
#13032=EDGE_CURVE('',#10284,#10282,#973,.T.);
#13033=EDGE_CURVE('',#10285,#10283,#974,.T.);
#13034=EDGE_CURVE('',#10285,#10286,#6279,.T.);
#13035=EDGE_CURVE('',#10286,#10284,#975,.T.);
#13036=EDGE_CURVE('',#10287,#10285,#976,.T.);
#13037=EDGE_CURVE('',#10287,#10288,#6280,.T.);
#13038=EDGE_CURVE('',#10288,#10286,#977,.T.);
#13039=EDGE_CURVE('',#10289,#10287,#978,.T.);
#13040=EDGE_CURVE('',#10289,#10290,#6281,.T.);
#13041=EDGE_CURVE('',#10290,#10288,#979,.T.);
#13042=EDGE_CURVE('',#10291,#10289,#6282,.T.);
#13043=EDGE_CURVE('',#10291,#10292,#6283,.T.);
#13044=EDGE_CURVE('',#10292,#10290,#6284,.T.);
#13045=EDGE_CURVE('',#10293,#10291,#980,.T.);
#13046=EDGE_CURVE('',#10293,#10294,#6285,.T.);
#13047=EDGE_CURVE('',#10294,#10292,#981,.T.);
#13048=EDGE_CURVE('',#10295,#10293,#982,.T.);
#13049=EDGE_CURVE('',#10295,#10296,#6286,.T.);
#13050=EDGE_CURVE('',#10296,#10294,#983,.T.);
#13051=EDGE_CURVE('',#10297,#10295,#984,.T.);
#13052=EDGE_CURVE('',#10297,#10298,#6287,.T.);
#13053=EDGE_CURVE('',#10298,#10296,#985,.T.);
#13054=EDGE_CURVE('',#10299,#10297,#986,.T.);
#13055=EDGE_CURVE('',#10299,#10300,#6288,.T.);
#13056=EDGE_CURVE('',#10300,#10298,#987,.T.);
#13057=EDGE_CURVE('',#10301,#10299,#988,.T.);
#13058=EDGE_CURVE('',#10301,#10302,#6289,.T.);
#13059=EDGE_CURVE('',#10302,#10300,#989,.T.);
#13060=EDGE_CURVE('',#10303,#10301,#990,.T.);
#13061=EDGE_CURVE('',#10303,#10304,#6290,.T.);
#13062=EDGE_CURVE('',#10304,#10302,#991,.T.);
#13063=EDGE_CURVE('',#10305,#10303,#992,.T.);
#13064=EDGE_CURVE('',#10305,#10306,#6291,.T.);
#13065=EDGE_CURVE('',#10306,#10304,#993,.T.);
#13066=EDGE_CURVE('',#10307,#10305,#6292,.T.);
#13067=EDGE_CURVE('',#10307,#10308,#6293,.T.);
#13068=EDGE_CURVE('',#10308,#10306,#6294,.T.);
#13069=EDGE_CURVE('',#10309,#10307,#994,.T.);
#13070=EDGE_CURVE('',#10309,#10310,#6295,.T.);
#13071=EDGE_CURVE('',#10310,#10308,#995,.T.);
#13072=EDGE_CURVE('',#10311,#10309,#996,.T.);
#13073=EDGE_CURVE('',#10311,#10312,#6296,.T.);
#13074=EDGE_CURVE('',#10312,#10310,#997,.T.);
#13075=EDGE_CURVE('',#10313,#10311,#998,.T.);
#13076=EDGE_CURVE('',#10313,#10314,#6297,.T.);
#13077=EDGE_CURVE('',#10314,#10312,#999,.T.);
#13078=EDGE_CURVE('',#10315,#10313,#1000,.T.);
#13079=EDGE_CURVE('',#10315,#10316,#6298,.T.);
#13080=EDGE_CURVE('',#10316,#10314,#1001,.T.);
#13081=EDGE_CURVE('',#10317,#10315,#1002,.T.);
#13082=EDGE_CURVE('',#10317,#10318,#6299,.T.);
#13083=EDGE_CURVE('',#10318,#10316,#1003,.T.);
#13084=EDGE_CURVE('',#10319,#10317,#1004,.T.);
#13085=EDGE_CURVE('',#10319,#10320,#6300,.T.);
#13086=EDGE_CURVE('',#10320,#10318,#1005,.T.);
#13087=EDGE_CURVE('',#10321,#10319,#1006,.T.);
#13088=EDGE_CURVE('',#10321,#10322,#6301,.T.);
#13089=EDGE_CURVE('',#10322,#10320,#1007,.T.);
#13090=EDGE_CURVE('',#10323,#10321,#6302,.T.);
#13091=EDGE_CURVE('',#10323,#10324,#6303,.T.);
#13092=EDGE_CURVE('',#10324,#10322,#6304,.T.);
#13093=EDGE_CURVE('',#10325,#10323,#1008,.T.);
#13094=EDGE_CURVE('',#10325,#10326,#6305,.T.);
#13095=EDGE_CURVE('',#10326,#10324,#1009,.T.);
#13096=EDGE_CURVE('',#10268,#10325,#1010,.T.);
#13097=EDGE_CURVE('',#10270,#10326,#1011,.T.);
#13098=EDGE_CURVE('',#10327,#10328,#1012,.T.);
#13099=EDGE_CURVE('',#10327,#10329,#6306,.T.);
#13100=EDGE_CURVE('',#10329,#10330,#1013,.T.);
#13101=EDGE_CURVE('',#10328,#10330,#6307,.T.);
#13102=EDGE_CURVE('',#10331,#10327,#1014,.T.);
#13103=EDGE_CURVE('',#10331,#10332,#6308,.T.);
#13104=EDGE_CURVE('',#10332,#10329,#1015,.T.);
#13105=EDGE_CURVE('',#10333,#10331,#1016,.T.);
#13106=EDGE_CURVE('',#10333,#10334,#6309,.T.);
#13107=EDGE_CURVE('',#10334,#10332,#1017,.T.);
#13108=EDGE_CURVE('',#10335,#10333,#1018,.T.);
#13109=EDGE_CURVE('',#10335,#10336,#6310,.T.);
#13110=EDGE_CURVE('',#10336,#10334,#1019,.T.);
#13111=EDGE_CURVE('',#10337,#10335,#1020,.T.);
#13112=EDGE_CURVE('',#10337,#10338,#6311,.T.);
#13113=EDGE_CURVE('',#10338,#10336,#1021,.T.);
#13114=EDGE_CURVE('',#10339,#10337,#1022,.T.);
#13115=EDGE_CURVE('',#10339,#10340,#6312,.T.);
#13116=EDGE_CURVE('',#10340,#10338,#1023,.T.);
#13117=EDGE_CURVE('',#10341,#10339,#1024,.T.);
#13118=EDGE_CURVE('',#10341,#10342,#6313,.T.);
#13119=EDGE_CURVE('',#10342,#10340,#1025,.T.);
#13120=EDGE_CURVE('',#10343,#10341,#1026,.T.);
#13121=EDGE_CURVE('',#10343,#10344,#6314,.T.);
#13122=EDGE_CURVE('',#10344,#10342,#1027,.T.);
#13123=EDGE_CURVE('',#10345,#10343,#6315,.T.);
#13124=EDGE_CURVE('',#10345,#10346,#6316,.T.);
#13125=EDGE_CURVE('',#10346,#10344,#6317,.T.);
#13126=EDGE_CURVE('',#10347,#10345,#1028,.T.);
#13127=EDGE_CURVE('',#10347,#10348,#6318,.T.);
#13128=EDGE_CURVE('',#10348,#10346,#1029,.T.);
#13129=EDGE_CURVE('',#10349,#10347,#1030,.T.);
#13130=EDGE_CURVE('',#10349,#10350,#6319,.T.);
#13131=EDGE_CURVE('',#10350,#10348,#1031,.T.);
#13132=EDGE_CURVE('',#10351,#10349,#1032,.T.);
#13133=EDGE_CURVE('',#10351,#10352,#6320,.T.);
#13134=EDGE_CURVE('',#10352,#10350,#1033,.T.);
#13135=EDGE_CURVE('',#10353,#10351,#1034,.T.);
#13136=EDGE_CURVE('',#10353,#10354,#6321,.T.);
#13137=EDGE_CURVE('',#10354,#10352,#1035,.T.);
#13138=EDGE_CURVE('',#10355,#10353,#1036,.T.);
#13139=EDGE_CURVE('',#10355,#10356,#6322,.T.);
#13140=EDGE_CURVE('',#10356,#10354,#1037,.T.);
#13141=EDGE_CURVE('',#10357,#10355,#1038,.T.);
#13142=EDGE_CURVE('',#10357,#10358,#6323,.T.);
#13143=EDGE_CURVE('',#10358,#10356,#1039,.T.);
#13144=EDGE_CURVE('',#10359,#10357,#1040,.T.);
#13145=EDGE_CURVE('',#10359,#10360,#6324,.T.);
#13146=EDGE_CURVE('',#10360,#10358,#1041,.T.);
#13147=EDGE_CURVE('',#10361,#10359,#1042,.T.);
#13148=EDGE_CURVE('',#10361,#10362,#6325,.T.);
#13149=EDGE_CURVE('',#10362,#10360,#1043,.T.);
#13150=EDGE_CURVE('',#10363,#10361,#1044,.T.);
#13151=EDGE_CURVE('',#10363,#10364,#6326,.T.);
#13152=EDGE_CURVE('',#10364,#10362,#1045,.T.);
#13153=EDGE_CURVE('',#10365,#10363,#6327,.T.);
#13154=EDGE_CURVE('',#10365,#10366,#6328,.T.);
#13155=EDGE_CURVE('',#10366,#10364,#6329,.T.);
#13156=EDGE_CURVE('',#10367,#10365,#6330,.T.);
#13157=EDGE_CURVE('',#10367,#10368,#6331,.T.);
#13158=EDGE_CURVE('',#10368,#10366,#6332,.T.);
#13159=EDGE_CURVE('',#10369,#10367,#6333,.T.);
#13160=EDGE_CURVE('',#10369,#10370,#6334,.T.);
#13161=EDGE_CURVE('',#10370,#10368,#6335,.T.);
#13162=EDGE_CURVE('',#10328,#10369,#1046,.T.);
#13163=EDGE_CURVE('',#10330,#10370,#1047,.T.);
#13164=EDGE_CURVE('',#10371,#10372,#6336,.T.);
#13165=EDGE_CURVE('',#10371,#10373,#6337,.T.);
#13166=EDGE_CURVE('',#10373,#10374,#6338,.T.);
#13167=EDGE_CURVE('',#10372,#10374,#6339,.T.);
#13168=EDGE_CURVE('',#10375,#10371,#1048,.T.);
#13169=EDGE_CURVE('',#10375,#10376,#6340,.T.);
#13170=EDGE_CURVE('',#10376,#10373,#1049,.T.);
#13171=EDGE_CURVE('',#10377,#10375,#1050,.T.);
#13172=EDGE_CURVE('',#10377,#10378,#6341,.T.);
#13173=EDGE_CURVE('',#10378,#10376,#1051,.T.);
#13174=EDGE_CURVE('',#10379,#10377,#1052,.T.);
#13175=EDGE_CURVE('',#10379,#10380,#6342,.T.);
#13176=EDGE_CURVE('',#10380,#10378,#1053,.T.);
#13177=EDGE_CURVE('',#10381,#10379,#1054,.T.);
#13178=EDGE_CURVE('',#10381,#10382,#6343,.T.);
#13179=EDGE_CURVE('',#10382,#10380,#1055,.T.);
#13180=EDGE_CURVE('',#10383,#10381,#1056,.T.);
#13181=EDGE_CURVE('',#10383,#10384,#6344,.T.);
#13182=EDGE_CURVE('',#10384,#10382,#1057,.T.);
#13183=EDGE_CURVE('',#10385,#10383,#6345,.T.);
#13184=EDGE_CURVE('',#10385,#10386,#6346,.T.);
#13185=EDGE_CURVE('',#10386,#10384,#6347,.T.);
#13186=EDGE_CURVE('',#10372,#10385,#6348,.T.);
#13187=EDGE_CURVE('',#10374,#10386,#6349,.T.);
#13188=EDGE_CURVE('',#10387,#10388,#6350,.T.);
#13189=EDGE_CURVE('',#10387,#10389,#6351,.T.);
#13190=EDGE_CURVE('',#10389,#10390,#6352,.T.);
#13191=EDGE_CURVE('',#10388,#10390,#6353,.T.);
#13192=EDGE_CURVE('',#10391,#10387,#1058,.T.);
#13193=EDGE_CURVE('',#10391,#10392,#6354,.T.);
#13194=EDGE_CURVE('',#10392,#10389,#1059,.T.);
#13195=EDGE_CURVE('',#10393,#10391,#1060,.T.);
#13196=EDGE_CURVE('',#10393,#10394,#6355,.T.);
#13197=EDGE_CURVE('',#10394,#10392,#1061,.T.);
#13198=EDGE_CURVE('',#10395,#10393,#1062,.T.);
#13199=EDGE_CURVE('',#10395,#10396,#6356,.T.);
#13200=EDGE_CURVE('',#10396,#10394,#1063,.T.);
#13201=EDGE_CURVE('',#10397,#10395,#1064,.T.);
#13202=EDGE_CURVE('',#10397,#10398,#6357,.T.);
#13203=EDGE_CURVE('',#10398,#10396,#1065,.T.);
#13204=EDGE_CURVE('',#10399,#10397,#1066,.T.);
#13205=EDGE_CURVE('',#10399,#10400,#6358,.T.);
#13206=EDGE_CURVE('',#10400,#10398,#1067,.T.);
#13207=EDGE_CURVE('',#10401,#10399,#1068,.T.);
#13208=EDGE_CURVE('',#10401,#10402,#6359,.T.);
#13209=EDGE_CURVE('',#10402,#10400,#1069,.T.);
#13210=EDGE_CURVE('',#10403,#10401,#6360,.T.);
#13211=EDGE_CURVE('',#10403,#10404,#6361,.T.);
#13212=EDGE_CURVE('',#10404,#10402,#6362,.T.);
#13213=EDGE_CURVE('',#10405,#10403,#6363,.T.);
#13214=EDGE_CURVE('',#10405,#10406,#6364,.T.);
#13215=EDGE_CURVE('',#10406,#10404,#6365,.T.);
#13216=EDGE_CURVE('',#10407,#10405,#6366,.T.);
#13217=EDGE_CURVE('',#10407,#10408,#6367,.T.);
#13218=EDGE_CURVE('',#10408,#10406,#6368,.T.);
#13219=EDGE_CURVE('',#10388,#10407,#6369,.T.);
#13220=EDGE_CURVE('',#10390,#10408,#6370,.T.);
#13221=EDGE_CURVE('',#10409,#10410,#1070,.T.);
#13222=EDGE_CURVE('',#10409,#10411,#6371,.T.);
#13223=EDGE_CURVE('',#10411,#10412,#1071,.T.);
#13224=EDGE_CURVE('',#10410,#10412,#6372,.T.);
#13225=EDGE_CURVE('',#10413,#10409,#1072,.T.);
#13226=EDGE_CURVE('',#10413,#10414,#6373,.T.);
#13227=EDGE_CURVE('',#10414,#10411,#1073,.T.);
#13228=EDGE_CURVE('',#10415,#10413,#1074,.T.);
#13229=EDGE_CURVE('',#10415,#10416,#6374,.T.);
#13230=EDGE_CURVE('',#10416,#10414,#1075,.T.);
#13231=EDGE_CURVE('',#10417,#10415,#1076,.T.);
#13232=EDGE_CURVE('',#10417,#10418,#6375,.T.);
#13233=EDGE_CURVE('',#10418,#10416,#1077,.T.);
#13234=EDGE_CURVE('',#10419,#10417,#1078,.T.);
#13235=EDGE_CURVE('',#10419,#10420,#6376,.T.);
#13236=EDGE_CURVE('',#10420,#10418,#1079,.T.);
#13237=EDGE_CURVE('',#10421,#10419,#1080,.T.);
#13238=EDGE_CURVE('',#10421,#10422,#6377,.T.);
#13239=EDGE_CURVE('',#10422,#10420,#1081,.T.);
#13240=EDGE_CURVE('',#10423,#10421,#1082,.T.);
#13241=EDGE_CURVE('',#10423,#10424,#6378,.T.);
#13242=EDGE_CURVE('',#10424,#10422,#1083,.T.);
#13243=EDGE_CURVE('',#10425,#10423,#1084,.T.);
#13244=EDGE_CURVE('',#10425,#10426,#6379,.T.);
#13245=EDGE_CURVE('',#10426,#10424,#1085,.T.);
#13246=EDGE_CURVE('',#10410,#10425,#1086,.T.);
#13247=EDGE_CURVE('',#10412,#10426,#1087,.T.);
#13248=EDGE_CURVE('',#10427,#10428,#1088,.T.);
#13249=EDGE_CURVE('',#10427,#10429,#6380,.T.);
#13250=EDGE_CURVE('',#10429,#10430,#1089,.T.);
#13251=EDGE_CURVE('',#10428,#10430,#6381,.T.);
#13252=EDGE_CURVE('',#10431,#10427,#1090,.T.);
#13253=EDGE_CURVE('',#10431,#10432,#6382,.T.);
#13254=EDGE_CURVE('',#10432,#10429,#1091,.T.);
#13255=EDGE_CURVE('',#10433,#10431,#1092,.T.);
#13256=EDGE_CURVE('',#10433,#10434,#6383,.T.);
#13257=EDGE_CURVE('',#10434,#10432,#1093,.T.);
#13258=EDGE_CURVE('',#10435,#10433,#1094,.T.);
#13259=EDGE_CURVE('',#10435,#10436,#6384,.T.);
#13260=EDGE_CURVE('',#10436,#10434,#1095,.T.);
#13261=EDGE_CURVE('',#10437,#10435,#1096,.T.);
#13262=EDGE_CURVE('',#10437,#10438,#6385,.T.);
#13263=EDGE_CURVE('',#10438,#10436,#1097,.T.);
#13264=EDGE_CURVE('',#10439,#10437,#1098,.T.);
#13265=EDGE_CURVE('',#10439,#10440,#6386,.T.);
#13266=EDGE_CURVE('',#10440,#10438,#1099,.T.);
#13267=EDGE_CURVE('',#10441,#10439,#1100,.T.);
#13268=EDGE_CURVE('',#10441,#10442,#6387,.T.);
#13269=EDGE_CURVE('',#10442,#10440,#1101,.T.);
#13270=EDGE_CURVE('',#10443,#10441,#1102,.T.);
#13271=EDGE_CURVE('',#10443,#10444,#6388,.T.);
#13272=EDGE_CURVE('',#10444,#10442,#1103,.T.);
#13273=EDGE_CURVE('',#10445,#10443,#1104,.T.);
#13274=EDGE_CURVE('',#10445,#10446,#6389,.T.);
#13275=EDGE_CURVE('',#10446,#10444,#1105,.T.);
#13276=EDGE_CURVE('',#10447,#10445,#1106,.T.);
#13277=EDGE_CURVE('',#10447,#10448,#6390,.T.);
#13278=EDGE_CURVE('',#10448,#10446,#1107,.T.);
#13279=EDGE_CURVE('',#10449,#10447,#1108,.T.);
#13280=EDGE_CURVE('',#10449,#10450,#6391,.T.);
#13281=EDGE_CURVE('',#10450,#10448,#1109,.T.);
#13282=EDGE_CURVE('',#10451,#10449,#1110,.T.);
#13283=EDGE_CURVE('',#10451,#10452,#6392,.T.);
#13284=EDGE_CURVE('',#10452,#10450,#1111,.T.);
#13285=EDGE_CURVE('',#10453,#10451,#1112,.T.);
#13286=EDGE_CURVE('',#10453,#10454,#6393,.T.);
#13287=EDGE_CURVE('',#10454,#10452,#1113,.T.);
#13288=EDGE_CURVE('',#10455,#10453,#1114,.T.);
#13289=EDGE_CURVE('',#10455,#10456,#6394,.T.);
#13290=EDGE_CURVE('',#10456,#10454,#1115,.T.);
#13291=EDGE_CURVE('',#10457,#10455,#1116,.T.);
#13292=EDGE_CURVE('',#10457,#10458,#6395,.T.);
#13293=EDGE_CURVE('',#10458,#10456,#1117,.T.);
#13294=EDGE_CURVE('',#10459,#10457,#1118,.T.);
#13295=EDGE_CURVE('',#10459,#10460,#6396,.T.);
#13296=EDGE_CURVE('',#10460,#10458,#1119,.T.);
#13297=EDGE_CURVE('',#10461,#10459,#6397,.T.);
#13298=EDGE_CURVE('',#10461,#10462,#6398,.T.);
#13299=EDGE_CURVE('',#10462,#10460,#6399,.T.);
#13300=EDGE_CURVE('',#10463,#10461,#1120,.T.);
#13301=EDGE_CURVE('',#10463,#10464,#6400,.T.);
#13302=EDGE_CURVE('',#10464,#10462,#1121,.T.);
#13303=EDGE_CURVE('',#10428,#10463,#1122,.T.);
#13304=EDGE_CURVE('',#10430,#10464,#1123,.T.);
#13305=EDGE_CURVE('',#10465,#10466,#1124,.T.);
#13306=EDGE_CURVE('',#10465,#10467,#6401,.T.);
#13307=EDGE_CURVE('',#10467,#10468,#1125,.T.);
#13308=EDGE_CURVE('',#10466,#10468,#6402,.T.);
#13309=EDGE_CURVE('',#10469,#10465,#1126,.T.);
#13310=EDGE_CURVE('',#10469,#10470,#6403,.T.);
#13311=EDGE_CURVE('',#10470,#10467,#1127,.T.);
#13312=EDGE_CURVE('',#10471,#10469,#1128,.T.);
#13313=EDGE_CURVE('',#10471,#10472,#6404,.T.);
#13314=EDGE_CURVE('',#10472,#10470,#1129,.T.);
#13315=EDGE_CURVE('',#10473,#10471,#1130,.T.);
#13316=EDGE_CURVE('',#10473,#10474,#6405,.T.);
#13317=EDGE_CURVE('',#10474,#10472,#1131,.T.);
#13318=EDGE_CURVE('',#10475,#10473,#1132,.T.);
#13319=EDGE_CURVE('',#10475,#10476,#6406,.T.);
#13320=EDGE_CURVE('',#10476,#10474,#1133,.T.);
#13321=EDGE_CURVE('',#10477,#10475,#1134,.T.);
#13322=EDGE_CURVE('',#10477,#10478,#6407,.T.);
#13323=EDGE_CURVE('',#10478,#10476,#1135,.T.);
#13324=EDGE_CURVE('',#10479,#10477,#1136,.T.);
#13325=EDGE_CURVE('',#10479,#10480,#6408,.T.);
#13326=EDGE_CURVE('',#10480,#10478,#1137,.T.);
#13327=EDGE_CURVE('',#10466,#10479,#1138,.T.);
#13328=EDGE_CURVE('',#10468,#10480,#1139,.T.);
#13329=EDGE_CURVE('',#10481,#10482,#1140,.T.);
#13330=EDGE_CURVE('',#10481,#10483,#6409,.T.);
#13331=EDGE_CURVE('',#10483,#10484,#1141,.T.);
#13332=EDGE_CURVE('',#10482,#10484,#6410,.T.);
#13333=EDGE_CURVE('',#10485,#10481,#1142,.T.);
#13334=EDGE_CURVE('',#10485,#10486,#6411,.T.);
#13335=EDGE_CURVE('',#10486,#10483,#1143,.T.);
#13336=EDGE_CURVE('',#10487,#10485,#1144,.T.);
#13337=EDGE_CURVE('',#10487,#10488,#6412,.T.);
#13338=EDGE_CURVE('',#10488,#10486,#1145,.T.);
#13339=EDGE_CURVE('',#10489,#10487,#1146,.T.);
#13340=EDGE_CURVE('',#10489,#10490,#6413,.T.);
#13341=EDGE_CURVE('',#10490,#10488,#1147,.T.);
#13342=EDGE_CURVE('',#10491,#10489,#1148,.T.);
#13343=EDGE_CURVE('',#10491,#10492,#6414,.T.);
#13344=EDGE_CURVE('',#10492,#10490,#1149,.T.);
#13345=EDGE_CURVE('',#10493,#10491,#1150,.T.);
#13346=EDGE_CURVE('',#10493,#10494,#6415,.T.);
#13347=EDGE_CURVE('',#10494,#10492,#1151,.T.);
#13348=EDGE_CURVE('',#10495,#10493,#1152,.T.);
#13349=EDGE_CURVE('',#10495,#10496,#6416,.T.);
#13350=EDGE_CURVE('',#10496,#10494,#1153,.T.);
#13351=EDGE_CURVE('',#10497,#10495,#6417,.T.);
#13352=EDGE_CURVE('',#10497,#10498,#6418,.T.);
#13353=EDGE_CURVE('',#10498,#10496,#6419,.T.);
#13354=EDGE_CURVE('',#10499,#10497,#6420,.T.);
#13355=EDGE_CURVE('',#10499,#10500,#6421,.T.);
#13356=EDGE_CURVE('',#10500,#10498,#6422,.T.);
#13357=EDGE_CURVE('',#10501,#10499,#6423,.T.);
#13358=EDGE_CURVE('',#10501,#10502,#6424,.T.);
#13359=EDGE_CURVE('',#10502,#10500,#6425,.T.);
#13360=EDGE_CURVE('',#10503,#10501,#6426,.T.);
#13361=EDGE_CURVE('',#10503,#10504,#6427,.T.);
#13362=EDGE_CURVE('',#10504,#10502,#6428,.T.);
#13363=EDGE_CURVE('',#10505,#10503,#6429,.T.);
#13364=EDGE_CURVE('',#10505,#10506,#6430,.T.);
#13365=EDGE_CURVE('',#10506,#10504,#6431,.T.);
#13366=EDGE_CURVE('',#10482,#10505,#1154,.T.);
#13367=EDGE_CURVE('',#10484,#10506,#1155,.T.);
#13368=EDGE_CURVE('',#10507,#10508,#1156,.T.);
#13369=EDGE_CURVE('',#10507,#10509,#6432,.T.);
#13370=EDGE_CURVE('',#10509,#10510,#1157,.T.);
#13371=EDGE_CURVE('',#10508,#10510,#6433,.T.);
#13372=EDGE_CURVE('',#10511,#10507,#1158,.T.);
#13373=EDGE_CURVE('',#10511,#10512,#6434,.T.);
#13374=EDGE_CURVE('',#10512,#10509,#1159,.T.);
#13375=EDGE_CURVE('',#10513,#10511,#1160,.T.);
#13376=EDGE_CURVE('',#10513,#10514,#6435,.T.);
#13377=EDGE_CURVE('',#10514,#10512,#1161,.T.);
#13378=EDGE_CURVE('',#10515,#10513,#1162,.T.);
#13379=EDGE_CURVE('',#10515,#10516,#6436,.T.);
#13380=EDGE_CURVE('',#10516,#10514,#1163,.T.);
#13381=EDGE_CURVE('',#10517,#10515,#6437,.T.);
#13382=EDGE_CURVE('',#10517,#10518,#6438,.T.);
#13383=EDGE_CURVE('',#10518,#10516,#6439,.T.);
#13384=EDGE_CURVE('',#10519,#10517,#1164,.T.);
#13385=EDGE_CURVE('',#10519,#10520,#6440,.T.);
#13386=EDGE_CURVE('',#10520,#10518,#1165,.T.);
#13387=EDGE_CURVE('',#10521,#10519,#1166,.T.);
#13388=EDGE_CURVE('',#10521,#10522,#6441,.T.);
#13389=EDGE_CURVE('',#10522,#10520,#1167,.T.);
#13390=EDGE_CURVE('',#10523,#10521,#1168,.T.);
#13391=EDGE_CURVE('',#10523,#10524,#6442,.T.);
#13392=EDGE_CURVE('',#10524,#10522,#1169,.T.);
#13393=EDGE_CURVE('',#10525,#10523,#6443,.T.);
#13394=EDGE_CURVE('',#10525,#10526,#6444,.T.);
#13395=EDGE_CURVE('',#10526,#10524,#6445,.T.);
#13396=EDGE_CURVE('',#10527,#10525,#6446,.T.);
#13397=EDGE_CURVE('',#10527,#10528,#6447,.T.);
#13398=EDGE_CURVE('',#10528,#10526,#6448,.T.);
#13399=EDGE_CURVE('',#10529,#10527,#6449,.T.);
#13400=EDGE_CURVE('',#10529,#10530,#6450,.T.);
#13401=EDGE_CURVE('',#10530,#10528,#6451,.T.);
#13402=EDGE_CURVE('',#10531,#10529,#6452,.T.);
#13403=EDGE_CURVE('',#10531,#10532,#6453,.T.);
#13404=EDGE_CURVE('',#10532,#10530,#6454,.T.);
#13405=EDGE_CURVE('',#10508,#10531,#6455,.T.);
#13406=EDGE_CURVE('',#10510,#10532,#6456,.T.);
#13407=EDGE_CURVE('',#10533,#10533,#8818,.T.);
#13408=EDGE_CURVE('',#10533,#10534,#6457,.T.);
#13409=EDGE_CURVE('',#10535,#10534,#1170,.T.);
#13410=EDGE_CURVE('',#10536,#10535,#1171,.T.);
#13411=EDGE_CURVE('',#10537,#10536,#1172,.T.);
#13412=EDGE_CURVE('',#10534,#10537,#1173,.T.);
#13413=EDGE_CURVE('',#10538,#10538,#8819,.T.);
#13414=EDGE_CURVE('',#10538,#10539,#6458,.T.);
#13415=EDGE_CURVE('',#10539,#10539,#8820,.T.);
#13416=EDGE_CURVE('',#10540,#10540,#8821,.T.);
#13417=EDGE_CURVE('',#10540,#10539,#6459,.T.);
#13418=EDGE_CURVE('',#10541,#10542,#6460,.T.);
#13419=EDGE_CURVE('',#10543,#10541,#1174,.T.);
#13420=EDGE_CURVE('',#10544,#10543,#6461,.T.);
#13421=EDGE_CURVE('',#10542,#10544,#6462,.T.);
#13422=EDGE_CURVE('',#10545,#10546,#6463,.T.);
#13423=EDGE_CURVE('',#10546,#10546,#8822,.T.);
#13424=EDGE_CURVE('',#10546,#10535,#6464,.T.);
#13425=EDGE_CURVE('',#10537,#10547,#6465,.T.);
#13426=EDGE_CURVE('',#10547,#10547,#8823,.T.);
#13427=EDGE_CURVE('',#10542,#10544,#8824,.T.);
#13428=EDGE_CURVE('',#10548,#10543,#8825,.T.);
#13429=EDGE_CURVE('',#10548,#10549,#6466,.T.);
#13430=EDGE_CURVE('',#10549,#10549,#8826,.T.);
#13431=EDGE_CURVE('',#10541,#10548,#8827,.T.);
#13432=EDGE_CURVE('',#10550,#10550,#8828,.T.);
#13433=EDGE_CURVE('',#10550,#10548,#8829,.T.);
#13434=EDGE_CURVE('',#10551,#10551,#8830,.T.);
#13435=EDGE_CURVE('',#10551,#10552,#6467,.T.);
#13436=EDGE_CURVE('',#10552,#10552,#8831,.T.);
#13437=EDGE_CURVE('',#10553,#10553,#8832,.T.);
#13438=EDGE_CURVE('',#10554,#10554,#8833,.T.);
#13439=EDGE_CURVE('',#10555,#10555,#8834,.T.);
#13440=EDGE_CURVE('',#10556,#10556,#8835,.T.);
#13441=EDGE_CURVE('',#10557,#10557,#8836,.T.);
#13442=EDGE_CURVE('',#10558,#10558,#8837,.T.);
#13443=EDGE_CURVE('',#10559,#10559,#8838,.T.);
#13444=EDGE_CURVE('',#10552,#10560,#6468,.T.);
#13445=EDGE_CURVE('',#10560,#10560,#8839,.T.);
#13446=EDGE_CURVE('',#10559,#10561,#6469,.T.);
#13447=EDGE_CURVE('',#10561,#10561,#8840,.T.);
#13448=EDGE_CURVE('',#10561,#10562,#6470,.T.);
#13449=EDGE_CURVE('',#10562,#10562,#8841,.T.);
#13450=EDGE_CURVE('',#10554,#10563,#6471,.T.);
#13451=EDGE_CURVE('',#10563,#10563,#8842,.T.);
#13452=EDGE_CURVE('',#10563,#10564,#6472,.T.);
#13453=EDGE_CURVE('',#10564,#10564,#8843,.T.);
#13454=EDGE_CURVE('',#10558,#10565,#6473,.T.);
#13455=EDGE_CURVE('',#10565,#10565,#8844,.T.);
#13456=EDGE_CURVE('',#10565,#10566,#6474,.T.);
#13457=EDGE_CURVE('',#10566,#10566,#8845,.T.);
#13458=EDGE_CURVE('',#10555,#10567,#6475,.T.);
#13459=EDGE_CURVE('',#10567,#10567,#8846,.T.);
#13460=EDGE_CURVE('',#10567,#10568,#6476,.T.);
#13461=EDGE_CURVE('',#10568,#10568,#8847,.T.);
#13462=EDGE_CURVE('',#10557,#10569,#6477,.T.);
#13463=EDGE_CURVE('',#10569,#10569,#8848,.T.);
#13464=EDGE_CURVE('',#10569,#10570,#6478,.T.);
#13465=EDGE_CURVE('',#10570,#10570,#8849,.T.);
#13466=EDGE_CURVE('',#10570,#10571,#6479,.T.);
#13467=EDGE_CURVE('',#10568,#10572,#6480,.T.);
#13468=EDGE_CURVE('',#10566,#10573,#6481,.T.);
#13469=EDGE_CURVE('',#10564,#10574,#6482,.T.);
#13470=EDGE_CURVE('',#10562,#10575,#6483,.T.);
#13471=EDGE_CURVE('',#10560,#10576,#6484,.T.);
#13472=EDGE_CURVE('',#10556,#10577,#6485,.T.);
#13473=EDGE_CURVE('',#10577,#10578,#8850,.T.);
#13474=EDGE_CURVE('',#10578,#10577,#8851,.T.);
#13475=EDGE_CURVE('',#10579,#10579,#8852,.T.);
#13476=EDGE_CURVE('',#10579,#10578,#6486,.T.);
#13477=EDGE_CURVE('',#10549,#10553,#6487,.T.);
#13478=EDGE_CURVE('',#10580,#10580,#8853,.T.);
#13479=EDGE_CURVE('',#10580,#10581,#6488,.T.);
#13480=EDGE_CURVE('',#10581,#10581,#8854,.T.);
#13481=EDGE_CURVE('',#10582,#10582,#8855,.T.);
#13482=EDGE_CURVE('',#10583,#10583,#8856,.T.);
#13483=EDGE_CURVE('',#10584,#10584,#8857,.T.);
#13484=EDGE_CURVE('',#10584,#10583,#6489,.T.);
#13485=EDGE_CURVE('',#10585,#10585,#8858,.T.);
#13486=EDGE_CURVE('',#10585,#10586,#6490,.T.);
#13487=EDGE_CURVE('',#10586,#10586,#8859,.T.);
#13488=EDGE_CURVE('',#10587,#10587,#8860,.T.);
#13489=EDGE_CURVE('',#10588,#10588,#8861,.T.);
#13490=EDGE_CURVE('',#10588,#10587,#6491,.T.);
#13491=EDGE_CURVE('',#10589,#10589,#8862,.T.);
#13492=EDGE_CURVE('',#10589,#10590,#6492,.T.);
#13493=EDGE_CURVE('',#10590,#10590,#8863,.T.);
#13494=EDGE_CURVE('',#10591,#10591,#8864,.T.);
#13495=EDGE_CURVE('',#10591,#10592,#6493,.T.);
#13496=EDGE_CURVE('',#10592,#10592,#8865,.T.);
#13497=EDGE_CURVE('',#10593,#10593,#8866,.T.);
#13498=EDGE_CURVE('',#10593,#10591,#6494,.T.);
#13499=EDGE_CURVE('',#10590,#10593,#6495,.T.);
#13500=EDGE_CURVE('',#10594,#10594,#8867,.T.);
#13501=EDGE_CURVE('',#10594,#10582,#6496,.T.);
#13502=EDGE_CURVE('',#10595,#10595,#8868,.T.);
#13503=EDGE_CURVE('',#10595,#10594,#6497,.T.);
#13504=EDGE_CURVE('',#10596,#10596,#8869,.T.);
#13505=EDGE_CURVE('',#10596,#10597,#6498,.T.);
#13506=EDGE_CURVE('',#10597,#10597,#8870,.T.);
#13507=EDGE_CURVE('',#10597,#10598,#6499,.T.);
#13508=EDGE_CURVE('',#10598,#10598,#8871,.T.);
#13509=EDGE_CURVE('',#10598,#10599,#6500,.T.);
#13510=EDGE_CURVE('',#10599,#10599,#8872,.T.);
#13511=EDGE_CURVE('',#10592,#10599,#8873,.T.);
#13512=EDGE_CURVE('',#10600,#10600,#8874,.T.);
#13513=EDGE_CURVE('',#10600,#10601,#6501,.T.);
#13514=EDGE_CURVE('',#10601,#10601,#8875,.T.);
#13515=EDGE_CURVE('',#10602,#10602,#8876,.T.);
#13516=EDGE_CURVE('',#10602,#10603,#6502,.T.);
#13517=EDGE_CURVE('',#10603,#10603,#8877,.T.);
#13518=EDGE_CURVE('',#10604,#10604,#8878,.T.);
#13519=EDGE_CURVE('',#10605,#10605,#8879,.T.);
#13520=EDGE_CURVE('',#10605,#10606,#8880,.T.);
#13521=EDGE_CURVE('',#10606,#10606,#8881,.T.);
#13522=EDGE_CURVE('',#10606,#10607,#6503,.T.);
#13523=EDGE_CURVE('',#10607,#10607,#8882,.T.);
#13524=EDGE_CURVE('',#10608,#10608,#8883,.T.);
#13525=EDGE_CURVE('',#10608,#10609,#6504,.T.);
#13526=EDGE_CURVE('',#10609,#10609,#8884,.T.);
#13527=EDGE_CURVE('',#10610,#10610,#8885,.T.);
#13528=EDGE_CURVE('',#10610,#10604,#6505,.T.);
#13529=EDGE_CURVE('',#10611,#10611,#8886,.T.);
#13530=EDGE_CURVE('',#10611,#10610,#6506,.T.);
#13531=EDGE_CURVE('',#10612,#10612,#8887,.T.);
#13532=EDGE_CURVE('',#10612,#10611,#6507,.T.);
#13533=EDGE_CURVE('',#10613,#10613,#8888,.T.);
#13534=EDGE_CURVE('',#10614,#10614,#8889,.T.);
#13535=EDGE_CURVE('',#10614,#10613,#6508,.T.);
#13536=EDGE_CURVE('',#10615,#10615,#8890,.T.);
#13537=EDGE_CURVE('',#10615,#10614,#6509,.T.);
#13538=EDGE_CURVE('',#10616,#10616,#8891,.T.);
#13539=EDGE_CURVE('',#10616,#10617,#6510,.T.);
#13540=EDGE_CURVE('',#10617,#10617,#8892,.T.);
#13541=EDGE_CURVE('',#10618,#10619,#191,.T.);
#13542=EDGE_CURVE('',#10618,#10620,#1175,.T.);
#13543=EDGE_CURVE('',#10621,#10620,#192,.T.);
#13544=EDGE_CURVE('',#10621,#10619,#1176,.T.);
#13545=EDGE_CURVE('',#10622,#10623,#193,.T.);
#13546=EDGE_CURVE('',#10622,#10624,#1177,.T.);
#13547=EDGE_CURVE('',#10625,#10624,#194,.T.);
#13548=EDGE_CURVE('',#10625,#10623,#1178,.T.);
#13549=EDGE_CURVE('',#10626,#10627,#195,.T.);
#13550=EDGE_CURVE('',#10626,#10628,#1179,.T.);
#13551=EDGE_CURVE('',#10629,#10628,#196,.T.);
#13552=EDGE_CURVE('',#10629,#10627,#1180,.T.);
#13553=EDGE_CURVE('',#10630,#10631,#197,.T.);
#13554=EDGE_CURVE('',#10630,#10632,#1181,.T.);
#13555=EDGE_CURVE('',#10633,#10632,#198,.T.);
#13556=EDGE_CURVE('',#10633,#10631,#1182,.T.);
#13557=EDGE_CURVE('',#10634,#10635,#199,.T.);
#13558=EDGE_CURVE('',#10634,#10636,#1183,.T.);
#13559=EDGE_CURVE('',#10637,#10636,#200,.T.);
#13560=EDGE_CURVE('',#10637,#10635,#1184,.T.);
#13561=EDGE_CURVE('',#10638,#10639,#201,.T.);
#13562=EDGE_CURVE('',#10638,#10640,#1185,.T.);
#13563=EDGE_CURVE('',#10641,#10640,#202,.T.);
#13564=EDGE_CURVE('',#10641,#10639,#1186,.T.);
#13565=EDGE_CURVE('',#10642,#10643,#203,.T.);
#13566=EDGE_CURVE('',#10642,#10644,#1187,.T.);
#13567=EDGE_CURVE('',#10645,#10644,#204,.T.);
#13568=EDGE_CURVE('',#10645,#10643,#1188,.T.);
#13569=EDGE_CURVE('',#10646,#10647,#205,.T.);
#13570=EDGE_CURVE('',#10646,#10648,#1189,.T.);
#13571=EDGE_CURVE('',#10649,#10648,#206,.T.);
#13572=EDGE_CURVE('',#10649,#10647,#1190,.T.);
#13573=EDGE_CURVE('',#10650,#10651,#207,.T.);
#13574=EDGE_CURVE('',#10650,#10652,#1191,.T.);
#13575=EDGE_CURVE('',#10653,#10652,#208,.T.);
#13576=EDGE_CURVE('',#10653,#10651,#1192,.T.);
#13577=EDGE_CURVE('',#10654,#10655,#209,.T.);
#13578=EDGE_CURVE('',#10654,#10656,#1193,.T.);
#13579=EDGE_CURVE('',#10657,#10656,#210,.T.);
#13580=EDGE_CURVE('',#10657,#10655,#1194,.T.);
#13581=EDGE_CURVE('',#10658,#10659,#211,.T.);
#13582=EDGE_CURVE('',#10658,#10660,#1195,.T.);
#13583=EDGE_CURVE('',#10661,#10660,#212,.T.);
#13584=EDGE_CURVE('',#10661,#10659,#1196,.T.);
#13585=EDGE_CURVE('',#10662,#10663,#213,.T.);
#13586=EDGE_CURVE('',#10662,#10664,#1197,.T.);
#13587=EDGE_CURVE('',#10665,#10664,#214,.T.);
#13588=EDGE_CURVE('',#10665,#10663,#1198,.T.);
#13589=EDGE_CURVE('',#10666,#10667,#215,.T.);
#13590=EDGE_CURVE('',#10666,#10668,#1199,.T.);
#13591=EDGE_CURVE('',#10669,#10668,#216,.T.);
#13592=EDGE_CURVE('',#10669,#10667,#1200,.T.);
#13593=EDGE_CURVE('',#10670,#10671,#217,.T.);
#13594=EDGE_CURVE('',#10670,#10672,#1201,.T.);
#13595=EDGE_CURVE('',#10673,#10672,#218,.T.);
#13596=EDGE_CURVE('',#10673,#10671,#1202,.T.);
#13597=EDGE_CURVE('',#10674,#10675,#219,.T.);
#13598=EDGE_CURVE('',#10674,#10676,#1203,.T.);
#13599=EDGE_CURVE('',#10677,#10676,#220,.T.);
#13600=EDGE_CURVE('',#10677,#10675,#1204,.T.);
#13601=EDGE_CURVE('',#10678,#10679,#221,.T.);
#13602=EDGE_CURVE('',#10678,#10680,#1205,.T.);
#13603=EDGE_CURVE('',#10681,#10680,#222,.T.);
#13604=EDGE_CURVE('',#10681,#10679,#1206,.T.);
#13605=EDGE_CURVE('',#10682,#10683,#1207,.T.);
#13606=EDGE_CURVE('',#10684,#10683,#223,.T.);
#13607=EDGE_CURVE('',#10684,#10685,#1208,.T.);
#13608=EDGE_CURVE('',#10682,#10685,#224,.T.);
#13609=EDGE_CURVE('',#10686,#10686,#8893,.T.);
#13610=EDGE_CURVE('',#10686,#10687,#6511,.T.);
#13611=EDGE_CURVE('',#10687,#10687,#8894,.T.);
#13612=EDGE_CURVE('',#10688,#10689,#225,.T.);
#13613=EDGE_CURVE('',#10688,#10690,#1209,.T.);
#13614=EDGE_CURVE('',#10691,#10690,#226,.T.);
#13615=EDGE_CURVE('',#10691,#10689,#1210,.T.);
#13616=EDGE_CURVE('',#10692,#10693,#227,.T.);
#13617=EDGE_CURVE('',#10692,#10694,#1211,.T.);
#13618=EDGE_CURVE('',#10695,#10694,#228,.T.);
#13619=EDGE_CURVE('',#10695,#10693,#1212,.T.);
#13620=EDGE_CURVE('',#10696,#10697,#229,.T.);
#13621=EDGE_CURVE('',#10696,#10698,#1213,.T.);
#13622=EDGE_CURVE('',#10699,#10698,#230,.T.);
#13623=EDGE_CURVE('',#10699,#10697,#1214,.T.);
#13624=EDGE_CURVE('',#10700,#10701,#231,.T.);
#13625=EDGE_CURVE('',#10700,#10702,#1215,.T.);
#13626=EDGE_CURVE('',#10703,#10702,#232,.T.);
#13627=EDGE_CURVE('',#10703,#10701,#1216,.T.);
#13628=EDGE_CURVE('',#10704,#10705,#233,.T.);
#13629=EDGE_CURVE('',#10704,#10706,#1217,.T.);
#13630=EDGE_CURVE('',#10707,#10706,#234,.T.);
#13631=EDGE_CURVE('',#10707,#10705,#1218,.T.);
#13632=EDGE_CURVE('',#10708,#10709,#235,.T.);
#13633=EDGE_CURVE('',#10708,#10710,#1219,.T.);
#13634=EDGE_CURVE('',#10711,#10710,#236,.T.);
#13635=EDGE_CURVE('',#10711,#10709,#1220,.T.);
#13636=EDGE_CURVE('',#10712,#10713,#237,.T.);
#13637=EDGE_CURVE('',#10712,#10714,#1221,.T.);
#13638=EDGE_CURVE('',#10715,#10714,#238,.T.);
#13639=EDGE_CURVE('',#10715,#10713,#1222,.T.);
#13640=EDGE_CURVE('',#10716,#10717,#239,.T.);
#13641=EDGE_CURVE('',#10716,#10718,#1223,.T.);
#13642=EDGE_CURVE('',#10719,#10718,#240,.T.);
#13643=EDGE_CURVE('',#10719,#10717,#1224,.T.);
#13644=EDGE_CURVE('',#10720,#10721,#241,.T.);
#13645=EDGE_CURVE('',#10720,#10722,#1225,.T.);
#13646=EDGE_CURVE('',#10723,#10722,#242,.T.);
#13647=EDGE_CURVE('',#10723,#10721,#1226,.T.);
#13648=EDGE_CURVE('',#10724,#10725,#243,.T.);
#13649=EDGE_CURVE('',#10724,#10726,#1227,.T.);
#13650=EDGE_CURVE('',#10727,#10726,#244,.T.);
#13651=EDGE_CURVE('',#10727,#10725,#1228,.T.);
#13652=EDGE_CURVE('',#10728,#10729,#245,.T.);
#13653=EDGE_CURVE('',#10728,#10730,#1229,.T.);
#13654=EDGE_CURVE('',#10731,#10730,#246,.T.);
#13655=EDGE_CURVE('',#10731,#10729,#1230,.T.);
#13656=EDGE_CURVE('',#10732,#10733,#247,.T.);
#13657=EDGE_CURVE('',#10732,#10734,#1231,.T.);
#13658=EDGE_CURVE('',#10735,#10734,#248,.T.);
#13659=EDGE_CURVE('',#10735,#10733,#1232,.T.);
#13660=EDGE_CURVE('',#10736,#10737,#249,.T.);
#13661=EDGE_CURVE('',#10736,#10738,#1233,.T.);
#13662=EDGE_CURVE('',#10739,#10738,#250,.T.);
#13663=EDGE_CURVE('',#10739,#10737,#1234,.T.);
#13664=EDGE_CURVE('',#10740,#10741,#251,.T.);
#13665=EDGE_CURVE('',#10740,#10742,#1235,.T.);
#13666=EDGE_CURVE('',#10743,#10742,#252,.T.);
#13667=EDGE_CURVE('',#10743,#10741,#1236,.T.);
#13668=EDGE_CURVE('',#10744,#10745,#253,.T.);
#13669=EDGE_CURVE('',#10744,#10746,#1237,.T.);
#13670=EDGE_CURVE('',#10747,#10746,#254,.T.);
#13671=EDGE_CURVE('',#10747,#10745,#1238,.T.);
#13672=EDGE_CURVE('',#10748,#10749,#255,.T.);
#13673=EDGE_CURVE('',#10748,#10750,#1239,.T.);
#13674=EDGE_CURVE('',#10751,#10750,#256,.T.);
#13675=EDGE_CURVE('',#10751,#10749,#1240,.T.);
#13676=EDGE_CURVE('',#10752,#10753,#1241,.T.);
#13677=EDGE_CURVE('',#10754,#10753,#257,.T.);
#13678=EDGE_CURVE('',#10754,#10755,#1242,.T.);
#13679=EDGE_CURVE('',#10752,#10755,#258,.T.);
#13680=EDGE_CURVE('',#10687,#10617,#6512,.T.);
#13681=EDGE_CURVE('',#10686,#10616,#6513,.T.);
#13682=EDGE_CURVE('',#10690,#10691,#8895,.T.);
#13683=EDGE_CURVE('',#10620,#10756,#8896,.T.);
#13684=EDGE_CURVE('',#10757,#10756,#259,.T.);
#13685=EDGE_CURVE('',#10757,#10621,#8897,.T.);
#13686=EDGE_CURVE('',#10688,#10689,#8898,.T.);
#13687=EDGE_CURVE('',#10618,#10758,#8899,.T.);
#13688=EDGE_CURVE('',#10759,#10758,#260,.T.);
#13689=EDGE_CURVE('',#10756,#10759,#1243,.T.);
#13690=EDGE_CURVE('',#10694,#10695,#8900,.T.);
#13691=EDGE_CURVE('',#10624,#10760,#8901,.T.);
#13692=EDGE_CURVE('',#10761,#10760,#261,.T.);
#13693=EDGE_CURVE('',#10761,#10625,#8902,.T.);
#13694=EDGE_CURVE('',#10692,#10693,#8903,.T.);
#13695=EDGE_CURVE('',#10622,#10762,#8904,.T.);
#13696=EDGE_CURVE('',#10763,#10762,#262,.T.);
#13697=EDGE_CURVE('',#10760,#10763,#1244,.T.);
#13698=EDGE_CURVE('',#10698,#10699,#8905,.T.);
#13699=EDGE_CURVE('',#10628,#10764,#8906,.T.);
#13700=EDGE_CURVE('',#10765,#10764,#263,.T.);
#13701=EDGE_CURVE('',#10765,#10629,#8907,.T.);
#13702=EDGE_CURVE('',#10696,#10697,#8908,.T.);
#13703=EDGE_CURVE('',#10626,#10766,#8909,.T.);
#13704=EDGE_CURVE('',#10767,#10766,#264,.T.);
#13705=EDGE_CURVE('',#10764,#10767,#1245,.T.);
#13706=EDGE_CURVE('',#10702,#10703,#8910,.T.);
#13707=EDGE_CURVE('',#10632,#10768,#8911,.T.);
#13708=EDGE_CURVE('',#10769,#10768,#265,.T.);
#13709=EDGE_CURVE('',#10769,#10633,#8912,.T.);
#13710=EDGE_CURVE('',#10700,#10701,#8913,.T.);
#13711=EDGE_CURVE('',#10630,#10770,#8914,.T.);
#13712=EDGE_CURVE('',#10771,#10770,#266,.T.);
#13713=EDGE_CURVE('',#10768,#10771,#1246,.T.);
#13714=EDGE_CURVE('',#10706,#10707,#8915,.T.);
#13715=EDGE_CURVE('',#10636,#10772,#8916,.T.);
#13716=EDGE_CURVE('',#10773,#10772,#267,.T.);
#13717=EDGE_CURVE('',#10773,#10637,#8917,.T.);
#13718=EDGE_CURVE('',#10704,#10705,#8918,.T.);
#13719=EDGE_CURVE('',#10634,#10774,#8919,.T.);
#13720=EDGE_CURVE('',#10775,#10774,#268,.T.);
#13721=EDGE_CURVE('',#10772,#10775,#1247,.T.);
#13722=EDGE_CURVE('',#10710,#10711,#8920,.T.);
#13723=EDGE_CURVE('',#10640,#10776,#8921,.T.);
#13724=EDGE_CURVE('',#10777,#10776,#269,.T.);
#13725=EDGE_CURVE('',#10777,#10641,#8922,.T.);
#13726=EDGE_CURVE('',#10708,#10709,#8923,.T.);
#13727=EDGE_CURVE('',#10638,#10778,#8924,.T.);
#13728=EDGE_CURVE('',#10779,#10778,#270,.T.);
#13729=EDGE_CURVE('',#10776,#10779,#1248,.T.);
#13730=EDGE_CURVE('',#10714,#10715,#8925,.T.);
#13731=EDGE_CURVE('',#10644,#10780,#8926,.T.);
#13732=EDGE_CURVE('',#10781,#10780,#271,.T.);
#13733=EDGE_CURVE('',#10781,#10645,#8927,.T.);
#13734=EDGE_CURVE('',#10712,#10713,#8928,.T.);
#13735=EDGE_CURVE('',#10642,#10782,#8929,.T.);
#13736=EDGE_CURVE('',#10783,#10782,#272,.T.);
#13737=EDGE_CURVE('',#10780,#10783,#1249,.T.);
#13738=EDGE_CURVE('',#10718,#10719,#8930,.T.);
#13739=EDGE_CURVE('',#10648,#10784,#8931,.T.);
#13740=EDGE_CURVE('',#10785,#10784,#273,.T.);
#13741=EDGE_CURVE('',#10785,#10649,#8932,.T.);
#13742=EDGE_CURVE('',#10716,#10717,#8933,.T.);
#13743=EDGE_CURVE('',#10646,#10786,#8934,.T.);
#13744=EDGE_CURVE('',#10787,#10786,#274,.T.);
#13745=EDGE_CURVE('',#10784,#10787,#1250,.T.);
#13746=EDGE_CURVE('',#10722,#10723,#8935,.T.);
#13747=EDGE_CURVE('',#10652,#10788,#8936,.T.);
#13748=EDGE_CURVE('',#10789,#10788,#275,.T.);
#13749=EDGE_CURVE('',#10789,#10653,#8937,.T.);
#13750=EDGE_CURVE('',#10720,#10721,#8938,.T.);
#13751=EDGE_CURVE('',#10650,#10790,#8939,.T.);
#13752=EDGE_CURVE('',#10791,#10790,#276,.T.);
#13753=EDGE_CURVE('',#10788,#10791,#1251,.T.);
#13754=EDGE_CURVE('',#10726,#10727,#8940,.T.);
#13755=EDGE_CURVE('',#10656,#10792,#8941,.T.);
#13756=EDGE_CURVE('',#10793,#10792,#277,.T.);
#13757=EDGE_CURVE('',#10793,#10657,#8942,.T.);
#13758=EDGE_CURVE('',#10724,#10725,#8943,.T.);
#13759=EDGE_CURVE('',#10654,#10794,#8944,.T.);
#13760=EDGE_CURVE('',#10795,#10794,#278,.T.);
#13761=EDGE_CURVE('',#10792,#10795,#1252,.T.);
#13762=EDGE_CURVE('',#10730,#10731,#8945,.T.);
#13763=EDGE_CURVE('',#10660,#10796,#8946,.T.);
#13764=EDGE_CURVE('',#10797,#10796,#279,.T.);
#13765=EDGE_CURVE('',#10797,#10661,#8947,.T.);
#13766=EDGE_CURVE('',#10728,#10729,#8948,.T.);
#13767=EDGE_CURVE('',#10658,#10798,#8949,.T.);
#13768=EDGE_CURVE('',#10799,#10798,#280,.T.);
#13769=EDGE_CURVE('',#10796,#10799,#1253,.T.);
#13770=EDGE_CURVE('',#10734,#10735,#8950,.T.);
#13771=EDGE_CURVE('',#10664,#10800,#8951,.T.);
#13772=EDGE_CURVE('',#10801,#10800,#281,.T.);
#13773=EDGE_CURVE('',#10801,#10665,#8952,.T.);
#13774=EDGE_CURVE('',#10732,#10733,#8953,.T.);
#13775=EDGE_CURVE('',#10662,#10802,#8954,.T.);
#13776=EDGE_CURVE('',#10803,#10802,#282,.T.);
#13777=EDGE_CURVE('',#10800,#10803,#1254,.T.);
#13778=EDGE_CURVE('',#10738,#10739,#8955,.T.);
#13779=EDGE_CURVE('',#10668,#10804,#8956,.T.);
#13780=EDGE_CURVE('',#10805,#10804,#283,.T.);
#13781=EDGE_CURVE('',#10805,#10669,#8957,.T.);
#13782=EDGE_CURVE('',#10736,#10737,#8958,.T.);
#13783=EDGE_CURVE('',#10666,#10806,#8959,.T.);
#13784=EDGE_CURVE('',#10807,#10806,#284,.T.);
#13785=EDGE_CURVE('',#10804,#10807,#1255,.T.);
#13786=EDGE_CURVE('',#10742,#10743,#8960,.T.);
#13787=EDGE_CURVE('',#10672,#10808,#8961,.T.);
#13788=EDGE_CURVE('',#10809,#10808,#285,.T.);
#13789=EDGE_CURVE('',#10809,#10673,#8962,.T.);
#13790=EDGE_CURVE('',#10740,#10741,#8963,.T.);
#13791=EDGE_CURVE('',#10670,#10810,#8964,.T.);
#13792=EDGE_CURVE('',#10811,#10810,#286,.T.);
#13793=EDGE_CURVE('',#10808,#10811,#1256,.T.);
#13794=EDGE_CURVE('',#10746,#10747,#8965,.T.);
#13795=EDGE_CURVE('',#10676,#10812,#8966,.T.);
#13796=EDGE_CURVE('',#10813,#10812,#287,.T.);
#13797=EDGE_CURVE('',#10813,#10677,#8967,.T.);
#13798=EDGE_CURVE('',#10744,#10745,#8968,.T.);
#13799=EDGE_CURVE('',#10674,#10814,#8969,.T.);
#13800=EDGE_CURVE('',#10815,#10814,#288,.T.);
#13801=EDGE_CURVE('',#10812,#10815,#1257,.T.);
#13802=EDGE_CURVE('',#10750,#10751,#8970,.T.);
#13803=EDGE_CURVE('',#10680,#10816,#8971,.T.);
#13804=EDGE_CURVE('',#10817,#10816,#289,.T.);
#13805=EDGE_CURVE('',#10817,#10681,#8972,.T.);
#13806=EDGE_CURVE('',#10748,#10749,#8973,.T.);
#13807=EDGE_CURVE('',#10678,#10818,#8974,.T.);
#13808=EDGE_CURVE('',#10819,#10818,#290,.T.);
#13809=EDGE_CURVE('',#10816,#10819,#1258,.T.);
#13810=EDGE_CURVE('',#10754,#10753,#8975,.T.);
#13811=EDGE_CURVE('',#10755,#10752,#8976,.T.);
#13812=EDGE_CURVE('',#10683,#10820,#8977,.T.);
#13813=EDGE_CURVE('',#10821,#10820,#291,.T.);
#13814=EDGE_CURVE('',#10821,#10684,#8978,.T.);
#13815=EDGE_CURVE('',#10682,#10822,#8979,.T.);
#13816=EDGE_CURVE('',#10823,#10822,#292,.T.);
#13817=EDGE_CURVE('',#10820,#10823,#1259,.T.);
#13818=EDGE_CURVE('',#10824,#10619,#8980,.T.);
#13819=EDGE_CURVE('',#10758,#10824,#6514,.T.);
#13820=EDGE_CURVE('',#10825,#10757,#1260,.T.);
#13821=EDGE_CURVE('',#10824,#10825,#293,.T.);
#13822=EDGE_CURVE('',#10826,#10826,#8981,.T.);
#13823=EDGE_CURVE('',#10826,#10827,#6515,.T.);
#13824=EDGE_CURVE('',#10827,#10828,#8982,.T.);
#13825=EDGE_CURVE('',#10828,#10785,#1261,.T.);
#13826=EDGE_CURVE('',#10787,#10829,#8983,.T.);
#13827=EDGE_CURVE('',#10829,#10781,#1262,.T.);
#13828=EDGE_CURVE('',#10783,#10830,#8984,.T.);
#13829=EDGE_CURVE('',#10830,#10777,#1263,.T.);
#13830=EDGE_CURVE('',#10779,#10831,#8985,.T.);
#13831=EDGE_CURVE('',#10831,#10773,#1264,.T.);
#13832=EDGE_CURVE('',#10775,#10832,#8986,.T.);
#13833=EDGE_CURVE('',#10832,#10769,#1265,.T.);
#13834=EDGE_CURVE('',#10771,#10833,#8987,.T.);
#13835=EDGE_CURVE('',#10833,#10765,#1266,.T.);
#13836=EDGE_CURVE('',#10767,#10834,#8988,.T.);
#13837=EDGE_CURVE('',#10834,#10761,#1267,.T.);
#13838=EDGE_CURVE('',#10763,#10825,#8989,.T.);
#13839=EDGE_CURVE('',#10759,#10835,#8990,.T.);
#13840=EDGE_CURVE('',#10835,#10821,#1268,.T.);
#13841=EDGE_CURVE('',#10823,#10836,#8991,.T.);
#13842=EDGE_CURVE('',#10836,#10817,#1269,.T.);
#13843=EDGE_CURVE('',#10819,#10837,#8992,.T.);
#13844=EDGE_CURVE('',#10837,#10813,#1270,.T.);
#13845=EDGE_CURVE('',#10815,#10838,#8993,.T.);
#13846=EDGE_CURVE('',#10838,#10809,#1271,.T.);
#13847=EDGE_CURVE('',#10811,#10839,#8994,.T.);
#13848=EDGE_CURVE('',#10839,#10805,#1272,.T.);
#13849=EDGE_CURVE('',#10807,#10840,#8995,.T.);
#13850=EDGE_CURVE('',#10840,#10801,#1273,.T.);
#13851=EDGE_CURVE('',#10803,#10841,#8996,.T.);
#13852=EDGE_CURVE('',#10841,#10797,#1274,.T.);
#13853=EDGE_CURVE('',#10799,#10842,#8997,.T.);
#13854=EDGE_CURVE('',#10842,#10793,#1275,.T.);
#13855=EDGE_CURVE('',#10795,#10843,#8998,.T.);
#13856=EDGE_CURVE('',#10843,#10789,#1276,.T.);
#13857=EDGE_CURVE('',#10791,#10827,#8999,.T.);
#13858=EDGE_CURVE('',#10844,#10623,#9000,.T.);
#13859=EDGE_CURVE('',#10762,#10844,#6516,.T.);
#13860=EDGE_CURVE('',#10844,#10834,#294,.T.);
#13861=EDGE_CURVE('',#10845,#10627,#9001,.T.);
#13862=EDGE_CURVE('',#10766,#10845,#6517,.T.);
#13863=EDGE_CURVE('',#10845,#10833,#295,.T.);
#13864=EDGE_CURVE('',#10846,#10631,#9002,.T.);
#13865=EDGE_CURVE('',#10770,#10846,#6518,.T.);
#13866=EDGE_CURVE('',#10846,#10832,#296,.T.);
#13867=EDGE_CURVE('',#10847,#10635,#9003,.T.);
#13868=EDGE_CURVE('',#10774,#10847,#6519,.T.);
#13869=EDGE_CURVE('',#10847,#10831,#297,.T.);
#13870=EDGE_CURVE('',#10848,#10639,#9004,.T.);
#13871=EDGE_CURVE('',#10778,#10848,#6520,.T.);
#13872=EDGE_CURVE('',#10848,#10830,#298,.T.);
#13873=EDGE_CURVE('',#10849,#10643,#9005,.T.);
#13874=EDGE_CURVE('',#10782,#10849,#6521,.T.);
#13875=EDGE_CURVE('',#10849,#10829,#299,.T.);
#13876=EDGE_CURVE('',#10850,#10647,#9006,.T.);
#13877=EDGE_CURVE('',#10786,#10850,#6522,.T.);
#13878=EDGE_CURVE('',#10850,#10828,#300,.T.);
#13879=EDGE_CURVE('',#10851,#10651,#9007,.T.);
#13880=EDGE_CURVE('',#10790,#10851,#6523,.T.);
#13881=EDGE_CURVE('',#10851,#10843,#301,.T.);
#13882=EDGE_CURVE('',#10852,#10655,#9008,.T.);
#13883=EDGE_CURVE('',#10794,#10852,#6524,.T.);
#13884=EDGE_CURVE('',#10852,#10842,#302,.T.);
#13885=EDGE_CURVE('',#10853,#10659,#9009,.T.);
#13886=EDGE_CURVE('',#10798,#10853,#6525,.T.);
#13887=EDGE_CURVE('',#10853,#10841,#303,.T.);
#13888=EDGE_CURVE('',#10854,#10663,#9010,.T.);
#13889=EDGE_CURVE('',#10802,#10854,#6526,.T.);
#13890=EDGE_CURVE('',#10854,#10840,#304,.T.);
#13891=EDGE_CURVE('',#10855,#10667,#9011,.T.);
#13892=EDGE_CURVE('',#10806,#10855,#6527,.T.);
#13893=EDGE_CURVE('',#10855,#10839,#305,.T.);
#13894=EDGE_CURVE('',#10856,#10671,#9012,.T.);
#13895=EDGE_CURVE('',#10810,#10856,#6528,.T.);
#13896=EDGE_CURVE('',#10856,#10838,#306,.T.);
#13897=EDGE_CURVE('',#10857,#10675,#9013,.T.);
#13898=EDGE_CURVE('',#10814,#10857,#6529,.T.);
#13899=EDGE_CURVE('',#10857,#10837,#307,.T.);
#13900=EDGE_CURVE('',#10858,#10679,#9014,.T.);
#13901=EDGE_CURVE('',#10818,#10858,#6530,.T.);
#13902=EDGE_CURVE('',#10858,#10836,#308,.T.);
#13903=EDGE_CURVE('',#10859,#10835,#309,.T.);
#13904=EDGE_CURVE('',#10859,#10685,#9015,.T.);
#13905=EDGE_CURVE('',#10822,#10859,#6531,.T.);
#13906=EDGE_CURVE('',#10860,#10860,#9016,.T.);
#13907=EDGE_CURVE('',#10860,#10861,#6532,.T.);
#13908=EDGE_CURVE('',#10861,#10861,#9017,.T.);
#13909=EDGE_CURVE('',#10862,#10862,#9018,.T.);
#13910=EDGE_CURVE('',#10863,#10863,#9019,.T.);
#13911=EDGE_CURVE('',#10863,#10862,#6533,.T.);
#13912=EDGE_CURVE('',#10864,#10864,#9020,.T.);
#13913=EDGE_CURVE('',#10864,#10863,#6534,.T.);
#13914=EDGE_CURVE('',#10865,#10865,#9021,.T.);
#13915=EDGE_CURVE('',#10866,#10866,#9022,.T.);
#13916=EDGE_CURVE('',#10866,#10865,#6535,.T.);
#13917=EDGE_CURVE('',#10867,#10867,#9023,.T.);
#13918=EDGE_CURVE('',#10867,#10868,#6536,.T.);
#13919=EDGE_CURVE('',#10868,#10868,#9024,.T.);
#13920=EDGE_CURVE('',#10868,#10860,#6537,.T.);
#13921=EDGE_CURVE('',#10869,#10869,#9025,.T.);
#13922=EDGE_CURVE('',#10869,#10870,#6538,.T.);
#13923=EDGE_CURVE('',#10870,#10870,#9026,.T.);
#13924=EDGE_CURVE('',#10871,#10871,#9027,.T.);
#13925=EDGE_CURVE('',#10872,#10872,#9028,.T.);
#13926=EDGE_CURVE('',#10872,#10871,#6539,.T.);
#13927=EDGE_CURVE('',#10873,#10873,#9029,.T.);
#13928=EDGE_CURVE('',#10873,#10872,#6540,.T.);
#13929=EDGE_CURVE('',#10874,#10874,#9030,.T.);
#13930=EDGE_CURVE('',#10874,#10873,#6541,.T.);
#13931=EDGE_CURVE('',#10875,#10875,#9031,.T.);
#13932=EDGE_CURVE('',#10875,#10876,#6542,.T.);
#13933=EDGE_CURVE('',#10876,#10876,#9032,.T.);
#13934=EDGE_CURVE('',#10876,#10869,#6543,.T.);
#13935=EDGE_CURVE('',#10877,#10877,#9033,.T.);
#13936=EDGE_CURVE('',#10877,#10878,#6544,.T.);
#13937=EDGE_CURVE('',#10878,#10878,#9034,.T.);
#13938=EDGE_CURVE('',#10879,#10879,#9035,.T.);
#13939=EDGE_CURVE('',#10879,#10880,#6545,.T.);
#13940=EDGE_CURVE('',#10880,#10880,#9036,.T.);
#13941=EDGE_CURVE('',#10881,#10882,#6546,.T.);
#13942=EDGE_CURVE('',#10881,#10883,#6547,.T.);
#13943=EDGE_CURVE('',#10884,#10883,#6548,.T.);
#13944=EDGE_CURVE('',#10882,#10884,#6549,.T.);
#13945=EDGE_CURVE('',#10885,#10882,#9037,.T.);
#13946=EDGE_CURVE('',#10886,#10884,#9038,.T.);
#13947=EDGE_CURVE('',#10885,#10886,#6550,.T.);
#13948=EDGE_CURVE('',#10885,#10887,#6551,.T.);
#13949=EDGE_CURVE('',#10888,#10886,#6552,.T.);
#13950=EDGE_CURVE('',#10887,#10888,#6553,.T.);
#13951=EDGE_CURVE('',#10887,#10889,#9039,.T.);
#13952=EDGE_CURVE('',#10890,#10888,#9040,.T.);
#13953=EDGE_CURVE('',#10889,#10890,#6554,.T.);
#13954=EDGE_CURVE('',#10889,#10891,#6555,.T.);
#13955=EDGE_CURVE('',#10892,#10890,#6556,.T.);
#13956=EDGE_CURVE('',#10891,#10892,#6557,.T.);
#13957=EDGE_CURVE('',#10893,#10891,#9041,.T.);
#13958=EDGE_CURVE('',#10894,#10892,#9042,.T.);
#13959=EDGE_CURVE('',#10893,#10894,#6558,.T.);
#13960=EDGE_CURVE('',#10893,#10895,#6559,.T.);
#13961=EDGE_CURVE('',#10896,#10894,#6560,.T.);
#13962=EDGE_CURVE('',#10895,#10896,#6561,.T.);
#13963=EDGE_CURVE('',#10881,#10895,#9043,.T.);
#13964=EDGE_CURVE('',#10883,#10896,#9044,.T.);
#13965=EDGE_CURVE('',#10897,#10898,#6562,.T.);
#13966=EDGE_CURVE('',#10897,#10899,#1277,.T.);
#13967=EDGE_CURVE('',#10899,#10900,#9045,.T.);
#13968=EDGE_CURVE('',#10900,#10901,#6563,.T.);
#13969=EDGE_CURVE('',#10901,#10901,#9046,.T.);
#13970=EDGE_CURVE('',#10900,#10902,#9047,.T.);
#13971=EDGE_CURVE('',#10902,#10898,#1278,.T.);
#13972=EDGE_CURVE('',#10903,#10904,#6564,.T.);
#13973=EDGE_CURVE('',#10903,#10897,#1279,.T.);
#13974=EDGE_CURVE('',#10898,#10904,#1280,.T.);
#13975=EDGE_CURVE('',#10905,#10906,#6565,.T.);
#13976=EDGE_CURVE('',#10905,#10903,#1281,.T.);
#13977=EDGE_CURVE('',#10904,#10906,#1282,.T.);
#13978=EDGE_CURVE('',#10907,#10908,#6566,.T.);
#13979=EDGE_CURVE('',#10907,#10905,#1283,.T.);
#13980=EDGE_CURVE('',#10906,#10908,#1284,.T.);
#13981=EDGE_CURVE('',#10909,#10910,#6567,.T.);
#13982=EDGE_CURVE('',#10909,#10907,#1285,.T.);
#13983=EDGE_CURVE('',#10908,#10910,#1286,.T.);
#13984=EDGE_CURVE('',#10911,#10912,#6568,.T.);
#13985=EDGE_CURVE('',#10911,#10909,#1287,.T.);
#13986=EDGE_CURVE('',#10910,#10912,#1288,.T.);
#13987=EDGE_CURVE('',#10913,#10914,#6569,.T.);
#13988=EDGE_CURVE('',#10913,#10911,#1289,.T.);
#13989=EDGE_CURVE('',#10912,#10914,#1290,.T.);
#13990=EDGE_CURVE('',#10915,#10916,#6570,.T.);
#13991=EDGE_CURVE('',#10915,#10913,#1291,.T.);
#13992=EDGE_CURVE('',#10914,#10916,#1292,.T.);
#13993=EDGE_CURVE('',#10917,#10918,#6571,.T.);
#13994=EDGE_CURVE('',#10917,#10915,#1293,.T.);
#13995=EDGE_CURVE('',#10916,#10918,#1294,.T.);
#13996=EDGE_CURVE('',#10919,#10920,#6572,.T.);
#13997=EDGE_CURVE('',#10919,#10917,#1295,.T.);
#13998=EDGE_CURVE('',#10918,#10920,#1296,.T.);
#13999=EDGE_CURVE('',#10921,#10922,#6573,.T.);
#14000=EDGE_CURVE('',#10921,#10919,#1297,.T.);
#14001=EDGE_CURVE('',#10920,#10922,#1298,.T.);
#14002=EDGE_CURVE('',#10923,#10924,#6574,.T.);
#14003=EDGE_CURVE('',#10923,#10921,#1299,.T.);
#14004=EDGE_CURVE('',#10922,#10924,#1300,.T.);
#14005=EDGE_CURVE('',#10925,#10926,#6575,.T.);
#14006=EDGE_CURVE('',#10925,#10923,#1301,.T.);
#14007=EDGE_CURVE('',#10924,#10926,#1302,.T.);
#14008=EDGE_CURVE('',#10927,#10928,#6576,.T.);
#14009=EDGE_CURVE('',#10927,#10925,#1303,.T.);
#14010=EDGE_CURVE('',#10926,#10928,#1304,.T.);
#14011=EDGE_CURVE('',#10929,#10930,#6577,.T.);
#14012=EDGE_CURVE('',#10929,#10927,#1305,.T.);
#14013=EDGE_CURVE('',#10928,#10930,#1306,.T.);
#14014=EDGE_CURVE('',#10931,#10932,#6578,.T.);
#14015=EDGE_CURVE('',#10931,#10929,#1307,.T.);
#14016=EDGE_CURVE('',#10930,#10932,#1308,.T.);
#14017=EDGE_CURVE('',#10933,#10934,#6579,.T.);
#14018=EDGE_CURVE('',#10933,#10931,#1309,.T.);
#14019=EDGE_CURVE('',#10932,#10934,#1310,.T.);
#14020=EDGE_CURVE('',#10935,#10936,#6580,.T.);
#14021=EDGE_CURVE('',#10935,#10933,#1311,.T.);
#14022=EDGE_CURVE('',#10934,#10936,#1312,.T.);
#14023=EDGE_CURVE('',#10937,#10938,#6581,.T.);
#14024=EDGE_CURVE('',#10937,#10935,#1313,.T.);
#14025=EDGE_CURVE('',#10936,#10938,#1314,.T.);
#14026=EDGE_CURVE('',#10939,#10940,#6582,.T.);
#14027=EDGE_CURVE('',#10939,#10937,#1315,.T.);
#14028=EDGE_CURVE('',#10938,#10940,#1316,.T.);
#14029=EDGE_CURVE('',#10941,#10942,#6583,.T.);
#14030=EDGE_CURVE('',#10941,#10939,#1317,.T.);
#14031=EDGE_CURVE('',#10940,#10942,#1318,.T.);
#14032=EDGE_CURVE('',#10943,#10944,#6584,.T.);
#14033=EDGE_CURVE('',#10943,#10941,#1319,.T.);
#14034=EDGE_CURVE('',#10942,#10944,#1320,.T.);
#14035=EDGE_CURVE('',#10945,#10946,#6585,.T.);
#14036=EDGE_CURVE('',#10947,#10945,#9048,.T.);
#14037=EDGE_CURVE('',#10947,#10943,#1321,.T.);
#14038=EDGE_CURVE('',#10944,#10946,#1322,.T.);
#14039=EDGE_CURVE('',#10948,#10949,#6586,.T.);
#14040=EDGE_CURVE('',#10948,#10950,#1323,.T.);
#14041=EDGE_CURVE('',#10951,#10950,#9049,.T.);
#14042=EDGE_CURVE('',#10949,#10951,#1324,.T.);
#14043=EDGE_CURVE('',#10952,#10953,#6587,.T.);
#14044=EDGE_CURVE('',#10952,#10948,#1325,.T.);
#14045=EDGE_CURVE('',#10953,#10949,#1326,.T.);
#14046=EDGE_CURVE('',#10954,#10955,#6588,.T.);
#14047=EDGE_CURVE('',#10954,#10952,#1327,.T.);
#14048=EDGE_CURVE('',#10955,#10953,#1328,.T.);
#14049=EDGE_CURVE('',#10956,#10957,#6589,.T.);
#14050=EDGE_CURVE('',#10956,#10954,#1329,.T.);
#14051=EDGE_CURVE('',#10957,#10955,#1330,.T.);
#14052=EDGE_CURVE('',#10958,#10959,#6590,.T.);
#14053=EDGE_CURVE('',#10958,#10956,#1331,.T.);
#14054=EDGE_CURVE('',#10959,#10957,#1332,.T.);
#14055=EDGE_CURVE('',#10960,#10961,#6591,.T.);
#14056=EDGE_CURVE('',#10960,#10958,#1333,.T.);
#14057=EDGE_CURVE('',#10961,#10959,#1334,.T.);
#14058=EDGE_CURVE('',#10962,#10963,#6592,.T.);
#14059=EDGE_CURVE('',#10962,#10960,#1335,.T.);
#14060=EDGE_CURVE('',#10963,#10961,#1336,.T.);
#14061=EDGE_CURVE('',#10964,#10965,#6593,.T.);
#14062=EDGE_CURVE('',#10964,#10962,#1337,.T.);
#14063=EDGE_CURVE('',#10965,#10963,#1338,.T.);
#14064=EDGE_CURVE('',#10966,#10967,#6594,.T.);
#14065=EDGE_CURVE('',#10966,#10964,#1339,.T.);
#14066=EDGE_CURVE('',#10967,#10965,#1340,.T.);
#14067=EDGE_CURVE('',#10968,#10969,#6595,.T.);
#14068=EDGE_CURVE('',#10968,#10966,#1341,.T.);
#14069=EDGE_CURVE('',#10969,#10967,#1342,.T.);
#14070=EDGE_CURVE('',#10970,#10971,#6596,.T.);
#14071=EDGE_CURVE('',#10970,#10968,#1343,.T.);
#14072=EDGE_CURVE('',#10971,#10969,#1344,.T.);
#14073=EDGE_CURVE('',#10972,#10973,#6597,.T.);
#14074=EDGE_CURVE('',#10972,#10970,#1345,.T.);
#14075=EDGE_CURVE('',#10973,#10971,#1346,.T.);
#14076=EDGE_CURVE('',#10974,#10975,#6598,.T.);
#14077=EDGE_CURVE('',#10974,#10972,#1347,.T.);
#14078=EDGE_CURVE('',#10975,#10973,#1348,.T.);
#14079=EDGE_CURVE('',#10976,#10977,#6599,.T.);
#14080=EDGE_CURVE('',#10976,#10974,#1349,.T.);
#14081=EDGE_CURVE('',#10977,#10975,#1350,.T.);
#14082=EDGE_CURVE('',#10978,#10979,#6600,.T.);
#14083=EDGE_CURVE('',#10978,#10976,#1351,.T.);
#14084=EDGE_CURVE('',#10979,#10977,#1352,.T.);
#14085=EDGE_CURVE('',#10980,#10981,#6601,.T.);
#14086=EDGE_CURVE('',#10980,#10978,#1353,.T.);
#14087=EDGE_CURVE('',#10981,#10979,#1354,.T.);
#14088=EDGE_CURVE('',#10982,#10983,#6602,.T.);
#14089=EDGE_CURVE('',#10982,#10980,#1355,.T.);
#14090=EDGE_CURVE('',#10983,#10981,#1356,.T.);
#14091=EDGE_CURVE('',#10984,#10985,#6603,.T.);
#14092=EDGE_CURVE('',#10984,#10982,#1357,.T.);
#14093=EDGE_CURVE('',#10985,#10983,#1358,.T.);
#14094=EDGE_CURVE('',#10986,#10987,#6604,.T.);
#14095=EDGE_CURVE('',#10986,#10984,#1359,.T.);
#14096=EDGE_CURVE('',#10987,#10985,#1360,.T.);
#14097=EDGE_CURVE('',#10988,#10989,#6605,.T.);
#14098=EDGE_CURVE('',#10988,#10986,#1361,.T.);
#14099=EDGE_CURVE('',#10989,#10987,#1362,.T.);
#14100=EDGE_CURVE('',#10990,#10991,#6606,.T.);
#14101=EDGE_CURVE('',#10990,#10988,#1363,.T.);
#14102=EDGE_CURVE('',#10991,#10989,#1364,.T.);
#14103=EDGE_CURVE('',#10992,#10993,#6607,.T.);
#14104=EDGE_CURVE('',#10992,#10990,#1365,.T.);
#14105=EDGE_CURVE('',#10993,#10991,#1366,.T.);
#14106=EDGE_CURVE('',#10950,#10947,#1367,.T.);
#14107=EDGE_CURVE('',#10994,#10947,#9050,.T.);
#14108=EDGE_CURVE('',#10994,#10951,#1368,.T.);
#14109=EDGE_CURVE('',#10946,#10994,#1369,.T.);
#14110=EDGE_CURVE('',#10995,#10902,#1370,.T.);
#14111=EDGE_CURVE('',#10995,#10993,#1371,.T.);
#14112=EDGE_CURVE('',#10899,#10996,#1372,.T.);
#14113=EDGE_CURVE('',#10996,#10995,#9051,.T.);
#14114=EDGE_CURVE('',#10996,#10992,#1373,.T.);
#14115=EDGE_CURVE('',#10945,#10994,#9052,.T.);
#14116=EDGE_CURVE('',#10945,#10997,#9053,.T.);
#14117=EDGE_CURVE('',#10997,#10997,#9054,.T.);
#14118=EDGE_CURVE('',#10998,#10998,#9055,.T.);
#14119=EDGE_CURVE('',#10999,#11000,#6608,.T.);
#14120=EDGE_CURVE('',#11000,#11000,#9056,.T.);
#14121=EDGE_CURVE('',#11001,#11002,#6609,.T.);
#14122=EDGE_CURVE('',#11001,#11003,#6610,.T.);
#14123=EDGE_CURVE('',#11003,#11004,#6611,.T.);
#14124=EDGE_CURVE('',#11002,#11004,#6612,.T.);
#14125=EDGE_CURVE('',#11005,#11001,#6613,.T.);
#14126=EDGE_CURVE('',#11005,#11006,#6614,.T.);
#14127=EDGE_CURVE('',#11006,#11003,#6615,.T.);
#14128=EDGE_CURVE('',#11007,#11005,#6616,.T.);
#14129=EDGE_CURVE('',#11007,#11008,#6617,.T.);
#14130=EDGE_CURVE('',#11008,#11006,#6618,.T.);
#14131=EDGE_CURVE('',#11009,#11007,#6619,.T.);
#14132=EDGE_CURVE('',#11009,#11010,#6620,.T.);
#14133=EDGE_CURVE('',#11010,#11008,#6621,.T.);
#14134=EDGE_CURVE('',#11011,#11009,#6622,.T.);
#14135=EDGE_CURVE('',#11011,#11012,#6623,.T.);
#14136=EDGE_CURVE('',#11012,#11010,#6624,.T.);
#14137=EDGE_CURVE('',#11002,#11011,#6625,.T.);
#14138=EDGE_CURVE('',#11004,#11012,#6626,.T.);
#14139=EDGE_CURVE('',#11013,#11014,#6627,.T.);
#14140=EDGE_CURVE('',#11013,#11015,#6628,.T.);
#14141=EDGE_CURVE('',#11016,#11015,#6629,.T.);
#14142=EDGE_CURVE('',#11014,#11016,#6630,.T.);
#14143=EDGE_CURVE('',#11014,#11017,#9057,.T.);
#14144=EDGE_CURVE('',#11016,#11017,#6631,.T.);
#14145=EDGE_CURVE('',#11017,#11018,#6632,.T.);
#14146=EDGE_CURVE('',#11015,#11018,#6633,.T.);
#14147=EDGE_CURVE('',#11018,#11013,#9058,.T.);
#14148=EDGE_CURVE('',#11019,#11020,#6634,.T.);
#14149=EDGE_CURVE('',#11019,#11021,#6635,.T.);
#14150=EDGE_CURVE('',#11022,#11021,#6636,.T.);
#14151=EDGE_CURVE('',#11020,#11022,#6637,.T.);
#14152=EDGE_CURVE('',#11020,#11023,#9059,.T.);
#14153=EDGE_CURVE('',#11022,#11023,#6638,.T.);
#14154=EDGE_CURVE('',#11023,#11024,#6639,.T.);
#14155=EDGE_CURVE('',#11021,#11024,#6640,.T.);
#14156=EDGE_CURVE('',#11024,#11019,#9060,.T.);
#14157=EDGE_CURVE('',#11025,#11026,#6641,.T.);
#14158=EDGE_CURVE('',#11025,#11027,#6642,.T.);
#14159=EDGE_CURVE('',#11028,#11027,#6643,.T.);
#14160=EDGE_CURVE('',#11026,#11028,#6644,.T.);
#14161=EDGE_CURVE('',#11026,#11029,#9061,.T.);
#14162=EDGE_CURVE('',#11028,#11029,#6645,.T.);
#14163=EDGE_CURVE('',#11029,#11030,#6646,.T.);
#14164=EDGE_CURVE('',#11027,#11030,#6647,.T.);
#14165=EDGE_CURVE('',#11030,#11025,#9062,.T.);
#14166=EDGE_CURVE('',#11031,#11032,#6648,.T.);
#14167=EDGE_CURVE('',#11031,#11033,#6649,.T.);
#14168=EDGE_CURVE('',#11034,#11033,#6650,.T.);
#14169=EDGE_CURVE('',#11032,#11034,#6651,.T.);
#14170=EDGE_CURVE('',#11032,#11035,#9063,.T.);
#14171=EDGE_CURVE('',#11034,#11035,#6652,.T.);
#14172=EDGE_CURVE('',#11035,#11036,#6653,.T.);
#14173=EDGE_CURVE('',#11033,#11036,#6654,.T.);
#14174=EDGE_CURVE('',#11036,#11031,#9064,.T.);
#14175=EDGE_CURVE('',#11037,#11038,#6655,.T.);
#14176=EDGE_CURVE('',#11037,#11039,#6656,.T.);
#14177=EDGE_CURVE('',#11040,#11039,#6657,.T.);
#14178=EDGE_CURVE('',#11038,#11040,#6658,.T.);
#14179=EDGE_CURVE('',#11038,#11041,#9065,.T.);
#14180=EDGE_CURVE('',#11040,#11041,#6659,.T.);
#14181=EDGE_CURVE('',#11041,#11042,#6660,.T.);
#14182=EDGE_CURVE('',#11039,#11042,#6661,.T.);
#14183=EDGE_CURVE('',#11042,#11037,#9066,.T.);
#14184=EDGE_CURVE('',#11043,#11044,#6662,.T.);
#14185=EDGE_CURVE('',#11043,#11045,#6663,.T.);
#14186=EDGE_CURVE('',#11046,#11045,#6664,.T.);
#14187=EDGE_CURVE('',#11044,#11046,#6665,.T.);
#14188=EDGE_CURVE('',#11044,#11047,#9067,.T.);
#14189=EDGE_CURVE('',#11046,#11047,#6666,.T.);
#14190=EDGE_CURVE('',#11047,#11048,#6667,.T.);
#14191=EDGE_CURVE('',#11045,#11048,#6668,.T.);
#14192=EDGE_CURVE('',#11048,#11043,#9068,.T.);
#14193=EDGE_CURVE('',#11049,#11050,#6669,.T.);
#14194=EDGE_CURVE('',#11049,#11051,#6670,.T.);
#14195=EDGE_CURVE('',#11052,#11051,#6671,.T.);
#14196=EDGE_CURVE('',#11050,#11052,#6672,.T.);
#14197=EDGE_CURVE('',#11050,#11053,#9069,.T.);
#14198=EDGE_CURVE('',#11052,#11053,#6673,.T.);
#14199=EDGE_CURVE('',#11053,#11054,#6674,.T.);
#14200=EDGE_CURVE('',#11051,#11054,#6675,.T.);
#14201=EDGE_CURVE('',#11054,#11049,#9070,.T.);
#14202=EDGE_CURVE('',#11055,#11056,#6676,.T.);
#14203=EDGE_CURVE('',#11055,#11057,#6677,.T.);
#14204=EDGE_CURVE('',#11058,#11057,#6678,.T.);
#14205=EDGE_CURVE('',#11056,#11058,#6679,.T.);
#14206=EDGE_CURVE('',#11056,#11059,#9071,.T.);
#14207=EDGE_CURVE('',#11058,#11059,#6680,.T.);
#14208=EDGE_CURVE('',#11059,#11060,#6681,.T.);
#14209=EDGE_CURVE('',#11057,#11060,#6682,.T.);
#14210=EDGE_CURVE('',#11060,#11055,#9072,.T.);
#14211=EDGE_CURVE('',#11061,#11062,#6683,.T.);
#14212=EDGE_CURVE('',#11061,#11063,#6684,.T.);
#14213=EDGE_CURVE('',#11064,#11063,#6685,.T.);
#14214=EDGE_CURVE('',#11062,#11064,#6686,.T.);
#14215=EDGE_CURVE('',#11062,#11065,#9073,.T.);
#14216=EDGE_CURVE('',#11064,#11066,#6687,.T.);
#14217=EDGE_CURVE('',#11065,#11066,#9074,.T.);
#14218=EDGE_CURVE('',#11066,#11067,#6688,.T.);
#14219=EDGE_CURVE('',#11063,#11067,#6689,.T.);
#14220=EDGE_CURVE('',#11067,#11068,#9075,.T.);
#14221=EDGE_CURVE('',#11068,#11061,#9076,.T.);
#14222=EDGE_CURVE('',#11069,#11070,#6690,.T.);
#14223=EDGE_CURVE('',#11069,#11071,#6691,.T.);
#14224=EDGE_CURVE('',#11072,#11071,#6692,.T.);
#14225=EDGE_CURVE('',#11070,#11072,#6693,.T.);
#14226=EDGE_CURVE('',#11070,#11073,#9077,.T.);
#14227=EDGE_CURVE('',#11072,#11073,#6694,.T.);
#14228=EDGE_CURVE('',#11073,#11074,#6695,.T.);
#14229=EDGE_CURVE('',#11071,#11074,#6696,.T.);
#14230=EDGE_CURVE('',#11074,#11069,#9078,.T.);
#14231=EDGE_CURVE('',#11075,#11076,#6697,.T.);
#14232=EDGE_CURVE('',#11075,#11077,#6698,.T.);
#14233=EDGE_CURVE('',#11078,#11077,#6699,.T.);
#14234=EDGE_CURVE('',#11076,#11078,#6700,.T.);
#14235=EDGE_CURVE('',#11076,#11079,#9079,.T.);
#14236=EDGE_CURVE('',#11078,#11079,#6701,.T.);
#14237=EDGE_CURVE('',#11079,#11080,#6702,.T.);
#14238=EDGE_CURVE('',#11077,#11080,#6703,.T.);
#14239=EDGE_CURVE('',#11080,#11075,#9080,.T.);
#14240=EDGE_CURVE('',#11081,#11082,#6704,.T.);
#14241=EDGE_CURVE('',#11081,#11083,#6705,.T.);
#14242=EDGE_CURVE('',#11084,#11083,#6706,.T.);
#14243=EDGE_CURVE('',#11082,#11084,#6707,.T.);
#14244=EDGE_CURVE('',#11082,#11085,#9081,.T.);
#14245=EDGE_CURVE('',#11084,#11085,#6708,.T.);
#14246=EDGE_CURVE('',#11085,#11086,#6709,.T.);
#14247=EDGE_CURVE('',#11083,#11086,#6710,.T.);
#14248=EDGE_CURVE('',#11086,#11081,#9082,.T.);
#14249=EDGE_CURVE('',#11087,#11088,#6711,.T.);
#14250=EDGE_CURVE('',#11087,#11089,#6712,.T.);
#14251=EDGE_CURVE('',#11090,#11089,#6713,.T.);
#14252=EDGE_CURVE('',#11088,#11090,#6714,.T.);
#14253=EDGE_CURVE('',#11088,#11091,#9083,.T.);
#14254=EDGE_CURVE('',#11090,#11091,#6715,.T.);
#14255=EDGE_CURVE('',#11091,#11092,#6716,.T.);
#14256=EDGE_CURVE('',#11089,#11092,#6717,.T.);
#14257=EDGE_CURVE('',#11092,#11087,#9084,.T.);
#14258=EDGE_CURVE('',#11093,#11094,#6718,.T.);
#14259=EDGE_CURVE('',#11093,#11095,#6719,.T.);
#14260=EDGE_CURVE('',#11096,#11095,#6720,.T.);
#14261=EDGE_CURVE('',#11094,#11096,#6721,.T.);
#14262=EDGE_CURVE('',#11094,#11097,#9085,.T.);
#14263=EDGE_CURVE('',#11096,#11097,#6722,.T.);
#14264=EDGE_CURVE('',#11097,#11098,#6723,.T.);
#14265=EDGE_CURVE('',#11095,#11098,#6724,.T.);
#14266=EDGE_CURVE('',#11098,#11093,#9086,.T.);
#14267=EDGE_CURVE('',#11099,#11100,#6725,.T.);
#14268=EDGE_CURVE('',#11099,#11101,#6726,.T.);
#14269=EDGE_CURVE('',#11102,#11101,#6727,.T.);
#14270=EDGE_CURVE('',#11100,#11102,#6728,.T.);
#14271=EDGE_CURVE('',#11100,#11103,#9087,.T.);
#14272=EDGE_CURVE('',#11102,#11103,#6729,.T.);
#14273=EDGE_CURVE('',#11103,#11104,#6730,.T.);
#14274=EDGE_CURVE('',#11101,#11104,#6731,.T.);
#14275=EDGE_CURVE('',#11104,#11099,#9088,.T.);
#14276=EDGE_CURVE('',#11105,#11106,#6732,.T.);
#14277=EDGE_CURVE('',#11105,#11107,#6733,.T.);
#14278=EDGE_CURVE('',#11108,#11107,#6734,.T.);
#14279=EDGE_CURVE('',#11106,#11108,#6735,.T.);
#14280=EDGE_CURVE('',#11106,#11109,#9089,.T.);
#14281=EDGE_CURVE('',#11108,#11109,#6736,.T.);
#14282=EDGE_CURVE('',#11109,#11110,#6737,.T.);
#14283=EDGE_CURVE('',#11107,#11110,#6738,.T.);
#14284=EDGE_CURVE('',#11110,#11105,#9090,.T.);
#14285=EDGE_CURVE('',#11111,#11112,#6739,.T.);
#14286=EDGE_CURVE('',#11111,#11113,#6740,.T.);
#14287=EDGE_CURVE('',#11114,#11113,#6741,.T.);
#14288=EDGE_CURVE('',#11112,#11114,#6742,.T.);
#14289=EDGE_CURVE('',#11112,#11115,#9091,.T.);
#14290=EDGE_CURVE('',#11114,#11115,#6743,.T.);
#14291=EDGE_CURVE('',#11115,#11116,#6744,.T.);
#14292=EDGE_CURVE('',#11113,#11116,#6745,.T.);
#14293=EDGE_CURVE('',#11116,#11111,#9092,.T.);
#14294=EDGE_CURVE('',#11117,#11118,#6746,.T.);
#14295=EDGE_CURVE('',#11117,#11119,#6747,.T.);
#14296=EDGE_CURVE('',#11120,#11119,#6748,.T.);
#14297=EDGE_CURVE('',#11118,#11120,#6749,.T.);
#14298=EDGE_CURVE('',#11118,#11121,#9093,.T.);
#14299=EDGE_CURVE('',#11120,#11121,#6750,.T.);
#14300=EDGE_CURVE('',#11121,#11122,#6751,.T.);
#14301=EDGE_CURVE('',#11119,#11122,#6752,.T.);
#14302=EDGE_CURVE('',#11122,#11117,#9094,.T.);
#14303=EDGE_CURVE('',#11123,#11124,#6753,.T.);
#14304=EDGE_CURVE('',#11123,#11125,#6754,.T.);
#14305=EDGE_CURVE('',#11126,#11125,#6755,.T.);
#14306=EDGE_CURVE('',#11124,#11126,#6756,.T.);
#14307=EDGE_CURVE('',#11124,#11127,#9095,.T.);
#14308=EDGE_CURVE('',#11126,#11127,#6757,.T.);
#14309=EDGE_CURVE('',#11127,#11128,#6758,.T.);
#14310=EDGE_CURVE('',#11125,#11128,#6759,.T.);
#14311=EDGE_CURVE('',#11128,#11123,#9096,.T.);
#14312=EDGE_CURVE('',#11129,#11130,#6760,.T.);
#14313=EDGE_CURVE('',#11129,#11131,#6761,.T.);
#14314=EDGE_CURVE('',#11132,#11131,#6762,.T.);
#14315=EDGE_CURVE('',#11130,#11132,#6763,.T.);
#14316=EDGE_CURVE('',#11130,#11133,#9097,.T.);
#14317=EDGE_CURVE('',#11132,#11133,#6764,.T.);
#14318=EDGE_CURVE('',#11133,#11134,#6765,.T.);
#14319=EDGE_CURVE('',#11131,#11134,#6766,.T.);
#14320=EDGE_CURVE('',#11134,#11129,#9098,.T.);
#14321=EDGE_CURVE('',#11135,#11136,#6767,.T.);
#14322=EDGE_CURVE('',#11135,#11137,#6768,.T.);
#14323=EDGE_CURVE('',#11138,#11137,#6769,.T.);
#14324=EDGE_CURVE('',#11136,#11138,#6770,.T.);
#14325=EDGE_CURVE('',#11136,#11139,#9099,.T.);
#14326=EDGE_CURVE('',#11138,#11139,#6771,.T.);
#14327=EDGE_CURVE('',#11139,#11140,#6772,.T.);
#14328=EDGE_CURVE('',#11137,#11140,#6773,.T.);
#14329=EDGE_CURVE('',#11140,#11135,#9100,.T.);
#14330=EDGE_CURVE('',#11141,#11142,#6774,.T.);
#14331=EDGE_CURVE('',#11141,#11143,#6775,.T.);
#14332=EDGE_CURVE('',#11144,#11143,#6776,.T.);
#14333=EDGE_CURVE('',#11142,#11144,#6777,.T.);
#14334=EDGE_CURVE('',#11142,#11145,#9101,.T.);
#14335=EDGE_CURVE('',#11144,#11145,#6778,.T.);
#14336=EDGE_CURVE('',#11145,#11146,#6779,.T.);
#14337=EDGE_CURVE('',#11143,#11146,#6780,.T.);
#14338=EDGE_CURVE('',#11146,#11141,#9102,.T.);
#14339=EDGE_CURVE('',#11147,#11148,#6781,.T.);
#14340=EDGE_CURVE('',#11147,#11149,#6782,.T.);
#14341=EDGE_CURVE('',#11150,#11149,#6783,.T.);
#14342=EDGE_CURVE('',#11148,#11150,#6784,.T.);
#14343=EDGE_CURVE('',#11148,#11151,#9103,.T.);
#14344=EDGE_CURVE('',#11150,#11151,#6785,.T.);
#14345=EDGE_CURVE('',#11151,#11152,#6786,.T.);
#14346=EDGE_CURVE('',#11149,#11152,#6787,.T.);
#14347=EDGE_CURVE('',#11152,#11147,#9104,.T.);
#14348=EDGE_CURVE('',#11153,#11154,#6788,.T.);
#14349=EDGE_CURVE('',#11153,#11155,#6789,.T.);
#14350=EDGE_CURVE('',#11156,#11155,#6790,.T.);
#14351=EDGE_CURVE('',#11154,#11156,#6791,.T.);
#14352=EDGE_CURVE('',#11154,#11157,#9105,.T.);
#14353=EDGE_CURVE('',#11156,#11157,#6792,.T.);
#14354=EDGE_CURVE('',#11157,#11158,#6793,.T.);
#14355=EDGE_CURVE('',#11155,#11158,#6794,.T.);
#14356=EDGE_CURVE('',#11158,#11153,#9106,.T.);
#14357=EDGE_CURVE('',#11159,#11160,#6795,.T.);
#14358=EDGE_CURVE('',#11159,#11161,#6796,.T.);
#14359=EDGE_CURVE('',#11162,#11161,#6797,.T.);
#14360=EDGE_CURVE('',#11160,#11162,#6798,.T.);
#14361=EDGE_CURVE('',#11160,#11163,#9107,.T.);
#14362=EDGE_CURVE('',#11162,#11163,#6799,.T.);
#14363=EDGE_CURVE('',#11163,#11164,#6800,.T.);
#14364=EDGE_CURVE('',#11161,#11164,#6801,.T.);
#14365=EDGE_CURVE('',#11164,#11159,#9108,.T.);
#14366=EDGE_CURVE('',#11165,#11166,#6802,.T.);
#14367=EDGE_CURVE('',#11165,#11167,#6803,.T.);
#14368=EDGE_CURVE('',#11168,#11167,#6804,.T.);
#14369=EDGE_CURVE('',#11166,#11168,#6805,.T.);
#14370=EDGE_CURVE('',#11166,#11169,#9109,.T.);
#14371=EDGE_CURVE('',#11168,#11169,#6806,.T.);
#14372=EDGE_CURVE('',#11169,#11170,#6807,.T.);
#14373=EDGE_CURVE('',#11167,#11170,#6808,.T.);
#14374=EDGE_CURVE('',#11170,#11165,#9110,.T.);
#14375=EDGE_CURVE('',#11171,#11172,#9111,.T.);
#14376=EDGE_CURVE('',#11171,#11173,#6809,.T.);
#14377=EDGE_CURVE('',#11173,#11172,#6810,.T.);
#14378=EDGE_CURVE('',#11174,#11171,#6811,.T.);
#14379=EDGE_CURVE('',#11174,#11175,#6812,.T.);
#14380=EDGE_CURVE('',#11173,#11175,#6813,.T.);
#14381=EDGE_CURVE('',#11172,#11176,#6814,.T.);
#14382=EDGE_CURVE('',#11175,#11176,#6815,.T.);
#14383=EDGE_CURVE('',#11176,#11174,#9112,.T.);
#14384=EDGE_CURVE('',#11177,#11178,#6816,.T.);
#14385=EDGE_CURVE('',#11177,#11179,#6817,.T.);
#14386=EDGE_CURVE('',#11180,#11179,#6818,.T.);
#14387=EDGE_CURVE('',#11178,#11180,#6819,.T.);
#14388=EDGE_CURVE('',#11178,#11181,#9113,.T.);
#14389=EDGE_CURVE('',#11180,#11181,#6820,.T.);
#14390=EDGE_CURVE('',#11181,#11182,#6821,.T.);
#14391=EDGE_CURVE('',#11179,#11182,#6822,.T.);
#14392=EDGE_CURVE('',#11182,#11177,#9114,.T.);
#14393=EDGE_CURVE('',#11183,#11184,#6823,.T.);
#14394=EDGE_CURVE('',#11183,#11185,#6824,.T.);
#14395=EDGE_CURVE('',#11186,#11185,#6825,.T.);
#14396=EDGE_CURVE('',#11184,#11186,#6826,.T.);
#14397=EDGE_CURVE('',#11184,#11187,#9115,.T.);
#14398=EDGE_CURVE('',#11186,#11187,#6827,.T.);
#14399=EDGE_CURVE('',#11187,#11188,#6828,.T.);
#14400=EDGE_CURVE('',#11185,#11188,#6829,.T.);
#14401=EDGE_CURVE('',#11188,#11183,#9116,.T.);
#14402=EDGE_CURVE('',#11189,#11190,#6830,.T.);
#14403=EDGE_CURVE('',#11189,#11191,#6831,.T.);
#14404=EDGE_CURVE('',#11192,#11191,#6832,.T.);
#14405=EDGE_CURVE('',#11190,#11192,#6833,.T.);
#14406=EDGE_CURVE('',#11190,#11193,#9117,.T.);
#14407=EDGE_CURVE('',#11192,#11193,#6834,.T.);
#14408=EDGE_CURVE('',#11193,#11194,#6835,.T.);
#14409=EDGE_CURVE('',#11191,#11194,#6836,.T.);
#14410=EDGE_CURVE('',#11194,#11189,#9118,.T.);
#14411=EDGE_CURVE('',#11195,#11196,#6837,.T.);
#14412=EDGE_CURVE('',#11195,#11197,#6838,.T.);
#14413=EDGE_CURVE('',#11198,#11197,#6839,.T.);
#14414=EDGE_CURVE('',#11196,#11198,#6840,.T.);
#14415=EDGE_CURVE('',#11196,#11199,#9119,.T.);
#14416=EDGE_CURVE('',#11198,#11199,#6841,.T.);
#14417=EDGE_CURVE('',#11199,#11200,#6842,.T.);
#14418=EDGE_CURVE('',#11197,#11200,#6843,.T.);
#14419=EDGE_CURVE('',#11200,#11195,#9120,.T.);
#14420=EDGE_CURVE('',#11201,#11202,#6844,.T.);
#14421=EDGE_CURVE('',#11201,#11203,#6845,.T.);
#14422=EDGE_CURVE('',#11204,#11203,#6846,.T.);
#14423=EDGE_CURVE('',#11202,#11204,#6847,.T.);
#14424=EDGE_CURVE('',#11202,#11205,#9121,.T.);
#14425=EDGE_CURVE('',#11204,#11205,#6848,.T.);
#14426=EDGE_CURVE('',#11205,#11206,#6849,.T.);
#14427=EDGE_CURVE('',#11203,#11206,#6850,.T.);
#14428=EDGE_CURVE('',#11206,#11201,#9122,.T.);
#14429=EDGE_CURVE('',#11207,#11208,#6851,.T.);
#14430=EDGE_CURVE('',#11207,#11209,#6852,.T.);
#14431=EDGE_CURVE('',#11210,#11209,#6853,.T.);
#14432=EDGE_CURVE('',#11208,#11210,#6854,.T.);
#14433=EDGE_CURVE('',#11208,#11211,#9123,.T.);
#14434=EDGE_CURVE('',#11210,#11211,#6855,.T.);
#14435=EDGE_CURVE('',#11211,#11212,#6856,.T.);
#14436=EDGE_CURVE('',#11209,#11212,#6857,.T.);
#14437=EDGE_CURVE('',#11212,#11207,#9124,.T.);
#14438=EDGE_CURVE('',#11213,#11214,#6858,.T.);
#14439=EDGE_CURVE('',#11213,#11215,#6859,.T.);
#14440=EDGE_CURVE('',#11216,#11215,#6860,.T.);
#14441=EDGE_CURVE('',#11214,#11216,#6861,.T.);
#14442=EDGE_CURVE('',#11214,#11217,#9125,.T.);
#14443=EDGE_CURVE('',#11216,#11217,#6862,.T.);
#14444=EDGE_CURVE('',#11217,#11218,#6863,.T.);
#14445=EDGE_CURVE('',#11215,#11218,#6864,.T.);
#14446=EDGE_CURVE('',#11218,#11213,#9126,.T.);
#14447=EDGE_CURVE('',#11219,#11220,#6865,.T.);
#14448=EDGE_CURVE('',#11219,#11221,#6866,.T.);
#14449=EDGE_CURVE('',#11222,#11221,#6867,.T.);
#14450=EDGE_CURVE('',#11220,#11222,#6868,.T.);
#14451=EDGE_CURVE('',#11220,#11223,#9127,.T.);
#14452=EDGE_CURVE('',#11222,#11223,#6869,.T.);
#14453=EDGE_CURVE('',#11223,#11224,#6870,.T.);
#14454=EDGE_CURVE('',#11221,#11224,#6871,.T.);
#14455=EDGE_CURVE('',#11224,#11219,#9128,.T.);
#14456=EDGE_CURVE('',#11225,#11226,#6872,.T.);
#14457=EDGE_CURVE('',#11225,#11227,#6873,.T.);
#14458=EDGE_CURVE('',#11228,#11227,#6874,.T.);
#14459=EDGE_CURVE('',#11226,#11228,#6875,.T.);
#14460=EDGE_CURVE('',#11226,#11229,#9129,.T.);
#14461=EDGE_CURVE('',#11228,#11229,#6876,.T.);
#14462=EDGE_CURVE('',#11229,#11230,#6877,.T.);
#14463=EDGE_CURVE('',#11227,#11230,#6878,.T.);
#14464=EDGE_CURVE('',#11230,#11225,#9130,.T.);
#14465=EDGE_CURVE('',#11231,#11231,#9131,.T.);
#14466=EDGE_CURVE('',#10901,#11231,#6879,.T.);
#14467=EDGE_CURVE('',#11232,#11232,#9132,.T.);
#14468=EDGE_CURVE('',#11232,#10998,#6880,.T.);
#14469=EDGE_CURVE('',#11223,#11014,#9133,.T.);
#14470=EDGE_CURVE('',#11023,#11220,#9134,.T.);
#14471=EDGE_CURVE('',#11217,#11020,#9135,.T.);
#14472=EDGE_CURVE('',#11029,#11214,#9136,.T.);
#14473=EDGE_CURVE('',#11211,#11026,#9137,.T.);
#14474=EDGE_CURVE('',#11035,#11208,#9138,.T.);
#14475=EDGE_CURVE('',#11205,#11032,#9139,.T.);
#14476=EDGE_CURVE('',#11041,#11202,#9140,.T.);
#14477=EDGE_CURVE('',#11199,#11038,#9141,.T.);
#14478=EDGE_CURVE('',#11047,#11196,#9142,.T.);
#14479=EDGE_CURVE('',#11193,#11044,#9143,.T.);
#14480=EDGE_CURVE('',#11053,#11190,#9144,.T.);
#14481=EDGE_CURVE('',#11187,#11050,#9145,.T.);
#14482=EDGE_CURVE('',#11059,#11184,#9146,.T.);
#14483=EDGE_CURVE('',#11181,#11056,#9147,.T.);
#14484=EDGE_CURVE('',#11066,#11178,#9148,.T.);
#14485=EDGE_CURVE('',#11068,#11232,#6881,.T.);
#14486=EDGE_CURVE('',#11073,#11062,#9149,.T.);
#14487=EDGE_CURVE('',#11169,#11070,#9150,.T.);
#14488=EDGE_CURVE('',#11079,#11166,#9151,.T.);
#14489=EDGE_CURVE('',#11163,#11076,#9152,.T.);
#14490=EDGE_CURVE('',#11085,#11160,#9153,.T.);
#14491=EDGE_CURVE('',#11157,#11082,#9154,.T.);
#14492=EDGE_CURVE('',#11091,#11154,#9155,.T.);
#14493=EDGE_CURVE('',#11151,#11088,#9156,.T.);
#14494=EDGE_CURVE('',#11097,#11148,#9157,.T.);
#14495=EDGE_CURVE('',#11145,#11094,#9158,.T.);
#14496=EDGE_CURVE('',#11103,#11142,#9159,.T.);
#14497=EDGE_CURVE('',#11139,#11100,#9160,.T.);
#14498=EDGE_CURVE('',#11109,#11136,#9161,.T.);
#14499=EDGE_CURVE('',#11133,#11106,#9162,.T.);
#14500=EDGE_CURVE('',#11115,#11130,#9163,.T.);
#14501=EDGE_CURVE('',#11127,#11112,#9164,.T.);
#14502=EDGE_CURVE('',#11121,#11124,#9165,.T.);
#14503=EDGE_CURVE('',#11172,#11118,#9166,.T.);
#14504=EDGE_CURVE('',#11229,#11171,#9167,.T.);
#14505=EDGE_CURVE('',#11017,#11226,#9168,.T.);
#14506=EDGE_CURVE('',#11233,#11233,#9169,.T.);
#14507=EDGE_CURVE('',#11233,#11065,#6882,.T.);
#14508=EDGE_CURVE('',#11234,#11235,#6883,.T.);
#14509=EDGE_CURVE('',#11234,#11236,#1374,.T.);
#14510=EDGE_CURVE('',#11237,#11236,#9170,.T.);
#14511=EDGE_CURVE('',#11235,#11237,#1375,.T.);
#14512=EDGE_CURVE('',#11238,#11239,#6884,.T.);
#14513=EDGE_CURVE('',#11238,#11234,#1376,.T.);
#14514=EDGE_CURVE('',#11239,#11235,#1377,.T.);
#14515=EDGE_CURVE('',#11240,#11241,#6885,.T.);
#14516=EDGE_CURVE('',#11240,#11238,#1378,.T.);
#14517=EDGE_CURVE('',#11241,#11239,#1379,.T.);
#14518=EDGE_CURVE('',#11242,#11243,#6886,.T.);
#14519=EDGE_CURVE('',#11242,#11240,#1380,.T.);
#14520=EDGE_CURVE('',#11243,#11241,#1381,.T.);
#14521=EDGE_CURVE('',#11244,#11245,#6887,.T.);
#14522=EDGE_CURVE('',#11244,#11242,#1382,.T.);
#14523=EDGE_CURVE('',#11245,#11243,#1383,.T.);
#14524=EDGE_CURVE('',#11246,#11247,#6888,.T.);
#14525=EDGE_CURVE('',#11246,#11244,#1384,.T.);
#14526=EDGE_CURVE('',#11247,#11245,#1385,.T.);
#14527=EDGE_CURVE('',#11248,#11249,#6889,.T.);
#14528=EDGE_CURVE('',#11248,#11246,#1386,.T.);
#14529=EDGE_CURVE('',#11249,#11247,#1387,.T.);
#14530=EDGE_CURVE('',#11250,#11251,#6890,.T.);
#14531=EDGE_CURVE('',#11252,#11250,#9171,.T.);
#14532=EDGE_CURVE('',#11252,#11248,#1388,.T.);
#14533=EDGE_CURVE('',#11251,#11249,#1389,.T.);
#14534=EDGE_CURVE('',#11253,#11254,#6891,.T.);
#14535=EDGE_CURVE('',#11253,#11255,#1390,.T.);
#14536=EDGE_CURVE('',#11255,#11256,#9172,.F.);
#14537=EDGE_CURVE('',#11256,#11254,#1391,.T.);
#14538=EDGE_CURVE('',#11257,#11258,#6892,.T.);
#14539=EDGE_CURVE('',#11257,#11253,#1392,.T.);
#14540=EDGE_CURVE('',#11254,#11258,#1393,.T.);
#14541=EDGE_CURVE('',#11259,#11260,#6893,.T.);
#14542=EDGE_CURVE('',#11259,#11257,#1394,.T.);
#14543=EDGE_CURVE('',#11258,#11260,#1395,.T.);
#14544=EDGE_CURVE('',#11261,#11262,#6894,.T.);
#14545=EDGE_CURVE('',#11261,#11259,#1396,.T.);
#14546=EDGE_CURVE('',#11260,#11262,#1397,.T.);
#14547=EDGE_CURVE('',#11263,#11264,#6895,.T.);
#14548=EDGE_CURVE('',#11263,#11261,#1398,.T.);
#14549=EDGE_CURVE('',#11262,#11264,#1399,.T.);
#14550=EDGE_CURVE('',#11265,#11266,#6896,.T.);
#14551=EDGE_CURVE('',#11265,#11263,#1400,.T.);
#14552=EDGE_CURVE('',#11264,#11266,#1401,.T.);
#14553=EDGE_CURVE('',#11267,#11268,#6897,.T.);
#14554=EDGE_CURVE('',#11267,#11265,#1402,.T.);
#14555=EDGE_CURVE('',#11266,#11268,#1403,.T.);
#14556=EDGE_CURVE('',#11269,#11270,#6898,.T.);
#14557=EDGE_CURVE('',#11269,#11267,#1404,.T.);
#14558=EDGE_CURVE('',#11268,#11270,#1405,.T.);
#14559=EDGE_CURVE('',#11271,#11272,#6899,.T.);
#14560=EDGE_CURVE('',#11271,#11269,#1406,.T.);
#14561=EDGE_CURVE('',#11270,#11272,#1407,.T.);
#14562=EDGE_CURVE('',#11273,#11274,#6900,.T.);
#14563=EDGE_CURVE('',#11273,#11275,#1408,.T.);
#14564=EDGE_CURVE('',#11276,#11275,#9173,.T.);
#14565=EDGE_CURVE('',#11274,#11276,#1409,.T.);
#14566=EDGE_CURVE('',#11277,#11278,#6901,.T.);
#14567=EDGE_CURVE('',#11277,#11273,#1410,.T.);
#14568=EDGE_CURVE('',#11278,#11274,#1411,.T.);
#14569=EDGE_CURVE('',#11279,#11280,#6902,.T.);
#14570=EDGE_CURVE('',#11279,#11277,#1412,.T.);
#14571=EDGE_CURVE('',#11280,#11278,#1413,.T.);
#14572=EDGE_CURVE('',#11281,#11282,#6903,.T.);
#14573=EDGE_CURVE('',#11281,#11279,#1414,.T.);
#14574=EDGE_CURVE('',#11282,#11280,#1415,.T.);
#14575=EDGE_CURVE('',#11283,#11284,#6904,.T.);
#14576=EDGE_CURVE('',#11283,#11281,#1416,.T.);
#14577=EDGE_CURVE('',#11284,#11282,#1417,.T.);
#14578=EDGE_CURVE('',#11285,#11286,#6905,.T.);
#14579=EDGE_CURVE('',#11285,#11283,#1418,.T.);
#14580=EDGE_CURVE('',#11286,#11284,#1419,.T.);
#14581=EDGE_CURVE('',#11287,#11288,#6906,.T.);
#14582=EDGE_CURVE('',#11287,#11285,#1420,.T.);
#14583=EDGE_CURVE('',#11288,#11286,#1421,.T.);
#14584=EDGE_CURVE('',#11289,#11290,#6907,.T.);
#14585=EDGE_CURVE('',#11289,#11287,#1422,.T.);
#14586=EDGE_CURVE('',#11290,#11288,#1423,.T.);
#14587=EDGE_CURVE('',#11291,#11292,#6908,.T.);
#14588=EDGE_CURVE('',#11291,#11289,#1424,.T.);
#14589=EDGE_CURVE('',#11292,#11290,#1425,.T.);
#14590=EDGE_CURVE('',#11275,#11293,#1426,.T.);
#14591=EDGE_CURVE('',#11294,#11293,#9174,.F.);
#14592=EDGE_CURVE('',#11295,#11294,#9175,.F.);
#14593=EDGE_CURVE('',#11295,#11276,#1427,.T.);
#14594=EDGE_CURVE('',#11272,#11295,#1428,.T.);
#14595=EDGE_CURVE('',#11296,#11256,#1429,.T.);
#14596=EDGE_CURVE('',#11296,#11292,#1430,.T.);
#14597=EDGE_CURVE('',#11297,#11296,#9176,.T.);
#14598=EDGE_CURVE('',#11297,#11291,#1431,.T.);
#14599=EDGE_CURVE('',#11255,#11297,#1432,.T.);
#14600=EDGE_CURVE('',#11293,#11271,#1433,.T.);
#14601=EDGE_CURVE('',#11293,#11295,#9177,.F.);
#14602=EDGE_CURVE('',#11298,#11299,#1434,.T.);
#14603=EDGE_CURVE('',#11300,#11298,#1435,.T.);
#14604=EDGE_CURVE('',#11301,#11300,#1436,.T.);
#14605=EDGE_CURVE('',#11301,#11299,#1437,.T.);
#14606=EDGE_CURVE('',#11299,#11302,#1438,.T.);
#14607=EDGE_CURVE('',#11303,#11301,#1439,.T.);
#14608=EDGE_CURVE('',#11303,#11302,#1440,.T.);
#14609=EDGE_CURVE('',#11302,#11237,#1441,.T.);
#14610=EDGE_CURVE('',#11304,#11303,#1442,.T.);
#14611=EDGE_CURVE('',#11304,#11251,#1443,.T.);
#14612=EDGE_CURVE('',#11300,#11305,#9178,.T.);
#14613=EDGE_CURVE('',#11305,#11300,#9179,.T.);
#14614=EDGE_CURVE('',#11300,#11306,#1444,.T.);
#14615=EDGE_CURVE('',#11306,#11307,#1445,.T.);
#14616=EDGE_CURVE('',#11307,#11252,#1446,.T.);
#14617=EDGE_CURVE('',#11250,#11304,#9180,.T.);
#14618=EDGE_CURVE('',#11236,#11308,#1447,.T.);
#14619=EDGE_CURVE('',#11307,#11308,#1448,.T.);
#14620=EDGE_CURVE('',#11308,#11309,#1449,.T.);
#14621=EDGE_CURVE('',#11306,#11309,#1450,.T.);
#14622=EDGE_CURVE('',#11309,#11298,#1451,.T.);
#14623=EDGE_CURVE('',#11310,#11310,#9181,.T.);
#14624=EDGE_CURVE('',#11310,#11311,#6909,.T.);
#14625=EDGE_CURVE('',#11312,#11311,#1494,.T.);
#14626=EDGE_CURVE('',#11313,#11312,#1495,.T.);
#14627=EDGE_CURVE('',#11314,#11313,#1496,.T.);
#14628=EDGE_CURVE('',#11315,#11314,#1497,.T.);
#14629=EDGE_CURVE('',#11316,#11315,#1498,.T.);
#14630=EDGE_CURVE('',#11317,#11316,#1499,.T.);
#14631=EDGE_CURVE('',#11311,#11317,#1500,.T.);
#14632=EDGE_CURVE('',#11315,#11318,#6910,.T.);
#14633=EDGE_CURVE('',#11318,#11319,#1501,.T.);
#14634=EDGE_CURVE('',#11316,#11319,#6911,.T.);
#14635=EDGE_CURVE('',#11314,#11320,#6912,.T.);
#14636=EDGE_CURVE('',#11320,#11318,#1502,.T.);
#14637=EDGE_CURVE('',#11313,#11321,#6913,.T.);
#14638=EDGE_CURVE('',#11321,#11320,#1503,.T.);
#14639=EDGE_CURVE('',#11322,#11321,#1504,.T.);
#14640=EDGE_CURVE('',#11323,#11322,#1505,.T.);
#14641=EDGE_CURVE('',#11323,#11324,#6914,.T.);
#14642=EDGE_CURVE('',#11324,#11324,#9182,.T.);
#14643=EDGE_CURVE('',#11325,#11323,#1506,.T.);
#14644=EDGE_CURVE('',#11319,#11325,#1507,.T.);
#14645=EDGE_CURVE('',#11312,#11322,#6915,.T.);
#14646=EDGE_CURVE('',#11326,#11326,#9183,.T.);
#14647=EDGE_CURVE('',#11327,#11327,#9184,.T.);
#14648=EDGE_CURVE('',#11328,#11328,#9185,.T.);
#14649=EDGE_CURVE('',#11317,#11325,#6916,.T.);
#14650=EDGE_CURVE('',#11328,#11329,#6917,.T.);
#14651=EDGE_CURVE('',#11329,#11329,#9186,.T.);
#14652=EDGE_CURVE('',#11330,#11330,#9187,.T.);
#14653=EDGE_CURVE('',#11330,#11326,#6918,.T.);
#14654=EDGE_CURVE('',#11331,#11331,#9188,.T.);
#14655=EDGE_CURVE('',#11305,#11331,#6919,.T.);
#14656=EDGE_CURVE('',#11332,#11332,#9189,.T.);
#14657=EDGE_CURVE('',#11327,#11332,#6920,.T.);
#14658=EDGE_CURVE('',#11333,#11333,#9190,.T.);
#14659=EDGE_CURVE('',#11333,#11294,#6921,.T.);
#14660=EDGE_CURVE('',#11334,#11334,#9191,.T.);
#14661=EDGE_CURVE('',#11334,#11330,#6922,.T.);
#14662=ORIENTED_EDGE('',*,*,#11335,.T.);
#14663=ORIENTED_EDGE('',*,*,#11336,.T.);
#14664=ORIENTED_EDGE('',*,*,#11337,.T.);
#14665=ORIENTED_EDGE('',*,*,#11336,.F.);
#14666=ORIENTED_EDGE('',*,*,#11337,.F.);
#14667=ORIENTED_EDGE('',*,*,#11338,.T.);
#14668=ORIENTED_EDGE('',*,*,#11339,.F.);
#14669=ORIENTED_EDGE('',*,*,#11338,.F.);
#14670=ORIENTED_EDGE('',*,*,#11340,.F.);
#14671=ORIENTED_EDGE('',*,*,#11341,.F.);
#14672=ORIENTED_EDGE('',*,*,#11342,.F.);
#14673=ORIENTED_EDGE('',*,*,#11343,.F.);
#14674=ORIENTED_EDGE('',*,*,#11344,.F.);
#14675=ORIENTED_EDGE('',*,*,#11345,.T.);
#14676=ORIENTED_EDGE('',*,*,#11346,.F.);
#14677=ORIENTED_EDGE('',*,*,#11347,.F.);
#14678=ORIENTED_EDGE('',*,*,#11348,.F.);
#14679=ORIENTED_EDGE('',*,*,#11349,.F.);
#14680=ORIENTED_EDGE('',*,*,#11335,.F.);
#14681=ORIENTED_EDGE('',*,*,#11350,.T.);
#14682=ORIENTED_EDGE('',*,*,#11351,.T.);
#14683=ORIENTED_EDGE('',*,*,#11339,.T.);
#14684=ORIENTED_EDGE('',*,*,#11351,.F.);
#14685=ORIENTED_EDGE('',*,*,#11352,.T.);
#14686=ORIENTED_EDGE('',*,*,#11353,.F.);
#14687=ORIENTED_EDGE('',*,*,#11354,.F.);
#14688=ORIENTED_EDGE('',*,*,#11355,.F.);
#14689=ORIENTED_EDGE('',*,*,#11356,.F.);
#14690=ORIENTED_EDGE('',*,*,#11357,.F.);
#14691=ORIENTED_EDGE('',*,*,#11358,.F.);
#14692=ORIENTED_EDGE('',*,*,#11359,.F.);
#14693=ORIENTED_EDGE('',*,*,#11360,.F.);
#14694=ORIENTED_EDGE('',*,*,#11361,.F.);
#14695=ORIENTED_EDGE('',*,*,#11350,.F.);
#14696=ORIENTED_EDGE('',*,*,#11341,.T.);
#14697=ORIENTED_EDGE('',*,*,#11362,.T.);
#14698=ORIENTED_EDGE('',*,*,#11363,.T.);
#14699=ORIENTED_EDGE('',*,*,#11362,.F.);
#14700=ORIENTED_EDGE('',*,*,#11363,.F.);
#14701=ORIENTED_EDGE('',*,*,#11364,.T.);
#14702=ORIENTED_EDGE('',*,*,#11365,.F.);
#14703=ORIENTED_EDGE('',*,*,#11364,.F.);
#14704=ORIENTED_EDGE('',*,*,#11353,.T.);
#14705=ORIENTED_EDGE('',*,*,#11366,.T.);
#14706=ORIENTED_EDGE('',*,*,#11365,.T.);
#14707=ORIENTED_EDGE('',*,*,#11366,.F.);
#14708=ORIENTED_EDGE('',*,*,#11349,.T.);
#14709=ORIENTED_EDGE('',*,*,#11367,.T.);
#14710=ORIENTED_EDGE('',*,*,#11368,.T.);
#14711=ORIENTED_EDGE('',*,*,#11367,.F.);
#14712=ORIENTED_EDGE('',*,*,#11368,.F.);
#14713=ORIENTED_EDGE('',*,*,#11369,.T.);
#14714=ORIENTED_EDGE('',*,*,#11370,.F.);
#14715=ORIENTED_EDGE('',*,*,#11369,.F.);
#14716=ORIENTED_EDGE('',*,*,#11361,.T.);
#14717=ORIENTED_EDGE('',*,*,#11371,.T.);
#14718=ORIENTED_EDGE('',*,*,#11370,.T.);
#14719=ORIENTED_EDGE('',*,*,#11371,.F.);
#14720=ORIENTED_EDGE('',*,*,#11342,.T.);
#14721=ORIENTED_EDGE('',*,*,#11372,.T.);
#14722=ORIENTED_EDGE('',*,*,#11373,.T.);
#14723=ORIENTED_EDGE('',*,*,#11372,.F.);
#14724=ORIENTED_EDGE('',*,*,#11373,.F.);
#14725=ORIENTED_EDGE('',*,*,#11374,.T.);
#14726=ORIENTED_EDGE('',*,*,#11375,.F.);
#14727=ORIENTED_EDGE('',*,*,#11374,.F.);
#14728=ORIENTED_EDGE('',*,*,#11354,.T.);
#14729=ORIENTED_EDGE('',*,*,#11376,.T.);
#14730=ORIENTED_EDGE('',*,*,#11375,.T.);
#14731=ORIENTED_EDGE('',*,*,#11376,.F.);
#14732=ORIENTED_EDGE('',*,*,#11348,.T.);
#14733=ORIENTED_EDGE('',*,*,#11377,.T.);
#14734=ORIENTED_EDGE('',*,*,#11378,.T.);
#14735=ORIENTED_EDGE('',*,*,#11377,.F.);
#14736=ORIENTED_EDGE('',*,*,#11378,.F.);
#14737=ORIENTED_EDGE('',*,*,#11379,.T.);
#14738=ORIENTED_EDGE('',*,*,#11380,.F.);
#14739=ORIENTED_EDGE('',*,*,#11379,.F.);
#14740=ORIENTED_EDGE('',*,*,#11360,.T.);
#14741=ORIENTED_EDGE('',*,*,#11381,.T.);
#14742=ORIENTED_EDGE('',*,*,#11380,.T.);
#14743=ORIENTED_EDGE('',*,*,#11381,.F.);
#14744=ORIENTED_EDGE('',*,*,#11343,.T.);
#14745=ORIENTED_EDGE('',*,*,#11382,.T.);
#14746=ORIENTED_EDGE('',*,*,#11383,.T.);
#14747=ORIENTED_EDGE('',*,*,#11382,.F.);
#14748=ORIENTED_EDGE('',*,*,#11383,.F.);
#14749=ORIENTED_EDGE('',*,*,#11384,.T.);
#14750=ORIENTED_EDGE('',*,*,#11385,.F.);
#14751=ORIENTED_EDGE('',*,*,#11384,.F.);
#14752=ORIENTED_EDGE('',*,*,#11355,.T.);
#14753=ORIENTED_EDGE('',*,*,#11386,.T.);
#14754=ORIENTED_EDGE('',*,*,#11385,.T.);
#14755=ORIENTED_EDGE('',*,*,#11386,.F.);
#14756=ORIENTED_EDGE('',*,*,#11347,.T.);
#14757=ORIENTED_EDGE('',*,*,#11387,.T.);
#14758=ORIENTED_EDGE('',*,*,#11388,.T.);
#14759=ORIENTED_EDGE('',*,*,#11387,.F.);
#14760=ORIENTED_EDGE('',*,*,#11388,.F.);
#14761=ORIENTED_EDGE('',*,*,#11389,.T.);
#14762=ORIENTED_EDGE('',*,*,#11390,.F.);
#14763=ORIENTED_EDGE('',*,*,#11389,.F.);
#14764=ORIENTED_EDGE('',*,*,#11359,.T.);
#14765=ORIENTED_EDGE('',*,*,#11391,.T.);
#14766=ORIENTED_EDGE('',*,*,#11390,.T.);
#14767=ORIENTED_EDGE('',*,*,#11391,.F.);
#14768=ORIENTED_EDGE('',*,*,#11344,.T.);
#14769=ORIENTED_EDGE('',*,*,#11392,.T.);
#14770=ORIENTED_EDGE('',*,*,#11393,.T.);
#14771=ORIENTED_EDGE('',*,*,#11392,.F.);
#14772=ORIENTED_EDGE('',*,*,#11393,.F.);
#14773=ORIENTED_EDGE('',*,*,#11394,.T.);
#14774=ORIENTED_EDGE('',*,*,#11395,.F.);
#14775=ORIENTED_EDGE('',*,*,#11394,.F.);
#14776=ORIENTED_EDGE('',*,*,#11356,.T.);
#14777=ORIENTED_EDGE('',*,*,#11396,.T.);
#14778=ORIENTED_EDGE('',*,*,#11395,.T.);
#14779=ORIENTED_EDGE('',*,*,#11396,.F.);
#14780=ORIENTED_EDGE('',*,*,#11346,.T.);
#14781=ORIENTED_EDGE('',*,*,#11397,.T.);
#14782=ORIENTED_EDGE('',*,*,#11398,.T.);
#14783=ORIENTED_EDGE('',*,*,#11397,.F.);
#14784=ORIENTED_EDGE('',*,*,#11398,.F.);
#14785=ORIENTED_EDGE('',*,*,#11399,.T.);
#14786=ORIENTED_EDGE('',*,*,#11400,.F.);
#14787=ORIENTED_EDGE('',*,*,#11399,.F.);
#14788=ORIENTED_EDGE('',*,*,#11358,.T.);
#14789=ORIENTED_EDGE('',*,*,#11401,.T.);
#14790=ORIENTED_EDGE('',*,*,#11400,.T.);
#14791=ORIENTED_EDGE('',*,*,#11401,.F.);
#14792=ORIENTED_EDGE('',*,*,#11357,.T.);
#14793=ORIENTED_EDGE('',*,*,#11402,.T.);
#14794=ORIENTED_EDGE('',*,*,#11345,.F.);
#14795=ORIENTED_EDGE('',*,*,#11402,.F.);
#14796=ORIENTED_EDGE('',*,*,#11403,.F.);
#14797=ORIENTED_EDGE('',*,*,#11404,.T.);
#14798=ORIENTED_EDGE('',*,*,#11340,.T.);
#14799=ORIENTED_EDGE('',*,*,#11404,.F.);
#14800=ORIENTED_EDGE('',*,*,#11405,.F.);
#14801=ORIENTED_EDGE('',*,*,#11406,.T.);
#14802=ORIENTED_EDGE('',*,*,#11403,.T.);
#14803=ORIENTED_EDGE('',*,*,#11406,.F.);
#14804=ORIENTED_EDGE('',*,*,#11352,.F.);
#14805=ORIENTED_EDGE('',*,*,#11407,.T.);
#14806=ORIENTED_EDGE('',*,*,#11405,.T.);
#14807=ORIENTED_EDGE('',*,*,#11407,.F.);
#14808=ORIENTED_EDGE('',*,*,#11408,.F.);
#14809=ORIENTED_EDGE('',*,*,#11409,.T.);
#14810=ORIENTED_EDGE('',*,*,#11410,.T.);
#14811=ORIENTED_EDGE('',*,*,#11409,.F.);
#14812=ORIENTED_EDGE('',*,*,#11411,.F.);
#14813=ORIENTED_EDGE('',*,*,#11408,.T.);
#14814=ORIENTED_EDGE('',*,*,#11412,.F.);
#14815=ORIENTED_EDGE('',*,*,#11413,.T.);
#14816=ORIENTED_EDGE('',*,*,#11411,.T.);
#14817=ORIENTED_EDGE('',*,*,#11413,.F.);
#14818=ORIENTED_EDGE('',*,*,#11414,.F.);
#14819=ORIENTED_EDGE('',*,*,#11415,.T.);
#14820=ORIENTED_EDGE('',*,*,#11412,.T.);
#14821=ORIENTED_EDGE('',*,*,#11415,.F.);
#14822=ORIENTED_EDGE('',*,*,#11414,.T.);
#14823=ORIENTED_EDGE('',*,*,#11416,.F.);
#14824=ORIENTED_EDGE('',*,*,#11416,.T.);
#14825=ORIENTED_EDGE('',*,*,#11417,.T.);
#14826=ORIENTED_EDGE('',*,*,#11418,.F.);
#14827=ORIENTED_EDGE('',*,*,#11417,.F.);
#14828=ORIENTED_EDGE('',*,*,#11418,.T.);
#14829=ORIENTED_EDGE('',*,*,#11419,.T.);
#14830=ORIENTED_EDGE('',*,*,#11420,.F.);
#14831=ORIENTED_EDGE('',*,*,#11419,.F.);
#14832=ORIENTED_EDGE('',*,*,#11420,.T.);
#14833=ORIENTED_EDGE('',*,*,#11421,.T.);
#14834=ORIENTED_EDGE('',*,*,#11422,.F.);
#14835=ORIENTED_EDGE('',*,*,#11421,.F.);
#14836=ORIENTED_EDGE('',*,*,#11423,.F.);
#14837=ORIENTED_EDGE('',*,*,#11422,.T.);
#14838=ORIENTED_EDGE('',*,*,#11410,.F.);
#14839=ORIENTED_EDGE('',*,*,#11424,.T.);
#14840=ORIENTED_EDGE('',*,*,#11423,.T.);
#14841=ORIENTED_EDGE('',*,*,#11424,.F.);
#14842=ORIENTED_EDGE('',*,*,#11425,.F.);
#14843=ORIENTED_EDGE('',*,*,#11426,.F.);
#14844=ORIENTED_EDGE('',*,*,#11427,.T.);
#14845=ORIENTED_EDGE('',*,*,#11428,.F.);
#14846=ORIENTED_EDGE('',*,*,#11429,.F.);
#14847=ORIENTED_EDGE('',*,*,#11430,.F.);
#14848=ORIENTED_EDGE('',*,*,#11431,.F.);
#14849=ORIENTED_EDGE('',*,*,#11432,.F.);
#14850=ORIENTED_EDGE('',*,*,#11433,.F.);
#14851=ORIENTED_EDGE('',*,*,#11434,.F.);
#14852=ORIENTED_EDGE('',*,*,#11435,.F.);
#14853=ORIENTED_EDGE('',*,*,#11436,.F.);
#14854=ORIENTED_EDGE('',*,*,#11437,.F.);
#14855=ORIENTED_EDGE('',*,*,#11438,.F.);
#14856=ORIENTED_EDGE('',*,*,#11439,.F.);
#14857=ORIENTED_EDGE('',*,*,#11440,.F.);
#14858=ORIENTED_EDGE('',*,*,#11441,.F.);
#14859=ORIENTED_EDGE('',*,*,#11442,.F.);
#14860=ORIENTED_EDGE('',*,*,#11443,.F.);
#14861=ORIENTED_EDGE('',*,*,#11427,.F.);
#14862=ORIENTED_EDGE('',*,*,#11444,.F.);
#14863=ORIENTED_EDGE('',*,*,#11441,.T.);
#14864=ORIENTED_EDGE('',*,*,#11442,.T.);
#14865=ORIENTED_EDGE('',*,*,#11444,.T.);
#14866=ORIENTED_EDGE('',*,*,#11426,.T.);
#14867=ORIENTED_EDGE('',*,*,#11445,.F.);
#14868=ORIENTED_EDGE('',*,*,#11446,.F.);
#14869=ORIENTED_EDGE('',*,*,#11434,.T.);
#14870=ORIENTED_EDGE('',*,*,#11445,.T.);
#14871=ORIENTED_EDGE('',*,*,#11425,.T.);
#14872=ORIENTED_EDGE('',*,*,#11447,.F.);
#14873=ORIENTED_EDGE('',*,*,#11429,.T.);
#14874=ORIENTED_EDGE('',*,*,#11448,.T.);
#14875=ORIENTED_EDGE('',*,*,#11449,.F.);
#14876=ORIENTED_EDGE('',*,*,#11450,.T.);
#14877=ORIENTED_EDGE('',*,*,#11446,.T.);
#14878=ORIENTED_EDGE('',*,*,#11451,.T.);
#14879=ORIENTED_EDGE('',*,*,#11452,.T.);
#14880=ORIENTED_EDGE('',*,*,#11453,.T.);
#14881=ORIENTED_EDGE('',*,*,#11451,.F.);
#14882=ORIENTED_EDGE('',*,*,#11454,.F.);
#14883=ORIENTED_EDGE('',*,*,#11455,.T.);
#14884=ORIENTED_EDGE('',*,*,#11452,.F.);
#14885=ORIENTED_EDGE('',*,*,#11453,.F.);
#14886=ORIENTED_EDGE('',*,*,#11455,.F.);
#14887=ORIENTED_EDGE('',*,*,#11439,.T.);
#14888=ORIENTED_EDGE('',*,*,#11456,.T.);
#14889=ORIENTED_EDGE('',*,*,#11449,.T.);
#14890=ORIENTED_EDGE('',*,*,#11457,.T.);
#14891=ORIENTED_EDGE('',*,*,#11440,.T.);
#14892=ORIENTED_EDGE('',*,*,#11457,.F.);
#14893=ORIENTED_EDGE('',*,*,#11448,.F.);
#14894=ORIENTED_EDGE('',*,*,#11428,.T.);
#14895=ORIENTED_EDGE('',*,*,#11443,.T.);
#14896=ORIENTED_EDGE('',*,*,#11458,.F.);
#14897=ORIENTED_EDGE('',*,*,#11438,.T.);
#14898=ORIENTED_EDGE('',*,*,#11459,.T.);
#14899=ORIENTED_EDGE('',*,*,#11430,.T.);
#14900=ORIENTED_EDGE('',*,*,#11450,.F.);
#14901=ORIENTED_EDGE('',*,*,#11456,.F.);
#14902=ORIENTED_EDGE('',*,*,#11460,.T.);
#14903=ORIENTED_EDGE('',*,*,#11458,.T.);
#14904=ORIENTED_EDGE('',*,*,#11460,.F.);
#14905=ORIENTED_EDGE('',*,*,#11454,.T.);
#14906=ORIENTED_EDGE('',*,*,#11435,.T.);
#14907=ORIENTED_EDGE('',*,*,#11447,.T.);
#14908=ORIENTED_EDGE('',*,*,#11433,.T.);
#14909=ORIENTED_EDGE('',*,*,#11461,.F.);
#14910=ORIENTED_EDGE('',*,*,#11436,.T.);
#14911=ORIENTED_EDGE('',*,*,#11461,.T.);
#14912=ORIENTED_EDGE('',*,*,#11432,.T.);
#14913=ORIENTED_EDGE('',*,*,#11462,.F.);
#14914=ORIENTED_EDGE('',*,*,#11437,.T.);
#14915=ORIENTED_EDGE('',*,*,#11462,.T.);
#14916=ORIENTED_EDGE('',*,*,#11431,.T.);
#14917=ORIENTED_EDGE('',*,*,#11459,.F.);
#14918=ORIENTED_EDGE('',*,*,#11463,.F.);
#14919=ORIENTED_EDGE('',*,*,#11464,.F.);
#14920=ORIENTED_EDGE('',*,*,#11464,.T.);
#14921=ORIENTED_EDGE('',*,*,#11465,.T.);
#14922=ORIENTED_EDGE('',*,*,#11466,.T.);
#14923=ORIENTED_EDGE('',*,*,#11467,.F.);
#14924=ORIENTED_EDGE('',*,*,#11468,.F.);
#14925=ORIENTED_EDGE('',*,*,#11469,.F.);
#14926=ORIENTED_EDGE('',*,*,#11468,.T.);
#14927=ORIENTED_EDGE('',*,*,#11470,.F.);
#14928=ORIENTED_EDGE('',*,*,#11463,.T.);
#14929=ORIENTED_EDGE('',*,*,#11466,.F.);
#14930=ORIENTED_EDGE('',*,*,#11471,.F.);
#14931=ORIENTED_EDGE('',*,*,#11469,.T.);
#14932=ORIENTED_EDGE('',*,*,#11470,.T.);
#14933=ORIENTED_EDGE('',*,*,#11467,.T.);
#14934=ORIENTED_EDGE('',*,*,#11471,.T.);
#14935=ORIENTED_EDGE('',*,*,#11465,.F.);
#14936=ORIENTED_EDGE('',*,*,#11472,.T.);
#14937=ORIENTED_EDGE('',*,*,#11473,.T.);
#14938=ORIENTED_EDGE('',*,*,#11474,.T.);
#14939=ORIENTED_EDGE('',*,*,#11475,.T.);
#14940=ORIENTED_EDGE('',*,*,#11476,.T.);
#14941=ORIENTED_EDGE('',*,*,#11477,.T.);
#14942=ORIENTED_EDGE('',*,*,#11472,.F.);
#14943=ORIENTED_EDGE('',*,*,#11478,.T.);
#14944=ORIENTED_EDGE('',*,*,#11479,.T.);
#14945=ORIENTED_EDGE('',*,*,#11480,.T.);
#14946=ORIENTED_EDGE('',*,*,#11476,.F.);
#14947=ORIENTED_EDGE('',*,*,#11481,.T.);
#14948=ORIENTED_EDGE('',*,*,#11474,.F.);
#14949=ORIENTED_EDGE('',*,*,#11482,.T.);
#14950=ORIENTED_EDGE('',*,*,#11479,.F.);
#14951=ORIENTED_EDGE('',*,*,#11483,.T.);
#14952=ORIENTED_EDGE('',*,*,#11478,.F.);
#14953=ORIENTED_EDGE('',*,*,#11484,.F.);
#14954=ORIENTED_EDGE('',*,*,#11485,.T.);
#14955=ORIENTED_EDGE('',*,*,#11486,.T.);
#14956=ORIENTED_EDGE('',*,*,#11475,.F.);
#14957=ORIENTED_EDGE('',*,*,#11487,.F.);
#14958=ORIENTED_EDGE('',*,*,#11488,.F.);
#14959=ORIENTED_EDGE('',*,*,#11484,.T.);
#14960=ORIENTED_EDGE('',*,*,#11473,.F.);
#14961=ORIENTED_EDGE('',*,*,#11477,.F.);
#14962=ORIENTED_EDGE('',*,*,#11480,.F.);
#14963=ORIENTED_EDGE('',*,*,#11482,.F.);
#14964=ORIENTED_EDGE('',*,*,#11483,.F.);
#14965=ORIENTED_EDGE('',*,*,#11489,.F.);
#14966=ORIENTED_EDGE('',*,*,#11490,.T.);
#14967=ORIENTED_EDGE('',*,*,#11487,.T.);
#14968=ORIENTED_EDGE('',*,*,#11481,.F.);
#14969=ORIENTED_EDGE('',*,*,#11486,.F.);
#14970=ORIENTED_EDGE('',*,*,#11491,.F.);
#14971=ORIENTED_EDGE('',*,*,#11489,.T.);
#14972=ORIENTED_EDGE('',*,*,#11485,.F.);
#14973=ORIENTED_EDGE('',*,*,#11488,.T.);
#14974=ORIENTED_EDGE('',*,*,#11490,.F.);
#14975=ORIENTED_EDGE('',*,*,#11491,.T.);
#14976=ORIENTED_EDGE('',*,*,#11492,.F.);
#14977=ORIENTED_EDGE('',*,*,#11493,.T.);
#14978=ORIENTED_EDGE('',*,*,#11494,.F.);
#14979=ORIENTED_EDGE('',*,*,#11493,.F.);
#14980=ORIENTED_EDGE('',*,*,#11495,.T.);
#14981=ORIENTED_EDGE('',*,*,#11496,.T.);
#14982=ORIENTED_EDGE('',*,*,#11497,.F.);
#14983=ORIENTED_EDGE('',*,*,#11496,.F.);
#14984=ORIENTED_EDGE('',*,*,#11492,.T.);
#14985=ORIENTED_EDGE('',*,*,#11495,.F.);
#14986=ORIENTED_EDGE('',*,*,#11497,.T.);
#14987=ORIENTED_EDGE('',*,*,#11498,.F.);
#14988=ORIENTED_EDGE('',*,*,#11499,.T.);
#14989=ORIENTED_EDGE('',*,*,#11500,.T.);
#14990=ORIENTED_EDGE('',*,*,#11501,.T.);
#14991=ORIENTED_EDGE('',*,*,#11502,.T.);
#14992=ORIENTED_EDGE('',*,*,#11500,.F.);
#14993=ORIENTED_EDGE('',*,*,#11501,.F.);
#14994=ORIENTED_EDGE('',*,*,#11502,.F.);
#14995=ORIENTED_EDGE('',*,*,#11503,.T.);
#14996=ORIENTED_EDGE('',*,*,#11504,.F.);
#14997=ORIENTED_EDGE('',*,*,#11505,.F.);
#14998=ORIENTED_EDGE('',*,*,#11503,.F.);
#14999=ORIENTED_EDGE('',*,*,#11499,.F.);
#15000=ORIENTED_EDGE('',*,*,#11494,.T.);
#15001=ORIENTED_EDGE('',*,*,#11504,.T.);
#15002=ORIENTED_EDGE('',*,*,#11505,.T.);
#15003=ORIENTED_EDGE('',*,*,#11506,.T.);
#15004=ORIENTED_EDGE('',*,*,#11507,.T.);
#15005=ORIENTED_EDGE('',*,*,#11506,.F.);
#15006=ORIENTED_EDGE('',*,*,#11507,.F.);
#15007=ORIENTED_EDGE('',*,*,#11508,.T.);
#15008=ORIENTED_EDGE('',*,*,#11509,.T.);
#15009=ORIENTED_EDGE('',*,*,#11510,.T.);
#15010=ORIENTED_EDGE('',*,*,#11508,.F.);
#15011=ORIENTED_EDGE('',*,*,#11510,.F.);
#15012=ORIENTED_EDGE('',*,*,#11498,.T.);
#15013=ORIENTED_EDGE('',*,*,#11511,.T.);
#15014=ORIENTED_EDGE('',*,*,#11512,.F.);
#15015=ORIENTED_EDGE('',*,*,#11511,.F.);
#15016=ORIENTED_EDGE('',*,*,#11512,.T.);
#15017=ORIENTED_EDGE('',*,*,#11513,.T.);
#15018=ORIENTED_EDGE('',*,*,#11514,.F.);
#15019=ORIENTED_EDGE('',*,*,#11513,.F.);
#15020=ORIENTED_EDGE('',*,*,#11514,.T.);
#15021=ORIENTED_EDGE('',*,*,#11515,.T.);
#15022=ORIENTED_EDGE('',*,*,#11516,.F.);
#15023=ORIENTED_EDGE('',*,*,#11515,.F.);
#15024=ORIENTED_EDGE('',*,*,#11516,.T.);
#15025=ORIENTED_EDGE('',*,*,#11517,.T.);
#15026=ORIENTED_EDGE('',*,*,#11518,.F.);
#15027=ORIENTED_EDGE('',*,*,#11517,.F.);
#15028=ORIENTED_EDGE('',*,*,#11518,.T.);
#15029=ORIENTED_EDGE('',*,*,#11519,.T.);
#15030=ORIENTED_EDGE('',*,*,#11520,.F.);
#15031=ORIENTED_EDGE('',*,*,#11519,.F.);
#15032=ORIENTED_EDGE('',*,*,#11520,.T.);
#15033=ORIENTED_EDGE('',*,*,#11521,.T.);
#15034=ORIENTED_EDGE('',*,*,#11522,.F.);
#15035=ORIENTED_EDGE('',*,*,#11521,.F.);
#15036=ORIENTED_EDGE('',*,*,#11509,.F.);
#15037=ORIENTED_EDGE('',*,*,#11522,.T.);
#15038=ORIENTED_EDGE('',*,*,#11523,.F.);
#15039=ORIENTED_EDGE('',*,*,#11524,.T.);
#15040=ORIENTED_EDGE('',*,*,#11525,.F.);
#15041=ORIENTED_EDGE('',*,*,#11526,.F.);
#15042=ORIENTED_EDGE('',*,*,#11527,.F.);
#15043=ORIENTED_EDGE('',*,*,#11528,.T.);
#15044=ORIENTED_EDGE('',*,*,#11523,.T.);
#15045=ORIENTED_EDGE('',*,*,#11529,.F.);
#15046=ORIENTED_EDGE('',*,*,#11530,.F.);
#15047=ORIENTED_EDGE('',*,*,#11531,.T.);
#15048=ORIENTED_EDGE('',*,*,#11527,.T.);
#15049=ORIENTED_EDGE('',*,*,#11532,.F.);
#15050=ORIENTED_EDGE('',*,*,#11533,.F.);
#15051=ORIENTED_EDGE('',*,*,#11534,.T.);
#15052=ORIENTED_EDGE('',*,*,#11530,.T.);
#15053=ORIENTED_EDGE('',*,*,#11535,.F.);
#15054=ORIENTED_EDGE('',*,*,#11536,.F.);
#15055=ORIENTED_EDGE('',*,*,#11537,.T.);
#15056=ORIENTED_EDGE('',*,*,#11533,.T.);
#15057=ORIENTED_EDGE('',*,*,#11538,.F.);
#15058=ORIENTED_EDGE('',*,*,#11539,.F.);
#15059=ORIENTED_EDGE('',*,*,#11540,.T.);
#15060=ORIENTED_EDGE('',*,*,#11536,.T.);
#15061=ORIENTED_EDGE('',*,*,#11541,.F.);
#15062=ORIENTED_EDGE('',*,*,#11542,.F.);
#15063=ORIENTED_EDGE('',*,*,#11543,.T.);
#15064=ORIENTED_EDGE('',*,*,#11539,.T.);
#15065=ORIENTED_EDGE('',*,*,#11544,.F.);
#15066=ORIENTED_EDGE('',*,*,#11545,.F.);
#15067=ORIENTED_EDGE('',*,*,#11546,.F.);
#15068=ORIENTED_EDGE('',*,*,#11547,.T.);
#15069=ORIENTED_EDGE('',*,*,#11542,.T.);
#15070=ORIENTED_EDGE('',*,*,#11548,.F.);
#15071=ORIENTED_EDGE('',*,*,#11549,.F.);
#15072=ORIENTED_EDGE('',*,*,#11550,.F.);
#15073=ORIENTED_EDGE('',*,*,#11551,.F.);
#15074=ORIENTED_EDGE('',*,*,#11552,.T.);
#15075=ORIENTED_EDGE('',*,*,#11553,.F.);
#15076=ORIENTED_EDGE('',*,*,#11552,.F.);
#15077=ORIENTED_EDGE('',*,*,#11554,.F.);
#15078=ORIENTED_EDGE('',*,*,#11555,.T.);
#15079=ORIENTED_EDGE('',*,*,#11556,.F.);
#15080=ORIENTED_EDGE('',*,*,#11555,.F.);
#15081=ORIENTED_EDGE('',*,*,#11557,.F.);
#15082=ORIENTED_EDGE('',*,*,#11558,.T.);
#15083=ORIENTED_EDGE('',*,*,#11548,.T.);
#15084=ORIENTED_EDGE('',*,*,#11544,.T.);
#15085=ORIENTED_EDGE('',*,*,#11541,.T.);
#15086=ORIENTED_EDGE('',*,*,#11538,.T.);
#15087=ORIENTED_EDGE('',*,*,#11535,.T.);
#15088=ORIENTED_EDGE('',*,*,#11532,.T.);
#15089=ORIENTED_EDGE('',*,*,#11529,.T.);
#15090=ORIENTED_EDGE('',*,*,#11526,.T.);
#15091=ORIENTED_EDGE('',*,*,#11559,.T.);
#15092=ORIENTED_EDGE('',*,*,#11560,.T.);
#15093=ORIENTED_EDGE('',*,*,#11561,.T.);
#15094=ORIENTED_EDGE('',*,*,#11562,.T.);
#15095=ORIENTED_EDGE('',*,*,#11563,.T.);
#15096=ORIENTED_EDGE('',*,*,#11546,.T.);
#15097=ORIENTED_EDGE('',*,*,#11564,.T.);
#15098=ORIENTED_EDGE('',*,*,#11557,.T.);
#15099=ORIENTED_EDGE('',*,*,#11554,.T.);
#15100=ORIENTED_EDGE('',*,*,#11551,.T.);
#15101=ORIENTED_EDGE('',*,*,#11545,.T.);
#15102=ORIENTED_EDGE('',*,*,#11558,.F.);
#15103=ORIENTED_EDGE('',*,*,#11564,.F.);
#15104=ORIENTED_EDGE('',*,*,#11565,.F.);
#15105=ORIENTED_EDGE('',*,*,#11524,.F.);
#15106=ORIENTED_EDGE('',*,*,#11528,.F.);
#15107=ORIENTED_EDGE('',*,*,#11531,.F.);
#15108=ORIENTED_EDGE('',*,*,#11534,.F.);
#15109=ORIENTED_EDGE('',*,*,#11537,.F.);
#15110=ORIENTED_EDGE('',*,*,#11540,.F.);
#15111=ORIENTED_EDGE('',*,*,#11543,.F.);
#15112=ORIENTED_EDGE('',*,*,#11547,.F.);
#15113=ORIENTED_EDGE('',*,*,#11563,.F.);
#15114=ORIENTED_EDGE('',*,*,#11566,.T.);
#15115=ORIENTED_EDGE('',*,*,#11567,.F.);
#15116=ORIENTED_EDGE('',*,*,#11566,.F.);
#15117=ORIENTED_EDGE('',*,*,#11562,.F.);
#15118=ORIENTED_EDGE('',*,*,#11568,.T.);
#15119=ORIENTED_EDGE('',*,*,#11569,.F.);
#15120=ORIENTED_EDGE('',*,*,#11568,.F.);
#15121=ORIENTED_EDGE('',*,*,#11561,.F.);
#15122=ORIENTED_EDGE('',*,*,#11550,.T.);
#15123=ORIENTED_EDGE('',*,*,#11570,.F.);
#15124=ORIENTED_EDGE('',*,*,#11571,.T.);
#15125=ORIENTED_EDGE('',*,*,#11572,.T.);
#15126=ORIENTED_EDGE('',*,*,#11573,.F.);
#15127=ORIENTED_EDGE('',*,*,#11574,.F.);
#15128=ORIENTED_EDGE('',*,*,#11575,.T.);
#15129=ORIENTED_EDGE('',*,*,#11576,.T.);
#15130=ORIENTED_EDGE('',*,*,#11571,.F.);
#15131=ORIENTED_EDGE('',*,*,#11577,.F.);
#15132=ORIENTED_EDGE('',*,*,#11578,.T.);
#15133=ORIENTED_EDGE('',*,*,#11579,.T.);
#15134=ORIENTED_EDGE('',*,*,#11575,.F.);
#15135=ORIENTED_EDGE('',*,*,#11580,.F.);
#15136=ORIENTED_EDGE('',*,*,#11581,.T.);
#15137=ORIENTED_EDGE('',*,*,#11582,.T.);
#15138=ORIENTED_EDGE('',*,*,#11578,.F.);
#15139=ORIENTED_EDGE('',*,*,#11583,.F.);
#15140=ORIENTED_EDGE('',*,*,#11584,.T.);
#15141=ORIENTED_EDGE('',*,*,#11585,.T.);
#15142=ORIENTED_EDGE('',*,*,#11581,.F.);
#15143=ORIENTED_EDGE('',*,*,#11586,.F.);
#15144=ORIENTED_EDGE('',*,*,#11573,.T.);
#15145=ORIENTED_EDGE('',*,*,#11587,.T.);
#15146=ORIENTED_EDGE('',*,*,#11584,.F.);
#15147=ORIENTED_EDGE('',*,*,#11587,.F.);
#15148=ORIENTED_EDGE('',*,*,#11572,.F.);
#15149=ORIENTED_EDGE('',*,*,#11576,.F.);
#15150=ORIENTED_EDGE('',*,*,#11579,.F.);
#15151=ORIENTED_EDGE('',*,*,#11582,.F.);
#15152=ORIENTED_EDGE('',*,*,#11585,.F.);
#15153=ORIENTED_EDGE('',*,*,#11588,.F.);
#15154=ORIENTED_EDGE('',*,*,#11589,.T.);
#15155=ORIENTED_EDGE('',*,*,#11590,.F.);
#15156=ORIENTED_EDGE('',*,*,#11591,.F.);
#15157=ORIENTED_EDGE('',*,*,#11592,.F.);
#15158=ORIENTED_EDGE('',*,*,#11591,.T.);
#15159=ORIENTED_EDGE('',*,*,#11593,.T.);
#15160=ORIENTED_EDGE('',*,*,#11594,.F.);
#15161=ORIENTED_EDGE('',*,*,#11593,.F.);
#15162=ORIENTED_EDGE('',*,*,#11590,.T.);
#15163=ORIENTED_EDGE('',*,*,#11595,.T.);
#15164=ORIENTED_EDGE('',*,*,#11596,.F.);
#15165=ORIENTED_EDGE('',*,*,#11595,.F.);
#15166=ORIENTED_EDGE('',*,*,#11589,.F.);
#15167=ORIENTED_EDGE('',*,*,#11597,.F.);
#15168=ORIENTED_EDGE('',*,*,#11598,.T.);
#15169=ORIENTED_EDGE('',*,*,#11599,.F.);
#15170=ORIENTED_EDGE('',*,*,#11600,.F.);
#15171=ORIENTED_EDGE('',*,*,#11601,.F.);
#15172=ORIENTED_EDGE('',*,*,#11600,.T.);
#15173=ORIENTED_EDGE('',*,*,#11602,.T.);
#15174=ORIENTED_EDGE('',*,*,#11603,.F.);
#15175=ORIENTED_EDGE('',*,*,#11602,.F.);
#15176=ORIENTED_EDGE('',*,*,#11599,.T.);
#15177=ORIENTED_EDGE('',*,*,#11604,.T.);
#15178=ORIENTED_EDGE('',*,*,#11605,.F.);
#15179=ORIENTED_EDGE('',*,*,#11604,.F.);
#15180=ORIENTED_EDGE('',*,*,#11598,.F.);
#15181=ORIENTED_EDGE('',*,*,#11606,.F.);
#15182=ORIENTED_EDGE('',*,*,#11607,.T.);
#15183=ORIENTED_EDGE('',*,*,#11608,.F.);
#15184=ORIENTED_EDGE('',*,*,#11609,.F.);
#15185=ORIENTED_EDGE('',*,*,#11610,.F.);
#15186=ORIENTED_EDGE('',*,*,#11609,.T.);
#15187=ORIENTED_EDGE('',*,*,#11611,.T.);
#15188=ORIENTED_EDGE('',*,*,#11612,.F.);
#15189=ORIENTED_EDGE('',*,*,#11611,.F.);
#15190=ORIENTED_EDGE('',*,*,#11608,.T.);
#15191=ORIENTED_EDGE('',*,*,#11613,.T.);
#15192=ORIENTED_EDGE('',*,*,#11614,.F.);
#15193=ORIENTED_EDGE('',*,*,#11613,.F.);
#15194=ORIENTED_EDGE('',*,*,#11607,.F.);
#15195=ORIENTED_EDGE('',*,*,#11615,.F.);
#15196=ORIENTED_EDGE('',*,*,#11616,.T.);
#15197=ORIENTED_EDGE('',*,*,#11617,.F.);
#15198=ORIENTED_EDGE('',*,*,#11618,.F.);
#15199=ORIENTED_EDGE('',*,*,#11619,.F.);
#15200=ORIENTED_EDGE('',*,*,#11618,.T.);
#15201=ORIENTED_EDGE('',*,*,#11620,.T.);
#15202=ORIENTED_EDGE('',*,*,#11621,.F.);
#15203=ORIENTED_EDGE('',*,*,#11620,.F.);
#15204=ORIENTED_EDGE('',*,*,#11617,.T.);
#15205=ORIENTED_EDGE('',*,*,#11622,.T.);
#15206=ORIENTED_EDGE('',*,*,#11623,.F.);
#15207=ORIENTED_EDGE('',*,*,#11622,.F.);
#15208=ORIENTED_EDGE('',*,*,#11616,.F.);
#15209=ORIENTED_EDGE('',*,*,#11624,.F.);
#15210=ORIENTED_EDGE('',*,*,#11625,.T.);
#15211=ORIENTED_EDGE('',*,*,#11626,.F.);
#15212=ORIENTED_EDGE('',*,*,#11627,.F.);
#15213=ORIENTED_EDGE('',*,*,#11628,.F.);
#15214=ORIENTED_EDGE('',*,*,#11627,.T.);
#15215=ORIENTED_EDGE('',*,*,#11629,.T.);
#15216=ORIENTED_EDGE('',*,*,#11630,.F.);
#15217=ORIENTED_EDGE('',*,*,#11629,.F.);
#15218=ORIENTED_EDGE('',*,*,#11626,.T.);
#15219=ORIENTED_EDGE('',*,*,#11631,.T.);
#15220=ORIENTED_EDGE('',*,*,#11632,.F.);
#15221=ORIENTED_EDGE('',*,*,#11631,.F.);
#15222=ORIENTED_EDGE('',*,*,#11625,.F.);
#15223=ORIENTED_EDGE('',*,*,#11633,.F.);
#15224=ORIENTED_EDGE('',*,*,#11634,.T.);
#15225=ORIENTED_EDGE('',*,*,#11635,.F.);
#15226=ORIENTED_EDGE('',*,*,#11636,.F.);
#15227=ORIENTED_EDGE('',*,*,#11637,.F.);
#15228=ORIENTED_EDGE('',*,*,#11636,.T.);
#15229=ORIENTED_EDGE('',*,*,#11638,.T.);
#15230=ORIENTED_EDGE('',*,*,#11639,.F.);
#15231=ORIENTED_EDGE('',*,*,#11638,.F.);
#15232=ORIENTED_EDGE('',*,*,#11635,.T.);
#15233=ORIENTED_EDGE('',*,*,#11640,.T.);
#15234=ORIENTED_EDGE('',*,*,#11641,.F.);
#15235=ORIENTED_EDGE('',*,*,#11640,.F.);
#15236=ORIENTED_EDGE('',*,*,#11634,.F.);
#15237=ORIENTED_EDGE('',*,*,#11642,.F.);
#15238=ORIENTED_EDGE('',*,*,#11643,.T.);
#15239=ORIENTED_EDGE('',*,*,#11644,.F.);
#15240=ORIENTED_EDGE('',*,*,#11645,.F.);
#15241=ORIENTED_EDGE('',*,*,#11646,.F.);
#15242=ORIENTED_EDGE('',*,*,#11645,.T.);
#15243=ORIENTED_EDGE('',*,*,#11647,.T.);
#15244=ORIENTED_EDGE('',*,*,#11648,.F.);
#15245=ORIENTED_EDGE('',*,*,#11647,.F.);
#15246=ORIENTED_EDGE('',*,*,#11644,.T.);
#15247=ORIENTED_EDGE('',*,*,#11649,.T.);
#15248=ORIENTED_EDGE('',*,*,#11650,.F.);
#15249=ORIENTED_EDGE('',*,*,#11649,.F.);
#15250=ORIENTED_EDGE('',*,*,#11643,.F.);
#15251=ORIENTED_EDGE('',*,*,#11651,.F.);
#15252=ORIENTED_EDGE('',*,*,#11652,.T.);
#15253=ORIENTED_EDGE('',*,*,#11653,.T.);
#15254=ORIENTED_EDGE('',*,*,#11654,.F.);
#15255=ORIENTED_EDGE('',*,*,#11655,.T.);
#15256=ORIENTED_EDGE('',*,*,#11656,.F.);
#15257=ORIENTED_EDGE('',*,*,#11652,.F.);
#15258=ORIENTED_EDGE('',*,*,#11657,.F.);
#15259=ORIENTED_EDGE('',*,*,#11653,.F.);
#15260=ORIENTED_EDGE('',*,*,#11656,.T.);
#15261=ORIENTED_EDGE('',*,*,#11658,.T.);
#15262=ORIENTED_EDGE('',*,*,#11659,.F.);
#15263=ORIENTED_EDGE('',*,*,#11658,.F.);
#15264=ORIENTED_EDGE('',*,*,#11655,.F.);
#15265=ORIENTED_EDGE('',*,*,#11660,.F.);
#15266=ORIENTED_EDGE('',*,*,#11661,.T.);
#15267=ORIENTED_EDGE('',*,*,#11662,.F.);
#15268=ORIENTED_EDGE('',*,*,#11663,.F.);
#15269=ORIENTED_EDGE('',*,*,#11664,.F.);
#15270=ORIENTED_EDGE('',*,*,#11663,.T.);
#15271=ORIENTED_EDGE('',*,*,#11665,.T.);
#15272=ORIENTED_EDGE('',*,*,#11666,.F.);
#15273=ORIENTED_EDGE('',*,*,#11665,.F.);
#15274=ORIENTED_EDGE('',*,*,#11662,.T.);
#15275=ORIENTED_EDGE('',*,*,#11667,.T.);
#15276=ORIENTED_EDGE('',*,*,#11668,.F.);
#15277=ORIENTED_EDGE('',*,*,#11667,.F.);
#15278=ORIENTED_EDGE('',*,*,#11661,.F.);
#15279=ORIENTED_EDGE('',*,*,#11669,.F.);
#15280=ORIENTED_EDGE('',*,*,#11670,.T.);
#15281=ORIENTED_EDGE('',*,*,#11671,.F.);
#15282=ORIENTED_EDGE('',*,*,#11672,.F.);
#15283=ORIENTED_EDGE('',*,*,#11673,.F.);
#15284=ORIENTED_EDGE('',*,*,#11672,.T.);
#15285=ORIENTED_EDGE('',*,*,#11674,.T.);
#15286=ORIENTED_EDGE('',*,*,#11675,.F.);
#15287=ORIENTED_EDGE('',*,*,#11674,.F.);
#15288=ORIENTED_EDGE('',*,*,#11671,.T.);
#15289=ORIENTED_EDGE('',*,*,#11676,.T.);
#15290=ORIENTED_EDGE('',*,*,#11677,.F.);
#15291=ORIENTED_EDGE('',*,*,#11676,.F.);
#15292=ORIENTED_EDGE('',*,*,#11670,.F.);
#15293=ORIENTED_EDGE('',*,*,#11678,.F.);
#15294=ORIENTED_EDGE('',*,*,#11679,.T.);
#15295=ORIENTED_EDGE('',*,*,#11680,.F.);
#15296=ORIENTED_EDGE('',*,*,#11681,.F.);
#15297=ORIENTED_EDGE('',*,*,#11682,.F.);
#15298=ORIENTED_EDGE('',*,*,#11681,.T.);
#15299=ORIENTED_EDGE('',*,*,#11683,.T.);
#15300=ORIENTED_EDGE('',*,*,#11684,.F.);
#15301=ORIENTED_EDGE('',*,*,#11683,.F.);
#15302=ORIENTED_EDGE('',*,*,#11680,.T.);
#15303=ORIENTED_EDGE('',*,*,#11685,.T.);
#15304=ORIENTED_EDGE('',*,*,#11686,.F.);
#15305=ORIENTED_EDGE('',*,*,#11685,.F.);
#15306=ORIENTED_EDGE('',*,*,#11679,.F.);
#15307=ORIENTED_EDGE('',*,*,#11687,.F.);
#15308=ORIENTED_EDGE('',*,*,#11688,.T.);
#15309=ORIENTED_EDGE('',*,*,#11689,.F.);
#15310=ORIENTED_EDGE('',*,*,#11690,.F.);
#15311=ORIENTED_EDGE('',*,*,#11691,.F.);
#15312=ORIENTED_EDGE('',*,*,#11690,.T.);
#15313=ORIENTED_EDGE('',*,*,#11692,.T.);
#15314=ORIENTED_EDGE('',*,*,#11693,.F.);
#15315=ORIENTED_EDGE('',*,*,#11692,.F.);
#15316=ORIENTED_EDGE('',*,*,#11689,.T.);
#15317=ORIENTED_EDGE('',*,*,#11694,.T.);
#15318=ORIENTED_EDGE('',*,*,#11695,.F.);
#15319=ORIENTED_EDGE('',*,*,#11694,.F.);
#15320=ORIENTED_EDGE('',*,*,#11688,.F.);
#15321=ORIENTED_EDGE('',*,*,#11696,.F.);
#15322=ORIENTED_EDGE('',*,*,#11697,.T.);
#15323=ORIENTED_EDGE('',*,*,#11698,.F.);
#15324=ORIENTED_EDGE('',*,*,#11699,.F.);
#15325=ORIENTED_EDGE('',*,*,#11700,.F.);
#15326=ORIENTED_EDGE('',*,*,#11699,.T.);
#15327=ORIENTED_EDGE('',*,*,#11701,.T.);
#15328=ORIENTED_EDGE('',*,*,#11702,.F.);
#15329=ORIENTED_EDGE('',*,*,#11701,.F.);
#15330=ORIENTED_EDGE('',*,*,#11698,.T.);
#15331=ORIENTED_EDGE('',*,*,#11703,.T.);
#15332=ORIENTED_EDGE('',*,*,#11704,.F.);
#15333=ORIENTED_EDGE('',*,*,#11703,.F.);
#15334=ORIENTED_EDGE('',*,*,#11697,.F.);
#15335=ORIENTED_EDGE('',*,*,#11705,.F.);
#15336=ORIENTED_EDGE('',*,*,#11706,.T.);
#15337=ORIENTED_EDGE('',*,*,#11707,.F.);
#15338=ORIENTED_EDGE('',*,*,#11708,.F.);
#15339=ORIENTED_EDGE('',*,*,#11709,.F.);
#15340=ORIENTED_EDGE('',*,*,#11708,.T.);
#15341=ORIENTED_EDGE('',*,*,#11710,.T.);
#15342=ORIENTED_EDGE('',*,*,#11711,.F.);
#15343=ORIENTED_EDGE('',*,*,#11710,.F.);
#15344=ORIENTED_EDGE('',*,*,#11707,.T.);
#15345=ORIENTED_EDGE('',*,*,#11712,.T.);
#15346=ORIENTED_EDGE('',*,*,#11713,.F.);
#15347=ORIENTED_EDGE('',*,*,#11712,.F.);
#15348=ORIENTED_EDGE('',*,*,#11706,.F.);
#15349=ORIENTED_EDGE('',*,*,#11714,.F.);
#15350=ORIENTED_EDGE('',*,*,#11715,.T.);
#15351=ORIENTED_EDGE('',*,*,#11716,.F.);
#15352=ORIENTED_EDGE('',*,*,#11717,.F.);
#15353=ORIENTED_EDGE('',*,*,#11718,.F.);
#15354=ORIENTED_EDGE('',*,*,#11717,.T.);
#15355=ORIENTED_EDGE('',*,*,#11719,.T.);
#15356=ORIENTED_EDGE('',*,*,#11720,.F.);
#15357=ORIENTED_EDGE('',*,*,#11719,.F.);
#15358=ORIENTED_EDGE('',*,*,#11716,.T.);
#15359=ORIENTED_EDGE('',*,*,#11721,.T.);
#15360=ORIENTED_EDGE('',*,*,#11722,.F.);
#15361=ORIENTED_EDGE('',*,*,#11721,.F.);
#15362=ORIENTED_EDGE('',*,*,#11715,.F.);
#15363=ORIENTED_EDGE('',*,*,#11723,.F.);
#15364=ORIENTED_EDGE('',*,*,#11724,.T.);
#15365=ORIENTED_EDGE('',*,*,#11725,.F.);
#15366=ORIENTED_EDGE('',*,*,#11726,.F.);
#15367=ORIENTED_EDGE('',*,*,#11727,.F.);
#15368=ORIENTED_EDGE('',*,*,#11726,.T.);
#15369=ORIENTED_EDGE('',*,*,#11728,.T.);
#15370=ORIENTED_EDGE('',*,*,#11729,.F.);
#15371=ORIENTED_EDGE('',*,*,#11728,.F.);
#15372=ORIENTED_EDGE('',*,*,#11725,.T.);
#15373=ORIENTED_EDGE('',*,*,#11730,.T.);
#15374=ORIENTED_EDGE('',*,*,#11731,.F.);
#15375=ORIENTED_EDGE('',*,*,#11730,.F.);
#15376=ORIENTED_EDGE('',*,*,#11724,.F.);
#15377=ORIENTED_EDGE('',*,*,#11732,.F.);
#15378=ORIENTED_EDGE('',*,*,#11733,.T.);
#15379=ORIENTED_EDGE('',*,*,#11734,.F.);
#15380=ORIENTED_EDGE('',*,*,#11735,.F.);
#15381=ORIENTED_EDGE('',*,*,#11736,.F.);
#15382=ORIENTED_EDGE('',*,*,#11735,.T.);
#15383=ORIENTED_EDGE('',*,*,#11737,.T.);
#15384=ORIENTED_EDGE('',*,*,#11738,.F.);
#15385=ORIENTED_EDGE('',*,*,#11737,.F.);
#15386=ORIENTED_EDGE('',*,*,#11734,.T.);
#15387=ORIENTED_EDGE('',*,*,#11739,.T.);
#15388=ORIENTED_EDGE('',*,*,#11740,.F.);
#15389=ORIENTED_EDGE('',*,*,#11739,.F.);
#15390=ORIENTED_EDGE('',*,*,#11733,.F.);
#15391=ORIENTED_EDGE('',*,*,#11741,.F.);
#15392=ORIENTED_EDGE('',*,*,#11742,.T.);
#15393=ORIENTED_EDGE('',*,*,#11743,.F.);
#15394=ORIENTED_EDGE('',*,*,#11744,.F.);
#15395=ORIENTED_EDGE('',*,*,#11745,.F.);
#15396=ORIENTED_EDGE('',*,*,#11744,.T.);
#15397=ORIENTED_EDGE('',*,*,#11746,.T.);
#15398=ORIENTED_EDGE('',*,*,#11747,.F.);
#15399=ORIENTED_EDGE('',*,*,#11746,.F.);
#15400=ORIENTED_EDGE('',*,*,#11743,.T.);
#15401=ORIENTED_EDGE('',*,*,#11748,.T.);
#15402=ORIENTED_EDGE('',*,*,#11749,.F.);
#15403=ORIENTED_EDGE('',*,*,#11748,.F.);
#15404=ORIENTED_EDGE('',*,*,#11742,.F.);
#15405=ORIENTED_EDGE('',*,*,#11750,.F.);
#15406=ORIENTED_EDGE('',*,*,#11751,.T.);
#15407=ORIENTED_EDGE('',*,*,#11752,.F.);
#15408=ORIENTED_EDGE('',*,*,#11753,.F.);
#15409=ORIENTED_EDGE('',*,*,#11754,.F.);
#15410=ORIENTED_EDGE('',*,*,#11753,.T.);
#15411=ORIENTED_EDGE('',*,*,#11755,.T.);
#15412=ORIENTED_EDGE('',*,*,#11756,.F.);
#15413=ORIENTED_EDGE('',*,*,#11755,.F.);
#15414=ORIENTED_EDGE('',*,*,#11752,.T.);
#15415=ORIENTED_EDGE('',*,*,#11757,.T.);
#15416=ORIENTED_EDGE('',*,*,#11758,.F.);
#15417=ORIENTED_EDGE('',*,*,#11757,.F.);
#15418=ORIENTED_EDGE('',*,*,#11751,.F.);
#15419=ORIENTED_EDGE('',*,*,#11759,.F.);
#15420=ORIENTED_EDGE('',*,*,#11760,.T.);
#15421=ORIENTED_EDGE('',*,*,#11761,.F.);
#15422=ORIENTED_EDGE('',*,*,#11762,.F.);
#15423=ORIENTED_EDGE('',*,*,#11763,.F.);
#15424=ORIENTED_EDGE('',*,*,#11762,.T.);
#15425=ORIENTED_EDGE('',*,*,#11764,.T.);
#15426=ORIENTED_EDGE('',*,*,#11765,.F.);
#15427=ORIENTED_EDGE('',*,*,#11764,.F.);
#15428=ORIENTED_EDGE('',*,*,#11761,.T.);
#15429=ORIENTED_EDGE('',*,*,#11766,.T.);
#15430=ORIENTED_EDGE('',*,*,#11767,.F.);
#15431=ORIENTED_EDGE('',*,*,#11766,.F.);
#15432=ORIENTED_EDGE('',*,*,#11760,.F.);
#15433=ORIENTED_EDGE('',*,*,#11768,.F.);
#15434=ORIENTED_EDGE('',*,*,#11769,.T.);
#15435=ORIENTED_EDGE('',*,*,#11770,.F.);
#15436=ORIENTED_EDGE('',*,*,#11771,.F.);
#15437=ORIENTED_EDGE('',*,*,#11772,.F.);
#15438=ORIENTED_EDGE('',*,*,#11771,.T.);
#15439=ORIENTED_EDGE('',*,*,#11773,.T.);
#15440=ORIENTED_EDGE('',*,*,#11774,.F.);
#15441=ORIENTED_EDGE('',*,*,#11773,.F.);
#15442=ORIENTED_EDGE('',*,*,#11770,.T.);
#15443=ORIENTED_EDGE('',*,*,#11775,.T.);
#15444=ORIENTED_EDGE('',*,*,#11776,.F.);
#15445=ORIENTED_EDGE('',*,*,#11775,.F.);
#15446=ORIENTED_EDGE('',*,*,#11769,.F.);
#15447=ORIENTED_EDGE('',*,*,#11777,.F.);
#15448=ORIENTED_EDGE('',*,*,#11778,.T.);
#15449=ORIENTED_EDGE('',*,*,#11779,.F.);
#15450=ORIENTED_EDGE('',*,*,#11780,.F.);
#15451=ORIENTED_EDGE('',*,*,#11781,.F.);
#15452=ORIENTED_EDGE('',*,*,#11780,.T.);
#15453=ORIENTED_EDGE('',*,*,#11782,.T.);
#15454=ORIENTED_EDGE('',*,*,#11783,.F.);
#15455=ORIENTED_EDGE('',*,*,#11782,.F.);
#15456=ORIENTED_EDGE('',*,*,#11779,.T.);
#15457=ORIENTED_EDGE('',*,*,#11784,.T.);
#15458=ORIENTED_EDGE('',*,*,#11785,.F.);
#15459=ORIENTED_EDGE('',*,*,#11784,.F.);
#15460=ORIENTED_EDGE('',*,*,#11778,.F.);
#15461=ORIENTED_EDGE('',*,*,#11786,.F.);
#15462=ORIENTED_EDGE('',*,*,#11787,.T.);
#15463=ORIENTED_EDGE('',*,*,#11788,.F.);
#15464=ORIENTED_EDGE('',*,*,#11789,.F.);
#15465=ORIENTED_EDGE('',*,*,#11790,.F.);
#15466=ORIENTED_EDGE('',*,*,#11789,.T.);
#15467=ORIENTED_EDGE('',*,*,#11791,.T.);
#15468=ORIENTED_EDGE('',*,*,#11792,.F.);
#15469=ORIENTED_EDGE('',*,*,#11793,.F.);
#15470=ORIENTED_EDGE('',*,*,#11791,.F.);
#15471=ORIENTED_EDGE('',*,*,#11788,.T.);
#15472=ORIENTED_EDGE('',*,*,#11794,.T.);
#15473=ORIENTED_EDGE('',*,*,#11795,.F.);
#15474=ORIENTED_EDGE('',*,*,#11794,.F.);
#15475=ORIENTED_EDGE('',*,*,#11787,.F.);
#15476=ORIENTED_EDGE('',*,*,#11796,.F.);
#15477=ORIENTED_EDGE('',*,*,#11797,.F.);
#15478=ORIENTED_EDGE('',*,*,#11798,.T.);
#15479=ORIENTED_EDGE('',*,*,#11799,.F.);
#15480=ORIENTED_EDGE('',*,*,#11800,.F.);
#15481=ORIENTED_EDGE('',*,*,#11801,.F.);
#15482=ORIENTED_EDGE('',*,*,#11800,.T.);
#15483=ORIENTED_EDGE('',*,*,#11802,.T.);
#15484=ORIENTED_EDGE('',*,*,#11803,.F.);
#15485=ORIENTED_EDGE('',*,*,#11802,.F.);
#15486=ORIENTED_EDGE('',*,*,#11799,.T.);
#15487=ORIENTED_EDGE('',*,*,#11804,.T.);
#15488=ORIENTED_EDGE('',*,*,#11805,.F.);
#15489=ORIENTED_EDGE('',*,*,#11804,.F.);
#15490=ORIENTED_EDGE('',*,*,#11798,.F.);
#15491=ORIENTED_EDGE('',*,*,#11806,.F.);
#15492=ORIENTED_EDGE('',*,*,#11807,.T.);
#15493=ORIENTED_EDGE('',*,*,#11808,.F.);
#15494=ORIENTED_EDGE('',*,*,#11809,.F.);
#15495=ORIENTED_EDGE('',*,*,#11810,.F.);
#15496=ORIENTED_EDGE('',*,*,#11809,.T.);
#15497=ORIENTED_EDGE('',*,*,#11811,.T.);
#15498=ORIENTED_EDGE('',*,*,#11812,.F.);
#15499=ORIENTED_EDGE('',*,*,#11811,.F.);
#15500=ORIENTED_EDGE('',*,*,#11808,.T.);
#15501=ORIENTED_EDGE('',*,*,#11813,.T.);
#15502=ORIENTED_EDGE('',*,*,#11814,.F.);
#15503=ORIENTED_EDGE('',*,*,#11813,.F.);
#15504=ORIENTED_EDGE('',*,*,#11807,.F.);
#15505=ORIENTED_EDGE('',*,*,#11815,.F.);
#15506=ORIENTED_EDGE('',*,*,#11816,.T.);
#15507=ORIENTED_EDGE('',*,*,#11817,.F.);
#15508=ORIENTED_EDGE('',*,*,#11818,.F.);
#15509=ORIENTED_EDGE('',*,*,#11819,.F.);
#15510=ORIENTED_EDGE('',*,*,#11818,.T.);
#15511=ORIENTED_EDGE('',*,*,#11820,.T.);
#15512=ORIENTED_EDGE('',*,*,#11821,.F.);
#15513=ORIENTED_EDGE('',*,*,#11820,.F.);
#15514=ORIENTED_EDGE('',*,*,#11817,.T.);
#15515=ORIENTED_EDGE('',*,*,#11822,.T.);
#15516=ORIENTED_EDGE('',*,*,#11823,.F.);
#15517=ORIENTED_EDGE('',*,*,#11822,.F.);
#15518=ORIENTED_EDGE('',*,*,#11816,.F.);
#15519=ORIENTED_EDGE('',*,*,#11824,.F.);
#15520=ORIENTED_EDGE('',*,*,#11825,.T.);
#15521=ORIENTED_EDGE('',*,*,#11826,.F.);
#15522=ORIENTED_EDGE('',*,*,#11827,.F.);
#15523=ORIENTED_EDGE('',*,*,#11828,.F.);
#15524=ORIENTED_EDGE('',*,*,#11827,.T.);
#15525=ORIENTED_EDGE('',*,*,#11829,.T.);
#15526=ORIENTED_EDGE('',*,*,#11830,.F.);
#15527=ORIENTED_EDGE('',*,*,#11829,.F.);
#15528=ORIENTED_EDGE('',*,*,#11826,.T.);
#15529=ORIENTED_EDGE('',*,*,#11831,.T.);
#15530=ORIENTED_EDGE('',*,*,#11832,.F.);
#15531=ORIENTED_EDGE('',*,*,#11831,.F.);
#15532=ORIENTED_EDGE('',*,*,#11825,.F.);
#15533=ORIENTED_EDGE('',*,*,#11833,.F.);
#15534=ORIENTED_EDGE('',*,*,#11834,.T.);
#15535=ORIENTED_EDGE('',*,*,#11835,.F.);
#15536=ORIENTED_EDGE('',*,*,#11836,.F.);
#15537=ORIENTED_EDGE('',*,*,#11837,.F.);
#15538=ORIENTED_EDGE('',*,*,#11836,.T.);
#15539=ORIENTED_EDGE('',*,*,#11838,.T.);
#15540=ORIENTED_EDGE('',*,*,#11839,.F.);
#15541=ORIENTED_EDGE('',*,*,#11838,.F.);
#15542=ORIENTED_EDGE('',*,*,#11835,.T.);
#15543=ORIENTED_EDGE('',*,*,#11840,.T.);
#15544=ORIENTED_EDGE('',*,*,#11841,.F.);
#15545=ORIENTED_EDGE('',*,*,#11840,.F.);
#15546=ORIENTED_EDGE('',*,*,#11834,.F.);
#15547=ORIENTED_EDGE('',*,*,#11842,.F.);
#15548=ORIENTED_EDGE('',*,*,#11843,.T.);
#15549=ORIENTED_EDGE('',*,*,#11844,.F.);
#15550=ORIENTED_EDGE('',*,*,#11845,.F.);
#15551=ORIENTED_EDGE('',*,*,#11846,.F.);
#15552=ORIENTED_EDGE('',*,*,#11845,.T.);
#15553=ORIENTED_EDGE('',*,*,#11847,.T.);
#15554=ORIENTED_EDGE('',*,*,#11848,.F.);
#15555=ORIENTED_EDGE('',*,*,#11847,.F.);
#15556=ORIENTED_EDGE('',*,*,#11844,.T.);
#15557=ORIENTED_EDGE('',*,*,#11849,.T.);
#15558=ORIENTED_EDGE('',*,*,#11850,.F.);
#15559=ORIENTED_EDGE('',*,*,#11849,.F.);
#15560=ORIENTED_EDGE('',*,*,#11843,.F.);
#15561=ORIENTED_EDGE('',*,*,#11851,.F.);
#15562=ORIENTED_EDGE('',*,*,#11852,.T.);
#15563=ORIENTED_EDGE('',*,*,#11853,.F.);
#15564=ORIENTED_EDGE('',*,*,#11854,.F.);
#15565=ORIENTED_EDGE('',*,*,#11855,.F.);
#15566=ORIENTED_EDGE('',*,*,#11854,.T.);
#15567=ORIENTED_EDGE('',*,*,#11856,.T.);
#15568=ORIENTED_EDGE('',*,*,#11857,.F.);
#15569=ORIENTED_EDGE('',*,*,#11856,.F.);
#15570=ORIENTED_EDGE('',*,*,#11853,.T.);
#15571=ORIENTED_EDGE('',*,*,#11858,.T.);
#15572=ORIENTED_EDGE('',*,*,#11859,.F.);
#15573=ORIENTED_EDGE('',*,*,#11858,.F.);
#15574=ORIENTED_EDGE('',*,*,#11852,.F.);
#15575=ORIENTED_EDGE('',*,*,#11860,.F.);
#15576=ORIENTED_EDGE('',*,*,#11861,.T.);
#15577=ORIENTED_EDGE('',*,*,#11862,.F.);
#15578=ORIENTED_EDGE('',*,*,#11863,.F.);
#15579=ORIENTED_EDGE('',*,*,#11864,.F.);
#15580=ORIENTED_EDGE('',*,*,#11865,.F.);
#15581=ORIENTED_EDGE('',*,*,#11866,.F.);
#15582=ORIENTED_EDGE('',*,*,#11867,.F.);
#15583=ORIENTED_EDGE('',*,*,#11868,.F.);
#15584=ORIENTED_EDGE('',*,*,#11861,.F.);
#15585=ORIENTED_EDGE('',*,*,#11866,.T.);
#15586=ORIENTED_EDGE('',*,*,#11869,.T.);
#15587=ORIENTED_EDGE('',*,*,#11870,.T.);
#15588=ORIENTED_EDGE('',*,*,#11871,.F.);
#15589=ORIENTED_EDGE('',*,*,#11865,.T.);
#15590=ORIENTED_EDGE('',*,*,#11872,.T.);
#15591=ORIENTED_EDGE('',*,*,#11873,.T.);
#15592=ORIENTED_EDGE('',*,*,#11869,.F.);
#15593=ORIENTED_EDGE('',*,*,#11864,.T.);
#15594=ORIENTED_EDGE('',*,*,#11874,.T.);
#15595=ORIENTED_EDGE('',*,*,#11875,.T.);
#15596=ORIENTED_EDGE('',*,*,#11872,.F.);
#15597=ORIENTED_EDGE('',*,*,#11870,.F.);
#15598=ORIENTED_EDGE('',*,*,#11873,.F.);
#15599=ORIENTED_EDGE('',*,*,#11875,.F.);
#15600=ORIENTED_EDGE('',*,*,#11876,.F.);
#15601=ORIENTED_EDGE('',*,*,#11877,.F.);
#15602=ORIENTED_EDGE('',*,*,#11878,.T.);
#15603=ORIENTED_EDGE('',*,*,#11879,.F.);
#15604=ORIENTED_EDGE('',*,*,#11878,.F.);
#15605=ORIENTED_EDGE('',*,*,#11880,.F.);
#15606=ORIENTED_EDGE('',*,*,#11881,.F.);
#15607=ORIENTED_EDGE('',*,*,#11863,.T.);
#15608=ORIENTED_EDGE('',*,*,#11882,.T.);
#15609=ORIENTED_EDGE('',*,*,#11876,.T.);
#15610=ORIENTED_EDGE('',*,*,#11874,.F.);
#15611=ORIENTED_EDGE('',*,*,#11879,.T.);
#15612=ORIENTED_EDGE('',*,*,#11883,.F.);
#15613=ORIENTED_EDGE('',*,*,#11860,.T.);
#15614=ORIENTED_EDGE('',*,*,#11884,.F.);
#15615=ORIENTED_EDGE('',*,*,#11867,.T.);
#15616=ORIENTED_EDGE('',*,*,#11871,.T.);
#15617=ORIENTED_EDGE('',*,*,#11881,.T.);
#15618=ORIENTED_EDGE('',*,*,#11885,.F.);
#15619=ORIENTED_EDGE('',*,*,#11862,.T.);
#15620=ORIENTED_EDGE('',*,*,#11868,.T.);
#15621=ORIENTED_EDGE('',*,*,#11885,.T.);
#15622=ORIENTED_EDGE('',*,*,#11880,.T.);
#15623=ORIENTED_EDGE('',*,*,#11877,.T.);
#15624=ORIENTED_EDGE('',*,*,#11882,.F.);
#15625=ORIENTED_EDGE('',*,*,#11886,.F.);
#15626=ORIENTED_EDGE('',*,*,#11887,.T.);
#15627=ORIENTED_EDGE('',*,*,#11888,.T.);
#15628=ORIENTED_EDGE('',*,*,#11887,.F.);
#15629=ORIENTED_EDGE('',*,*,#11888,.F.);
#15630=ORIENTED_EDGE('',*,*,#11889,.T.);
#15631=ORIENTED_EDGE('',*,*,#11889,.F.);
#15632=ORIENTED_EDGE('',*,*,#11890,.F.);
#15633=ORIENTED_EDGE('',*,*,#11886,.T.);
#15634=ORIENTED_EDGE('',*,*,#11559,.F.);
#15635=ORIENTED_EDGE('',*,*,#11560,.F.);
#15636=ORIENTED_EDGE('',*,*,#11891,.T.);
#15637=ORIENTED_EDGE('',*,*,#11890,.T.);
#15638=ORIENTED_EDGE('',*,*,#11891,.F.);
#15639=ORIENTED_EDGE('',*,*,#11549,.T.);
#15640=ORIENTED_EDGE('',*,*,#11553,.T.);
#15641=ORIENTED_EDGE('',*,*,#11556,.T.);
#15642=ORIENTED_EDGE('',*,*,#11525,.T.);
#15643=ORIENTED_EDGE('',*,*,#11565,.T.);
#15644=ORIENTED_EDGE('',*,*,#11567,.T.);
#15645=ORIENTED_EDGE('',*,*,#11569,.T.);
#15646=ORIENTED_EDGE('',*,*,#11892,.F.);
#15647=ORIENTED_EDGE('',*,*,#11884,.T.);
#15648=ORIENTED_EDGE('',*,*,#11893,.T.);
#15649=ORIENTED_EDGE('',*,*,#11892,.T.);
#15650=ORIENTED_EDGE('',*,*,#11893,.F.);
#15651=ORIENTED_EDGE('',*,*,#11588,.T.);
#15652=ORIENTED_EDGE('',*,*,#11894,.F.);
#15653=ORIENTED_EDGE('',*,*,#11848,.T.);
#15654=ORIENTED_EDGE('',*,*,#11850,.T.);
#15655=ORIENTED_EDGE('',*,*,#11842,.T.);
#15656=ORIENTED_EDGE('',*,*,#11895,.F.);
#15657=ORIENTED_EDGE('',*,*,#11603,.T.);
#15658=ORIENTED_EDGE('',*,*,#11605,.T.);
#15659=ORIENTED_EDGE('',*,*,#11597,.T.);
#15660=ORIENTED_EDGE('',*,*,#11896,.F.);
#15661=ORIENTED_EDGE('',*,*,#11839,.T.);
#15662=ORIENTED_EDGE('',*,*,#11841,.T.);
#15663=ORIENTED_EDGE('',*,*,#11833,.T.);
#15664=ORIENTED_EDGE('',*,*,#11897,.F.);
#15665=ORIENTED_EDGE('',*,*,#11612,.T.);
#15666=ORIENTED_EDGE('',*,*,#11614,.T.);
#15667=ORIENTED_EDGE('',*,*,#11606,.T.);
#15668=ORIENTED_EDGE('',*,*,#11898,.F.);
#15669=ORIENTED_EDGE('',*,*,#11830,.T.);
#15670=ORIENTED_EDGE('',*,*,#11832,.T.);
#15671=ORIENTED_EDGE('',*,*,#11824,.T.);
#15672=ORIENTED_EDGE('',*,*,#11899,.F.);
#15673=ORIENTED_EDGE('',*,*,#11621,.T.);
#15674=ORIENTED_EDGE('',*,*,#11623,.T.);
#15675=ORIENTED_EDGE('',*,*,#11615,.T.);
#15676=ORIENTED_EDGE('',*,*,#11900,.F.);
#15677=ORIENTED_EDGE('',*,*,#11821,.T.);
#15678=ORIENTED_EDGE('',*,*,#11823,.T.);
#15679=ORIENTED_EDGE('',*,*,#11815,.T.);
#15680=ORIENTED_EDGE('',*,*,#11901,.F.);
#15681=ORIENTED_EDGE('',*,*,#11630,.T.);
#15682=ORIENTED_EDGE('',*,*,#11632,.T.);
#15683=ORIENTED_EDGE('',*,*,#11624,.T.);
#15684=ORIENTED_EDGE('',*,*,#11902,.F.);
#15685=ORIENTED_EDGE('',*,*,#11812,.T.);
#15686=ORIENTED_EDGE('',*,*,#11814,.T.);
#15687=ORIENTED_EDGE('',*,*,#11806,.T.);
#15688=ORIENTED_EDGE('',*,*,#11903,.F.);
#15689=ORIENTED_EDGE('',*,*,#11639,.T.);
#15690=ORIENTED_EDGE('',*,*,#11641,.T.);
#15691=ORIENTED_EDGE('',*,*,#11633,.T.);
#15692=ORIENTED_EDGE('',*,*,#11904,.F.);
#15693=ORIENTED_EDGE('',*,*,#11803,.T.);
#15694=ORIENTED_EDGE('',*,*,#11805,.T.);
#15695=ORIENTED_EDGE('',*,*,#11797,.T.);
#15696=ORIENTED_EDGE('',*,*,#11905,.F.);
#15697=ORIENTED_EDGE('',*,*,#11648,.T.);
#15698=ORIENTED_EDGE('',*,*,#11650,.T.);
#15699=ORIENTED_EDGE('',*,*,#11642,.T.);
#15700=ORIENTED_EDGE('',*,*,#11906,.F.);
#15701=ORIENTED_EDGE('',*,*,#11793,.T.);
#15702=ORIENTED_EDGE('',*,*,#11795,.T.);
#15703=ORIENTED_EDGE('',*,*,#11907,.T.);
#15704=ORIENTED_EDGE('',*,*,#11883,.T.);
#15705=ORIENTED_EDGE('',*,*,#11907,.F.);
#15706=ORIENTED_EDGE('',*,*,#11796,.T.);
#15707=ORIENTED_EDGE('',*,*,#11786,.T.);
#15708=ORIENTED_EDGE('',*,*,#11908,.F.);
#15709=ORIENTED_EDGE('',*,*,#11783,.T.);
#15710=ORIENTED_EDGE('',*,*,#11785,.T.);
#15711=ORIENTED_EDGE('',*,*,#11777,.T.);
#15712=ORIENTED_EDGE('',*,*,#11909,.F.);
#15713=ORIENTED_EDGE('',*,*,#11666,.T.);
#15714=ORIENTED_EDGE('',*,*,#11668,.T.);
#15715=ORIENTED_EDGE('',*,*,#11660,.T.);
#15716=ORIENTED_EDGE('',*,*,#11910,.F.);
#15717=ORIENTED_EDGE('',*,*,#11774,.T.);
#15718=ORIENTED_EDGE('',*,*,#11776,.T.);
#15719=ORIENTED_EDGE('',*,*,#11768,.T.);
#15720=ORIENTED_EDGE('',*,*,#11911,.F.);
#15721=ORIENTED_EDGE('',*,*,#11675,.T.);
#15722=ORIENTED_EDGE('',*,*,#11677,.T.);
#15723=ORIENTED_EDGE('',*,*,#11669,.T.);
#15724=ORIENTED_EDGE('',*,*,#11912,.F.);
#15725=ORIENTED_EDGE('',*,*,#11765,.T.);
#15726=ORIENTED_EDGE('',*,*,#11767,.T.);
#15727=ORIENTED_EDGE('',*,*,#11759,.T.);
#15728=ORIENTED_EDGE('',*,*,#11913,.F.);
#15729=ORIENTED_EDGE('',*,*,#11684,.T.);
#15730=ORIENTED_EDGE('',*,*,#11686,.T.);
#15731=ORIENTED_EDGE('',*,*,#11678,.T.);
#15732=ORIENTED_EDGE('',*,*,#11914,.F.);
#15733=ORIENTED_EDGE('',*,*,#11756,.T.);
#15734=ORIENTED_EDGE('',*,*,#11758,.T.);
#15735=ORIENTED_EDGE('',*,*,#11750,.T.);
#15736=ORIENTED_EDGE('',*,*,#11915,.F.);
#15737=ORIENTED_EDGE('',*,*,#11693,.T.);
#15738=ORIENTED_EDGE('',*,*,#11695,.T.);
#15739=ORIENTED_EDGE('',*,*,#11687,.T.);
#15740=ORIENTED_EDGE('',*,*,#11916,.F.);
#15741=ORIENTED_EDGE('',*,*,#11747,.T.);
#15742=ORIENTED_EDGE('',*,*,#11749,.T.);
#15743=ORIENTED_EDGE('',*,*,#11741,.T.);
#15744=ORIENTED_EDGE('',*,*,#11917,.F.);
#15745=ORIENTED_EDGE('',*,*,#11702,.T.);
#15746=ORIENTED_EDGE('',*,*,#11704,.T.);
#15747=ORIENTED_EDGE('',*,*,#11696,.T.);
#15748=ORIENTED_EDGE('',*,*,#11918,.F.);
#15749=ORIENTED_EDGE('',*,*,#11738,.T.);
#15750=ORIENTED_EDGE('',*,*,#11740,.T.);
#15751=ORIENTED_EDGE('',*,*,#11732,.T.);
#15752=ORIENTED_EDGE('',*,*,#11919,.F.);
#15753=ORIENTED_EDGE('',*,*,#11711,.T.);
#15754=ORIENTED_EDGE('',*,*,#11713,.T.);
#15755=ORIENTED_EDGE('',*,*,#11705,.T.);
#15756=ORIENTED_EDGE('',*,*,#11920,.F.);
#15757=ORIENTED_EDGE('',*,*,#11729,.T.);
#15758=ORIENTED_EDGE('',*,*,#11731,.T.);
#15759=ORIENTED_EDGE('',*,*,#11723,.T.);
#15760=ORIENTED_EDGE('',*,*,#11921,.F.);
#15761=ORIENTED_EDGE('',*,*,#11720,.T.);
#15762=ORIENTED_EDGE('',*,*,#11722,.T.);
#15763=ORIENTED_EDGE('',*,*,#11714,.T.);
#15764=ORIENTED_EDGE('',*,*,#11922,.F.);
#15765=ORIENTED_EDGE('',*,*,#11657,.T.);
#15766=ORIENTED_EDGE('',*,*,#11659,.T.);
#15767=ORIENTED_EDGE('',*,*,#11654,.T.);
#15768=ORIENTED_EDGE('',*,*,#11923,.F.);
#15769=ORIENTED_EDGE('',*,*,#11857,.T.);
#15770=ORIENTED_EDGE('',*,*,#11859,.T.);
#15771=ORIENTED_EDGE('',*,*,#11851,.T.);
#15772=ORIENTED_EDGE('',*,*,#11924,.F.);
#15773=ORIENTED_EDGE('',*,*,#11594,.T.);
#15774=ORIENTED_EDGE('',*,*,#11596,.T.);
#15775=ORIENTED_EDGE('',*,*,#11925,.F.);
#15776=ORIENTED_EDGE('',*,*,#11926,.T.);
#15777=ORIENTED_EDGE('',*,*,#11792,.T.);
#15778=ORIENTED_EDGE('',*,*,#11906,.T.);
#15779=ORIENTED_EDGE('',*,*,#11646,.T.);
#15780=ORIENTED_EDGE('',*,*,#11905,.T.);
#15781=ORIENTED_EDGE('',*,*,#11801,.T.);
#15782=ORIENTED_EDGE('',*,*,#11904,.T.);
#15783=ORIENTED_EDGE('',*,*,#11637,.T.);
#15784=ORIENTED_EDGE('',*,*,#11903,.T.);
#15785=ORIENTED_EDGE('',*,*,#11810,.T.);
#15786=ORIENTED_EDGE('',*,*,#11902,.T.);
#15787=ORIENTED_EDGE('',*,*,#11628,.T.);
#15788=ORIENTED_EDGE('',*,*,#11901,.T.);
#15789=ORIENTED_EDGE('',*,*,#11819,.T.);
#15790=ORIENTED_EDGE('',*,*,#11900,.T.);
#15791=ORIENTED_EDGE('',*,*,#11619,.T.);
#15792=ORIENTED_EDGE('',*,*,#11899,.T.);
#15793=ORIENTED_EDGE('',*,*,#11828,.T.);
#15794=ORIENTED_EDGE('',*,*,#11898,.T.);
#15795=ORIENTED_EDGE('',*,*,#11610,.T.);
#15796=ORIENTED_EDGE('',*,*,#11897,.T.);
#15797=ORIENTED_EDGE('',*,*,#11837,.T.);
#15798=ORIENTED_EDGE('',*,*,#11896,.T.);
#15799=ORIENTED_EDGE('',*,*,#11601,.T.);
#15800=ORIENTED_EDGE('',*,*,#11895,.T.);
#15801=ORIENTED_EDGE('',*,*,#11846,.T.);
#15802=ORIENTED_EDGE('',*,*,#11894,.T.);
#15803=ORIENTED_EDGE('',*,*,#11592,.T.);
#15804=ORIENTED_EDGE('',*,*,#11924,.T.);
#15805=ORIENTED_EDGE('',*,*,#11855,.T.);
#15806=ORIENTED_EDGE('',*,*,#11923,.T.);
#15807=ORIENTED_EDGE('',*,*,#11651,.T.);
#15808=ORIENTED_EDGE('',*,*,#11922,.T.);
#15809=ORIENTED_EDGE('',*,*,#11718,.T.);
#15810=ORIENTED_EDGE('',*,*,#11921,.T.);
#15811=ORIENTED_EDGE('',*,*,#11727,.T.);
#15812=ORIENTED_EDGE('',*,*,#11920,.T.);
#15813=ORIENTED_EDGE('',*,*,#11709,.T.);
#15814=ORIENTED_EDGE('',*,*,#11919,.T.);
#15815=ORIENTED_EDGE('',*,*,#11736,.T.);
#15816=ORIENTED_EDGE('',*,*,#11918,.T.);
#15817=ORIENTED_EDGE('',*,*,#11700,.T.);
#15818=ORIENTED_EDGE('',*,*,#11917,.T.);
#15819=ORIENTED_EDGE('',*,*,#11745,.T.);
#15820=ORIENTED_EDGE('',*,*,#11916,.T.);
#15821=ORIENTED_EDGE('',*,*,#11691,.T.);
#15822=ORIENTED_EDGE('',*,*,#11915,.T.);
#15823=ORIENTED_EDGE('',*,*,#11754,.T.);
#15824=ORIENTED_EDGE('',*,*,#11914,.T.);
#15825=ORIENTED_EDGE('',*,*,#11682,.T.);
#15826=ORIENTED_EDGE('',*,*,#11913,.T.);
#15827=ORIENTED_EDGE('',*,*,#11763,.T.);
#15828=ORIENTED_EDGE('',*,*,#11912,.T.);
#15829=ORIENTED_EDGE('',*,*,#11673,.T.);
#15830=ORIENTED_EDGE('',*,*,#11911,.T.);
#15831=ORIENTED_EDGE('',*,*,#11772,.T.);
#15832=ORIENTED_EDGE('',*,*,#11910,.T.);
#15833=ORIENTED_EDGE('',*,*,#11664,.T.);
#15834=ORIENTED_EDGE('',*,*,#11909,.T.);
#15835=ORIENTED_EDGE('',*,*,#11781,.T.);
#15836=ORIENTED_EDGE('',*,*,#11908,.T.);
#15837=ORIENTED_EDGE('',*,*,#11790,.T.);
#15838=ORIENTED_EDGE('',*,*,#11926,.F.);
#15839=ORIENTED_EDGE('',*,*,#11925,.T.);
#15840=ORIENTED_EDGE('',*,*,#11570,.T.);
#15841=ORIENTED_EDGE('',*,*,#11586,.T.);
#15842=ORIENTED_EDGE('',*,*,#11583,.T.);
#15843=ORIENTED_EDGE('',*,*,#11580,.T.);
#15844=ORIENTED_EDGE('',*,*,#11577,.T.);
#15845=ORIENTED_EDGE('',*,*,#11574,.T.);
#15846=ORIENTED_EDGE('',*,*,#11927,.F.);
#15847=ORIENTED_EDGE('',*,*,#11928,.T.);
#15848=ORIENTED_EDGE('',*,*,#11929,.F.);
#15849=ORIENTED_EDGE('',*,*,#11930,.F.);
#15850=ORIENTED_EDGE('',*,*,#11931,.F.);
#15851=ORIENTED_EDGE('',*,*,#11932,.T.);
#15852=ORIENTED_EDGE('',*,*,#11927,.T.);
#15853=ORIENTED_EDGE('',*,*,#11933,.F.);
#15854=ORIENTED_EDGE('',*,*,#11934,.F.);
#15855=ORIENTED_EDGE('',*,*,#11935,.T.);
#15856=ORIENTED_EDGE('',*,*,#11931,.T.);
#15857=ORIENTED_EDGE('',*,*,#11936,.F.);
#15858=ORIENTED_EDGE('',*,*,#11937,.F.);
#15859=ORIENTED_EDGE('',*,*,#11938,.T.);
#15860=ORIENTED_EDGE('',*,*,#11934,.T.);
#15861=ORIENTED_EDGE('',*,*,#11939,.F.);
#15862=ORIENTED_EDGE('',*,*,#11940,.F.);
#15863=ORIENTED_EDGE('',*,*,#11941,.F.);
#15864=ORIENTED_EDGE('',*,*,#11942,.T.);
#15865=ORIENTED_EDGE('',*,*,#11937,.T.);
#15866=ORIENTED_EDGE('',*,*,#11943,.F.);
#15867=ORIENTED_EDGE('',*,*,#11944,.F.);
#15868=ORIENTED_EDGE('',*,*,#11945,.T.);
#15869=ORIENTED_EDGE('',*,*,#11946,.T.);
#15870=ORIENTED_EDGE('',*,*,#11947,.T.);
#15871=ORIENTED_EDGE('',*,*,#11948,.F.);
#15872=ORIENTED_EDGE('',*,*,#11949,.T.);
#15873=ORIENTED_EDGE('',*,*,#11944,.T.);
#15874=ORIENTED_EDGE('',*,*,#11950,.T.);
#15875=ORIENTED_EDGE('',*,*,#11951,.F.);
#15876=ORIENTED_EDGE('',*,*,#11952,.T.);
#15877=ORIENTED_EDGE('',*,*,#11948,.T.);
#15878=ORIENTED_EDGE('',*,*,#11953,.T.);
#15879=ORIENTED_EDGE('',*,*,#11954,.F.);
#15880=ORIENTED_EDGE('',*,*,#11955,.T.);
#15881=ORIENTED_EDGE('',*,*,#11951,.T.);
#15882=ORIENTED_EDGE('',*,*,#11956,.T.);
#15883=ORIENTED_EDGE('',*,*,#11957,.F.);
#15884=ORIENTED_EDGE('',*,*,#11958,.T.);
#15885=ORIENTED_EDGE('',*,*,#11954,.T.);
#15886=ORIENTED_EDGE('',*,*,#11959,.T.);
#15887=ORIENTED_EDGE('',*,*,#11960,.F.);
#15888=ORIENTED_EDGE('',*,*,#11961,.T.);
#15889=ORIENTED_EDGE('',*,*,#11957,.T.);
#15890=ORIENTED_EDGE('',*,*,#11962,.T.);
#15891=ORIENTED_EDGE('',*,*,#11963,.F.);
#15892=ORIENTED_EDGE('',*,*,#11964,.T.);
#15893=ORIENTED_EDGE('',*,*,#11960,.T.);
#15894=ORIENTED_EDGE('',*,*,#11965,.T.);
#15895=ORIENTED_EDGE('',*,*,#11966,.F.);
#15896=ORIENTED_EDGE('',*,*,#11967,.T.);
#15897=ORIENTED_EDGE('',*,*,#11968,.F.);
#15898=ORIENTED_EDGE('',*,*,#11969,.F.);
#15899=ORIENTED_EDGE('',*,*,#11970,.F.);
#15900=ORIENTED_EDGE('',*,*,#11971,.T.);
#15901=ORIENTED_EDGE('',*,*,#11966,.T.);
#15902=ORIENTED_EDGE('',*,*,#11972,.F.);
#15903=ORIENTED_EDGE('',*,*,#11973,.F.);
#15904=ORIENTED_EDGE('',*,*,#11974,.T.);
#15905=ORIENTED_EDGE('',*,*,#11970,.T.);
#15906=ORIENTED_EDGE('',*,*,#11975,.F.);
#15907=ORIENTED_EDGE('',*,*,#11976,.F.);
#15908=ORIENTED_EDGE('',*,*,#11977,.T.);
#15909=ORIENTED_EDGE('',*,*,#11973,.T.);
#15910=ORIENTED_EDGE('',*,*,#11978,.F.);
#15911=ORIENTED_EDGE('',*,*,#11979,.F.);
#15912=ORIENTED_EDGE('',*,*,#11980,.T.);
#15913=ORIENTED_EDGE('',*,*,#11976,.T.);
#15914=ORIENTED_EDGE('',*,*,#11981,.F.);
#15915=ORIENTED_EDGE('',*,*,#11982,.F.);
#15916=ORIENTED_EDGE('',*,*,#11983,.T.);
#15917=ORIENTED_EDGE('',*,*,#11979,.T.);
#15918=ORIENTED_EDGE('',*,*,#11984,.F.);
#15919=ORIENTED_EDGE('',*,*,#11985,.F.);
#15920=ORIENTED_EDGE('',*,*,#11986,.T.);
#15921=ORIENTED_EDGE('',*,*,#11982,.T.);
#15922=ORIENTED_EDGE('',*,*,#11987,.F.);
#15923=ORIENTED_EDGE('',*,*,#11968,.T.);
#15924=ORIENTED_EDGE('',*,*,#11988,.T.);
#15925=ORIENTED_EDGE('',*,*,#11989,.F.);
#15926=ORIENTED_EDGE('',*,*,#11990,.F.);
#15927=ORIENTED_EDGE('',*,*,#11991,.T.);
#15928=ORIENTED_EDGE('',*,*,#11991,.F.);
#15929=ORIENTED_EDGE('',*,*,#11992,.F.);
#15930=ORIENTED_EDGE('',*,*,#11965,.F.);
#15931=ORIENTED_EDGE('',*,*,#11962,.F.);
#15932=ORIENTED_EDGE('',*,*,#11959,.F.);
#15933=ORIENTED_EDGE('',*,*,#11956,.F.);
#15934=ORIENTED_EDGE('',*,*,#11953,.F.);
#15935=ORIENTED_EDGE('',*,*,#11950,.F.);
#15936=ORIENTED_EDGE('',*,*,#11947,.F.);
#15937=ORIENTED_EDGE('',*,*,#11993,.F.);
#15938=ORIENTED_EDGE('',*,*,#11994,.T.);
#15939=ORIENTED_EDGE('',*,*,#11987,.T.);
#15940=ORIENTED_EDGE('',*,*,#11984,.T.);
#15941=ORIENTED_EDGE('',*,*,#11981,.T.);
#15942=ORIENTED_EDGE('',*,*,#11978,.T.);
#15943=ORIENTED_EDGE('',*,*,#11975,.T.);
#15944=ORIENTED_EDGE('',*,*,#11972,.T.);
#15945=ORIENTED_EDGE('',*,*,#11969,.T.);
#15946=ORIENTED_EDGE('',*,*,#11985,.T.);
#15947=ORIENTED_EDGE('',*,*,#11994,.F.);
#15948=ORIENTED_EDGE('',*,*,#11995,.F.);
#15949=ORIENTED_EDGE('',*,*,#11996,.T.);
#15950=ORIENTED_EDGE('',*,*,#11988,.F.);
#15951=ORIENTED_EDGE('',*,*,#11967,.F.);
#15952=ORIENTED_EDGE('',*,*,#11971,.F.);
#15953=ORIENTED_EDGE('',*,*,#11974,.F.);
#15954=ORIENTED_EDGE('',*,*,#11977,.F.);
#15955=ORIENTED_EDGE('',*,*,#11980,.F.);
#15956=ORIENTED_EDGE('',*,*,#11983,.F.);
#15957=ORIENTED_EDGE('',*,*,#11986,.F.);
#15958=ORIENTED_EDGE('',*,*,#11996,.F.);
#15959=ORIENTED_EDGE('',*,*,#11997,.F.);
#15960=ORIENTED_EDGE('',*,*,#11945,.F.);
#15961=ORIENTED_EDGE('',*,*,#11949,.F.);
#15962=ORIENTED_EDGE('',*,*,#11952,.F.);
#15963=ORIENTED_EDGE('',*,*,#11955,.F.);
#15964=ORIENTED_EDGE('',*,*,#11958,.F.);
#15965=ORIENTED_EDGE('',*,*,#11961,.F.);
#15966=ORIENTED_EDGE('',*,*,#11964,.F.);
#15967=ORIENTED_EDGE('',*,*,#11998,.F.);
#15968=ORIENTED_EDGE('',*,*,#11963,.T.);
#15969=ORIENTED_EDGE('',*,*,#11992,.T.);
#15970=ORIENTED_EDGE('',*,*,#11999,.F.);
#15971=ORIENTED_EDGE('',*,*,#11998,.T.);
#15972=ORIENTED_EDGE('',*,*,#12000,.F.);
#15973=ORIENTED_EDGE('',*,*,#12001,.F.);
#15974=ORIENTED_EDGE('',*,*,#12002,.F.);
#15975=ORIENTED_EDGE('',*,*,#12003,.T.);
#15976=ORIENTED_EDGE('',*,*,#12004,.F.);
#15977=ORIENTED_EDGE('',*,*,#12003,.F.);
#15978=ORIENTED_EDGE('',*,*,#12005,.F.);
#15979=ORIENTED_EDGE('',*,*,#12006,.T.);
#15980=ORIENTED_EDGE('',*,*,#12007,.F.);
#15981=ORIENTED_EDGE('',*,*,#12006,.F.);
#15982=ORIENTED_EDGE('',*,*,#12008,.F.);
#15983=ORIENTED_EDGE('',*,*,#12009,.T.);
#15984=ORIENTED_EDGE('',*,*,#11943,.T.);
#15985=ORIENTED_EDGE('',*,*,#11939,.T.);
#15986=ORIENTED_EDGE('',*,*,#11936,.T.);
#15987=ORIENTED_EDGE('',*,*,#11933,.T.);
#15988=ORIENTED_EDGE('',*,*,#11930,.T.);
#15989=ORIENTED_EDGE('',*,*,#12010,.T.);
#15990=ORIENTED_EDGE('',*,*,#12011,.T.);
#15991=ORIENTED_EDGE('',*,*,#12012,.T.);
#15992=ORIENTED_EDGE('',*,*,#12013,.T.);
#15993=ORIENTED_EDGE('',*,*,#12014,.T.);
#15994=ORIENTED_EDGE('',*,*,#11941,.T.);
#15995=ORIENTED_EDGE('',*,*,#12015,.T.);
#15996=ORIENTED_EDGE('',*,*,#12008,.T.);
#15997=ORIENTED_EDGE('',*,*,#12005,.T.);
#15998=ORIENTED_EDGE('',*,*,#12002,.T.);
#15999=ORIENTED_EDGE('',*,*,#11940,.T.);
#16000=ORIENTED_EDGE('',*,*,#12009,.F.);
#16001=ORIENTED_EDGE('',*,*,#12015,.F.);
#16002=ORIENTED_EDGE('',*,*,#12016,.F.);
#16003=ORIENTED_EDGE('',*,*,#11928,.F.);
#16004=ORIENTED_EDGE('',*,*,#11932,.F.);
#16005=ORIENTED_EDGE('',*,*,#11935,.F.);
#16006=ORIENTED_EDGE('',*,*,#11938,.F.);
#16007=ORIENTED_EDGE('',*,*,#11942,.F.);
#16008=ORIENTED_EDGE('',*,*,#12014,.F.);
#16009=ORIENTED_EDGE('',*,*,#12017,.T.);
#16010=ORIENTED_EDGE('',*,*,#12018,.F.);
#16011=ORIENTED_EDGE('',*,*,#12017,.F.);
#16012=ORIENTED_EDGE('',*,*,#12013,.F.);
#16013=ORIENTED_EDGE('',*,*,#12019,.T.);
#16014=ORIENTED_EDGE('',*,*,#12020,.F.);
#16015=ORIENTED_EDGE('',*,*,#12019,.F.);
#16016=ORIENTED_EDGE('',*,*,#12012,.F.);
#16017=ORIENTED_EDGE('',*,*,#12001,.T.);
#16018=ORIENTED_EDGE('',*,*,#12021,.F.);
#16019=ORIENTED_EDGE('',*,*,#12022,.T.);
#16020=ORIENTED_EDGE('',*,*,#12023,.F.);
#16021=ORIENTED_EDGE('',*,*,#12024,.F.);
#16022=ORIENTED_EDGE('',*,*,#12025,.F.);
#16023=ORIENTED_EDGE('',*,*,#12026,.F.);
#16024=ORIENTED_EDGE('',*,*,#12027,.F.);
#16025=ORIENTED_EDGE('',*,*,#12028,.F.);
#16026=ORIENTED_EDGE('',*,*,#12029,.F.);
#16027=ORIENTED_EDGE('',*,*,#12022,.F.);
#16028=ORIENTED_EDGE('',*,*,#12027,.T.);
#16029=ORIENTED_EDGE('',*,*,#12030,.T.);
#16030=ORIENTED_EDGE('',*,*,#12031,.T.);
#16031=ORIENTED_EDGE('',*,*,#12032,.F.);
#16032=ORIENTED_EDGE('',*,*,#12026,.T.);
#16033=ORIENTED_EDGE('',*,*,#12033,.T.);
#16034=ORIENTED_EDGE('',*,*,#12034,.T.);
#16035=ORIENTED_EDGE('',*,*,#12030,.F.);
#16036=ORIENTED_EDGE('',*,*,#12025,.T.);
#16037=ORIENTED_EDGE('',*,*,#12035,.T.);
#16038=ORIENTED_EDGE('',*,*,#12036,.T.);
#16039=ORIENTED_EDGE('',*,*,#12033,.F.);
#16040=ORIENTED_EDGE('',*,*,#12031,.F.);
#16041=ORIENTED_EDGE('',*,*,#12034,.F.);
#16042=ORIENTED_EDGE('',*,*,#12036,.F.);
#16043=ORIENTED_EDGE('',*,*,#12037,.F.);
#16044=ORIENTED_EDGE('',*,*,#12038,.F.);
#16045=ORIENTED_EDGE('',*,*,#12039,.T.);
#16046=ORIENTED_EDGE('',*,*,#12040,.F.);
#16047=ORIENTED_EDGE('',*,*,#12039,.F.);
#16048=ORIENTED_EDGE('',*,*,#12041,.F.);
#16049=ORIENTED_EDGE('',*,*,#12042,.F.);
#16050=ORIENTED_EDGE('',*,*,#12024,.T.);
#16051=ORIENTED_EDGE('',*,*,#12043,.T.);
#16052=ORIENTED_EDGE('',*,*,#12037,.T.);
#16053=ORIENTED_EDGE('',*,*,#12035,.F.);
#16054=ORIENTED_EDGE('',*,*,#12040,.T.);
#16055=ORIENTED_EDGE('',*,*,#11997,.T.);
#16056=ORIENTED_EDGE('',*,*,#11995,.T.);
#16057=ORIENTED_EDGE('',*,*,#11993,.T.);
#16058=ORIENTED_EDGE('',*,*,#11946,.F.);
#16059=ORIENTED_EDGE('',*,*,#12044,.F.);
#16060=ORIENTED_EDGE('',*,*,#12021,.T.);
#16061=ORIENTED_EDGE('',*,*,#12045,.F.);
#16062=ORIENTED_EDGE('',*,*,#12046,.F.);
#16063=ORIENTED_EDGE('',*,*,#12028,.T.);
#16064=ORIENTED_EDGE('',*,*,#12032,.T.);
#16065=ORIENTED_EDGE('',*,*,#12042,.T.);
#16066=ORIENTED_EDGE('',*,*,#12047,.F.);
#16067=ORIENTED_EDGE('',*,*,#12023,.T.);
#16068=ORIENTED_EDGE('',*,*,#12029,.T.);
#16069=ORIENTED_EDGE('',*,*,#12047,.T.);
#16070=ORIENTED_EDGE('',*,*,#12041,.T.);
#16071=ORIENTED_EDGE('',*,*,#12038,.T.);
#16072=ORIENTED_EDGE('',*,*,#12043,.F.);
#16073=ORIENTED_EDGE('',*,*,#12046,.T.);
#16074=ORIENTED_EDGE('',*,*,#12048,.T.);
#16075=ORIENTED_EDGE('',*,*,#12049,.F.);
#16076=ORIENTED_EDGE('',*,*,#12048,.F.);
#16077=ORIENTED_EDGE('',*,*,#12050,.T.);
#16078=ORIENTED_EDGE('',*,*,#12051,.T.);
#16079=ORIENTED_EDGE('',*,*,#12044,.T.);
#16080=ORIENTED_EDGE('',*,*,#12051,.F.);
#16081=ORIENTED_EDGE('',*,*,#12052,.F.);
#16082=ORIENTED_EDGE('',*,*,#12049,.T.);
#16083=ORIENTED_EDGE('',*,*,#12010,.F.);
#16084=ORIENTED_EDGE('',*,*,#12011,.F.);
#16085=ORIENTED_EDGE('',*,*,#12053,.T.);
#16086=ORIENTED_EDGE('',*,*,#12052,.T.);
#16087=ORIENTED_EDGE('',*,*,#12053,.F.);
#16088=ORIENTED_EDGE('',*,*,#12000,.T.);
#16089=ORIENTED_EDGE('',*,*,#12004,.T.);
#16090=ORIENTED_EDGE('',*,*,#12007,.T.);
#16091=ORIENTED_EDGE('',*,*,#11929,.T.);
#16092=ORIENTED_EDGE('',*,*,#12016,.T.);
#16093=ORIENTED_EDGE('',*,*,#12018,.T.);
#16094=ORIENTED_EDGE('',*,*,#12020,.T.);
#16095=ORIENTED_EDGE('',*,*,#12054,.F.);
#16096=ORIENTED_EDGE('',*,*,#12045,.T.);
#16097=ORIENTED_EDGE('',*,*,#12055,.T.);
#16098=ORIENTED_EDGE('',*,*,#12054,.T.);
#16099=ORIENTED_EDGE('',*,*,#12055,.F.);
#16100=ORIENTED_EDGE('',*,*,#12056,.F.);
#16101=ORIENTED_EDGE('',*,*,#12057,.T.);
#16102=ORIENTED_EDGE('',*,*,#11989,.T.);
#16103=ORIENTED_EDGE('',*,*,#11999,.T.);
#16104=ORIENTED_EDGE('',*,*,#11990,.T.);
#16105=ORIENTED_EDGE('',*,*,#12057,.F.);
#16106=ORIENTED_EDGE('',*,*,#12056,.T.);
#16107=ORIENTED_EDGE('',*,*,#12058,.F.);
#16108=ORIENTED_EDGE('',*,*,#12058,.T.);
#16109=ORIENTED_EDGE('',*,*,#12059,.T.);
#16110=ORIENTED_EDGE('',*,*,#12050,.F.);
#16111=ORIENTED_EDGE('',*,*,#12059,.F.);
#16112=ORIENTED_EDGE('',*,*,#12060,.F.);
#16113=ORIENTED_EDGE('',*,*,#12061,.T.);
#16114=ORIENTED_EDGE('',*,*,#12062,.T.);
#16115=ORIENTED_EDGE('',*,*,#12061,.F.);
#16116=ORIENTED_EDGE('',*,*,#12062,.F.);
#16117=ORIENTED_EDGE('',*,*,#12063,.T.);
#16118=ORIENTED_EDGE('',*,*,#12063,.F.);
#16119=ORIENTED_EDGE('',*,*,#12064,.F.);
#16120=ORIENTED_EDGE('',*,*,#12065,.F.);
#16121=ORIENTED_EDGE('',*,*,#12066,.T.);
#16122=ORIENTED_EDGE('',*,*,#12067,.T.);
#16123=ORIENTED_EDGE('',*,*,#12068,.F.);
#16124=ORIENTED_EDGE('',*,*,#12067,.F.);
#16125=ORIENTED_EDGE('',*,*,#12069,.F.);
#16126=ORIENTED_EDGE('',*,*,#12070,.T.);
#16127=ORIENTED_EDGE('',*,*,#12071,.F.);
#16128=ORIENTED_EDGE('',*,*,#12070,.F.);
#16129=ORIENTED_EDGE('',*,*,#12072,.T.);
#16130=ORIENTED_EDGE('',*,*,#12073,.T.);
#16131=ORIENTED_EDGE('',*,*,#12074,.F.);
#16132=ORIENTED_EDGE('',*,*,#12073,.F.);
#16133=ORIENTED_EDGE('',*,*,#12075,.F.);
#16134=ORIENTED_EDGE('',*,*,#12065,.T.);
#16135=ORIENTED_EDGE('',*,*,#12069,.T.);
#16136=ORIENTED_EDGE('',*,*,#12066,.F.);
#16137=ORIENTED_EDGE('',*,*,#12075,.T.);
#16138=ORIENTED_EDGE('',*,*,#12072,.F.);
#16139=ORIENTED_EDGE('',*,*,#12076,.F.);
#16140=ORIENTED_EDGE('',*,*,#12077,.F.);
#16141=ORIENTED_EDGE('',*,*,#12078,.T.);
#16142=ORIENTED_EDGE('',*,*,#12079,.T.);
#16143=ORIENTED_EDGE('',*,*,#12080,.F.);
#16144=ORIENTED_EDGE('',*,*,#12079,.F.);
#16145=ORIENTED_EDGE('',*,*,#12081,.F.);
#16146=ORIENTED_EDGE('',*,*,#12082,.T.);
#16147=ORIENTED_EDGE('',*,*,#12083,.F.);
#16148=ORIENTED_EDGE('',*,*,#12082,.F.);
#16149=ORIENTED_EDGE('',*,*,#12084,.T.);
#16150=ORIENTED_EDGE('',*,*,#12085,.T.);
#16151=ORIENTED_EDGE('',*,*,#12086,.F.);
#16152=ORIENTED_EDGE('',*,*,#12085,.F.);
#16153=ORIENTED_EDGE('',*,*,#12087,.F.);
#16154=ORIENTED_EDGE('',*,*,#12077,.T.);
#16155=ORIENTED_EDGE('',*,*,#12081,.T.);
#16156=ORIENTED_EDGE('',*,*,#12078,.F.);
#16157=ORIENTED_EDGE('',*,*,#12087,.T.);
#16158=ORIENTED_EDGE('',*,*,#12084,.F.);
#16159=ORIENTED_EDGE('',*,*,#12088,.F.);
#16160=ORIENTED_EDGE('',*,*,#12060,.T.);
#16161=ORIENTED_EDGE('',*,*,#12089,.F.);
#16162=ORIENTED_EDGE('',*,*,#12090,.T.);
#16163=ORIENTED_EDGE('',*,*,#12088,.T.);
#16164=ORIENTED_EDGE('',*,*,#12090,.F.);
#16165=ORIENTED_EDGE('',*,*,#12091,.F.);
#16166=ORIENTED_EDGE('',*,*,#12092,.T.);
#16167=ORIENTED_EDGE('',*,*,#12089,.T.);
#16168=ORIENTED_EDGE('',*,*,#12092,.F.);
#16169=ORIENTED_EDGE('',*,*,#12071,.T.);
#16170=ORIENTED_EDGE('',*,*,#12074,.T.);
#16171=ORIENTED_EDGE('',*,*,#12064,.T.);
#16172=ORIENTED_EDGE('',*,*,#12068,.T.);
#16173=ORIENTED_EDGE('',*,*,#12093,.F.);
#16174=ORIENTED_EDGE('',*,*,#12091,.T.);
#16175=ORIENTED_EDGE('',*,*,#12094,.F.);
#16176=ORIENTED_EDGE('',*,*,#12095,.T.);
#16177=ORIENTED_EDGE('',*,*,#12093,.T.);
#16178=ORIENTED_EDGE('',*,*,#12095,.F.);
#16179=ORIENTED_EDGE('',*,*,#12096,.F.);
#16180=ORIENTED_EDGE('',*,*,#12097,.T.);
#16181=ORIENTED_EDGE('',*,*,#12094,.T.);
#16182=ORIENTED_EDGE('',*,*,#12097,.F.);
#16183=ORIENTED_EDGE('',*,*,#12096,.T.);
#16184=ORIENTED_EDGE('',*,*,#12098,.F.);
#16185=ORIENTED_EDGE('',*,*,#12099,.F.);
#16186=ORIENTED_EDGE('',*,*,#12100,.T.);
#16187=ORIENTED_EDGE('',*,*,#12098,.T.);
#16188=ORIENTED_EDGE('',*,*,#12100,.F.);
#16189=ORIENTED_EDGE('',*,*,#12101,.F.);
#16190=ORIENTED_EDGE('',*,*,#12099,.T.);
#16191=ORIENTED_EDGE('',*,*,#12102,.F.);
#16192=ORIENTED_EDGE('',*,*,#12103,.T.);
#16193=ORIENTED_EDGE('',*,*,#12101,.T.);
#16194=ORIENTED_EDGE('',*,*,#12103,.F.);
#16195=ORIENTED_EDGE('',*,*,#12083,.T.);
#16196=ORIENTED_EDGE('',*,*,#12086,.T.);
#16197=ORIENTED_EDGE('',*,*,#12076,.T.);
#16198=ORIENTED_EDGE('',*,*,#12080,.T.);
#16199=ORIENTED_EDGE('',*,*,#12102,.T.);
#16200=ORIENTED_EDGE('',*,*,#12104,.F.);
#16201=ORIENTED_EDGE('',*,*,#12105,.F.);
#16202=ORIENTED_EDGE('',*,*,#12106,.T.);
#16203=ORIENTED_EDGE('',*,*,#12104,.T.);
#16204=ORIENTED_EDGE('',*,*,#12106,.F.);
#16205=ORIENTED_EDGE('',*,*,#12107,.F.);
#16206=ORIENTED_EDGE('',*,*,#12105,.T.);
#16207=ORIENTED_EDGE('',*,*,#12108,.F.);
#16208=ORIENTED_EDGE('',*,*,#12109,.T.);
#16209=ORIENTED_EDGE('',*,*,#12107,.T.);
#16210=ORIENTED_EDGE('',*,*,#12109,.F.);
#16211=ORIENTED_EDGE('',*,*,#12110,.F.);
#16212=ORIENTED_EDGE('',*,*,#12111,.T.);
#16213=ORIENTED_EDGE('',*,*,#12108,.T.);
#16214=ORIENTED_EDGE('',*,*,#12111,.F.);
#16215=ORIENTED_EDGE('',*,*,#12110,.T.);
#16216=ORIENTED_EDGE('',*,*,#12112,.F.);
#16217=ORIENTED_EDGE('',*,*,#12113,.T.);
#16218=ORIENTED_EDGE('',*,*,#12114,.T.);
#16219=ORIENTED_EDGE('',*,*,#12115,.T.);
#16220=ORIENTED_EDGE('',*,*,#12113,.F.);
#16221=ORIENTED_EDGE('',*,*,#12115,.F.);
#16222=ORIENTED_EDGE('',*,*,#12116,.F.);
#16223=ORIENTED_EDGE('',*,*,#12114,.F.);
#16224=ORIENTED_EDGE('',*,*,#12116,.T.);
#16225=ORIENTED_EDGE('',*,*,#12117,.T.);
#16226=ORIENTED_EDGE('',*,*,#12118,.T.);
#16227=ORIENTED_EDGE('',*,*,#12117,.F.);
#16228=ORIENTED_EDGE('',*,*,#12119,.F.);
#16229=ORIENTED_EDGE('',*,*,#12120,.F.);
#16230=ORIENTED_EDGE('',*,*,#12121,.T.);
#16231=ORIENTED_EDGE('',*,*,#12122,.F.);
#16232=ORIENTED_EDGE('',*,*,#12123,.F.);
#16233=ORIENTED_EDGE('',*,*,#12121,.F.);
#16234=ORIENTED_EDGE('',*,*,#12124,.F.);
#16235=ORIENTED_EDGE('',*,*,#12125,.T.);
#16236=ORIENTED_EDGE('',*,*,#12126,.F.);
#16237=ORIENTED_EDGE('',*,*,#12127,.F.);
#16238=ORIENTED_EDGE('',*,*,#12125,.F.);
#16239=ORIENTED_EDGE('',*,*,#12128,.F.);
#16240=ORIENTED_EDGE('',*,*,#12129,.F.);
#16241=ORIENTED_EDGE('',*,*,#12128,.T.);
#16242=ORIENTED_EDGE('',*,*,#12124,.T.);
#16243=ORIENTED_EDGE('',*,*,#12120,.T.);
#16244=ORIENTED_EDGE('',*,*,#12130,.T.);
#16245=ORIENTED_EDGE('',*,*,#12131,.F.);
#16246=ORIENTED_EDGE('',*,*,#12132,.T.);
#16247=ORIENTED_EDGE('',*,*,#12133,.F.);
#16248=ORIENTED_EDGE('',*,*,#12132,.F.);
#16249=ORIENTED_EDGE('',*,*,#12134,.F.);
#16250=ORIENTED_EDGE('',*,*,#12135,.T.);
#16251=ORIENTED_EDGE('',*,*,#12136,.F.);
#16252=ORIENTED_EDGE('',*,*,#12135,.F.);
#16253=ORIENTED_EDGE('',*,*,#12137,.F.);
#16254=ORIENTED_EDGE('',*,*,#12138,.T.);
#16255=ORIENTED_EDGE('',*,*,#12139,.F.);
#16256=ORIENTED_EDGE('',*,*,#12138,.F.);
#16257=ORIENTED_EDGE('',*,*,#12140,.F.);
#16258=ORIENTED_EDGE('',*,*,#12141,.T.);
#16259=ORIENTED_EDGE('',*,*,#12142,.F.);
#16260=ORIENTED_EDGE('',*,*,#12141,.F.);
#16261=ORIENTED_EDGE('',*,*,#12143,.F.);
#16262=ORIENTED_EDGE('',*,*,#12144,.T.);
#16263=ORIENTED_EDGE('',*,*,#12145,.F.);
#16264=ORIENTED_EDGE('',*,*,#12144,.F.);
#16265=ORIENTED_EDGE('',*,*,#12146,.F.);
#16266=ORIENTED_EDGE('',*,*,#12147,.T.);
#16267=ORIENTED_EDGE('',*,*,#12148,.F.);
#16268=ORIENTED_EDGE('',*,*,#12147,.F.);
#16269=ORIENTED_EDGE('',*,*,#12149,.F.);
#16270=ORIENTED_EDGE('',*,*,#12150,.T.);
#16271=ORIENTED_EDGE('',*,*,#12151,.F.);
#16272=ORIENTED_EDGE('',*,*,#12150,.F.);
#16273=ORIENTED_EDGE('',*,*,#12152,.F.);
#16274=ORIENTED_EDGE('',*,*,#12153,.T.);
#16275=ORIENTED_EDGE('',*,*,#12154,.F.);
#16276=ORIENTED_EDGE('',*,*,#12153,.F.);
#16277=ORIENTED_EDGE('',*,*,#12155,.F.);
#16278=ORIENTED_EDGE('',*,*,#12156,.T.);
#16279=ORIENTED_EDGE('',*,*,#12157,.F.);
#16280=ORIENTED_EDGE('',*,*,#12156,.F.);
#16281=ORIENTED_EDGE('',*,*,#12158,.F.);
#16282=ORIENTED_EDGE('',*,*,#12159,.F.);
#16283=ORIENTED_EDGE('',*,*,#12160,.T.);
#16284=ORIENTED_EDGE('',*,*,#12161,.T.);
#16285=ORIENTED_EDGE('',*,*,#12160,.F.);
#16286=ORIENTED_EDGE('',*,*,#12162,.F.);
#16287=ORIENTED_EDGE('',*,*,#12161,.F.);
#16288=ORIENTED_EDGE('',*,*,#12131,.T.);
#16289=ORIENTED_EDGE('',*,*,#12163,.F.);
#16290=ORIENTED_EDGE('',*,*,#12164,.F.);
#16291=ORIENTED_EDGE('',*,*,#12165,.T.);
#16292=ORIENTED_EDGE('',*,*,#12166,.T.);
#16293=ORIENTED_EDGE('',*,*,#12165,.F.);
#16294=ORIENTED_EDGE('',*,*,#12167,.F.);
#16295=ORIENTED_EDGE('',*,*,#12166,.F.);
#16296=ORIENTED_EDGE('',*,*,#12134,.T.);
#16297=ORIENTED_EDGE('',*,*,#12168,.F.);
#16298=ORIENTED_EDGE('',*,*,#12169,.F.);
#16299=ORIENTED_EDGE('',*,*,#12170,.T.);
#16300=ORIENTED_EDGE('',*,*,#12171,.T.);
#16301=ORIENTED_EDGE('',*,*,#12170,.F.);
#16302=ORIENTED_EDGE('',*,*,#12172,.F.);
#16303=ORIENTED_EDGE('',*,*,#12171,.F.);
#16304=ORIENTED_EDGE('',*,*,#12137,.T.);
#16305=ORIENTED_EDGE('',*,*,#12173,.F.);
#16306=ORIENTED_EDGE('',*,*,#12174,.F.);
#16307=ORIENTED_EDGE('',*,*,#12175,.T.);
#16308=ORIENTED_EDGE('',*,*,#12176,.T.);
#16309=ORIENTED_EDGE('',*,*,#12175,.F.);
#16310=ORIENTED_EDGE('',*,*,#12177,.F.);
#16311=ORIENTED_EDGE('',*,*,#12176,.F.);
#16312=ORIENTED_EDGE('',*,*,#12140,.T.);
#16313=ORIENTED_EDGE('',*,*,#12178,.F.);
#16314=ORIENTED_EDGE('',*,*,#12179,.F.);
#16315=ORIENTED_EDGE('',*,*,#12180,.T.);
#16316=ORIENTED_EDGE('',*,*,#12181,.T.);
#16317=ORIENTED_EDGE('',*,*,#12180,.F.);
#16318=ORIENTED_EDGE('',*,*,#12182,.F.);
#16319=ORIENTED_EDGE('',*,*,#12181,.F.);
#16320=ORIENTED_EDGE('',*,*,#12143,.T.);
#16321=ORIENTED_EDGE('',*,*,#12183,.F.);
#16322=ORIENTED_EDGE('',*,*,#12184,.F.);
#16323=ORIENTED_EDGE('',*,*,#12185,.T.);
#16324=ORIENTED_EDGE('',*,*,#12186,.T.);
#16325=ORIENTED_EDGE('',*,*,#12185,.F.);
#16326=ORIENTED_EDGE('',*,*,#12187,.F.);
#16327=ORIENTED_EDGE('',*,*,#12186,.F.);
#16328=ORIENTED_EDGE('',*,*,#12146,.T.);
#16329=ORIENTED_EDGE('',*,*,#12188,.F.);
#16330=ORIENTED_EDGE('',*,*,#12189,.F.);
#16331=ORIENTED_EDGE('',*,*,#12190,.T.);
#16332=ORIENTED_EDGE('',*,*,#12191,.T.);
#16333=ORIENTED_EDGE('',*,*,#12190,.F.);
#16334=ORIENTED_EDGE('',*,*,#12192,.F.);
#16335=ORIENTED_EDGE('',*,*,#12191,.F.);
#16336=ORIENTED_EDGE('',*,*,#12149,.T.);
#16337=ORIENTED_EDGE('',*,*,#12193,.F.);
#16338=ORIENTED_EDGE('',*,*,#12194,.F.);
#16339=ORIENTED_EDGE('',*,*,#12195,.T.);
#16340=ORIENTED_EDGE('',*,*,#12196,.T.);
#16341=ORIENTED_EDGE('',*,*,#12195,.F.);
#16342=ORIENTED_EDGE('',*,*,#12197,.F.);
#16343=ORIENTED_EDGE('',*,*,#12196,.F.);
#16344=ORIENTED_EDGE('',*,*,#12152,.T.);
#16345=ORIENTED_EDGE('',*,*,#12198,.F.);
#16346=ORIENTED_EDGE('',*,*,#12199,.F.);
#16347=ORIENTED_EDGE('',*,*,#12200,.T.);
#16348=ORIENTED_EDGE('',*,*,#12201,.T.);
#16349=ORIENTED_EDGE('',*,*,#12200,.F.);
#16350=ORIENTED_EDGE('',*,*,#12202,.F.);
#16351=ORIENTED_EDGE('',*,*,#12201,.F.);
#16352=ORIENTED_EDGE('',*,*,#12155,.T.);
#16353=ORIENTED_EDGE('',*,*,#12162,.T.);
#16354=ORIENTED_EDGE('',*,*,#12159,.T.);
#16355=ORIENTED_EDGE('',*,*,#12203,.F.);
#16356=ORIENTED_EDGE('',*,*,#12197,.T.);
#16357=ORIENTED_EDGE('',*,*,#12194,.T.);
#16358=ORIENTED_EDGE('',*,*,#12204,.F.);
#16359=ORIENTED_EDGE('',*,*,#12167,.T.);
#16360=ORIENTED_EDGE('',*,*,#12164,.T.);
#16361=ORIENTED_EDGE('',*,*,#12205,.F.);
#16362=ORIENTED_EDGE('',*,*,#12206,.F.);
#16363=ORIENTED_EDGE('',*,*,#12172,.T.);
#16364=ORIENTED_EDGE('',*,*,#12169,.T.);
#16365=ORIENTED_EDGE('',*,*,#12207,.F.);
#16366=ORIENTED_EDGE('',*,*,#12187,.T.);
#16367=ORIENTED_EDGE('',*,*,#12184,.T.);
#16368=ORIENTED_EDGE('',*,*,#12208,.F.);
#16369=ORIENTED_EDGE('',*,*,#12177,.T.);
#16370=ORIENTED_EDGE('',*,*,#12174,.T.);
#16371=ORIENTED_EDGE('',*,*,#12209,.F.);
#16372=ORIENTED_EDGE('',*,*,#12182,.T.);
#16373=ORIENTED_EDGE('',*,*,#12179,.T.);
#16374=ORIENTED_EDGE('',*,*,#12210,.F.);
#16375=ORIENTED_EDGE('',*,*,#12192,.T.);
#16376=ORIENTED_EDGE('',*,*,#12189,.T.);
#16377=ORIENTED_EDGE('',*,*,#12211,.F.);
#16378=ORIENTED_EDGE('',*,*,#12202,.T.);
#16379=ORIENTED_EDGE('',*,*,#12199,.T.);
#16380=ORIENTED_EDGE('',*,*,#12212,.F.);
#16381=ORIENTED_EDGE('',*,*,#12213,.T.);
#16382=ORIENTED_EDGE('',*,*,#12129,.T.);
#16383=ORIENTED_EDGE('',*,*,#12214,.T.);
#16384=ORIENTED_EDGE('',*,*,#12215,.F.);
#16385=ORIENTED_EDGE('',*,*,#12214,.F.);
#16386=ORIENTED_EDGE('',*,*,#12215,.T.);
#16387=ORIENTED_EDGE('',*,*,#12216,.T.);
#16388=ORIENTED_EDGE('',*,*,#12213,.F.);
#16389=ORIENTED_EDGE('',*,*,#12216,.F.);
#16390=ORIENTED_EDGE('',*,*,#12118,.F.);
#16391=ORIENTED_EDGE('',*,*,#12217,.T.);
#16392=ORIENTED_EDGE('',*,*,#12205,.T.);
#16393=ORIENTED_EDGE('',*,*,#12163,.T.);
#16394=ORIENTED_EDGE('',*,*,#12204,.T.);
#16395=ORIENTED_EDGE('',*,*,#12193,.T.);
#16396=ORIENTED_EDGE('',*,*,#12203,.T.);
#16397=ORIENTED_EDGE('',*,*,#12158,.T.);
#16398=ORIENTED_EDGE('',*,*,#12212,.T.);
#16399=ORIENTED_EDGE('',*,*,#12198,.T.);
#16400=ORIENTED_EDGE('',*,*,#12211,.T.);
#16401=ORIENTED_EDGE('',*,*,#12188,.T.);
#16402=ORIENTED_EDGE('',*,*,#12210,.T.);
#16403=ORIENTED_EDGE('',*,*,#12178,.T.);
#16404=ORIENTED_EDGE('',*,*,#12209,.T.);
#16405=ORIENTED_EDGE('',*,*,#12173,.T.);
#16406=ORIENTED_EDGE('',*,*,#12208,.T.);
#16407=ORIENTED_EDGE('',*,*,#12183,.T.);
#16408=ORIENTED_EDGE('',*,*,#12207,.T.);
#16409=ORIENTED_EDGE('',*,*,#12168,.T.);
#16410=ORIENTED_EDGE('',*,*,#12206,.T.);
#16411=ORIENTED_EDGE('',*,*,#12217,.F.);
#16412=ORIENTED_EDGE('',*,*,#12218,.F.);
#16413=ORIENTED_EDGE('',*,*,#12219,.T.);
#16414=ORIENTED_EDGE('',*,*,#12112,.T.);
#16415=ORIENTED_EDGE('',*,*,#12219,.F.);
#16416=ORIENTED_EDGE('',*,*,#12220,.F.);
#16417=ORIENTED_EDGE('',*,*,#12221,.T.);
#16418=ORIENTED_EDGE('',*,*,#12218,.T.);
#16419=ORIENTED_EDGE('',*,*,#12221,.F.);
#16420=ORIENTED_EDGE('',*,*,#12220,.T.);
#16421=ORIENTED_EDGE('',*,*,#12133,.T.);
#16422=ORIENTED_EDGE('',*,*,#12136,.T.);
#16423=ORIENTED_EDGE('',*,*,#12139,.T.);
#16424=ORIENTED_EDGE('',*,*,#12142,.T.);
#16425=ORIENTED_EDGE('',*,*,#12145,.T.);
#16426=ORIENTED_EDGE('',*,*,#12148,.T.);
#16427=ORIENTED_EDGE('',*,*,#12151,.T.);
#16428=ORIENTED_EDGE('',*,*,#12154,.T.);
#16429=ORIENTED_EDGE('',*,*,#12157,.T.);
#16430=ORIENTED_EDGE('',*,*,#12127,.T.);
#16431=ORIENTED_EDGE('',*,*,#12222,.F.);
#16432=ORIENTED_EDGE('',*,*,#12122,.T.);
#16433=ORIENTED_EDGE('',*,*,#12123,.T.);
#16434=ORIENTED_EDGE('',*,*,#12126,.T.);
#16435=ORIENTED_EDGE('',*,*,#12130,.F.);
#16436=ORIENTED_EDGE('',*,*,#12119,.T.);
#16437=ORIENTED_EDGE('',*,*,#12222,.T.);
#16438=ORIENTED_EDGE('',*,*,#12223,.F.);
#16439=ORIENTED_EDGE('',*,*,#12224,.T.);
#16440=ORIENTED_EDGE('',*,*,#12225,.T.);
#16441=ORIENTED_EDGE('',*,*,#12226,.F.);
#16442=ORIENTED_EDGE('',*,*,#12227,.F.);
#16443=ORIENTED_EDGE('',*,*,#12228,.T.);
#16444=ORIENTED_EDGE('',*,*,#12229,.T.);
#16445=ORIENTED_EDGE('',*,*,#12224,.F.);
#16446=ORIENTED_EDGE('',*,*,#12230,.F.);
#16447=ORIENTED_EDGE('',*,*,#12231,.T.);
#16448=ORIENTED_EDGE('',*,*,#12232,.T.);
#16449=ORIENTED_EDGE('',*,*,#12228,.F.);
#16450=ORIENTED_EDGE('',*,*,#12233,.F.);
#16451=ORIENTED_EDGE('',*,*,#12234,.T.);
#16452=ORIENTED_EDGE('',*,*,#12235,.T.);
#16453=ORIENTED_EDGE('',*,*,#12231,.F.);
#16454=ORIENTED_EDGE('',*,*,#12236,.F.);
#16455=ORIENTED_EDGE('',*,*,#12237,.T.);
#16456=ORIENTED_EDGE('',*,*,#12238,.T.);
#16457=ORIENTED_EDGE('',*,*,#12234,.F.);
#16458=ORIENTED_EDGE('',*,*,#12239,.F.);
#16459=ORIENTED_EDGE('',*,*,#12240,.T.);
#16460=ORIENTED_EDGE('',*,*,#12241,.T.);
#16461=ORIENTED_EDGE('',*,*,#12237,.F.);
#16462=ORIENTED_EDGE('',*,*,#12242,.F.);
#16463=ORIENTED_EDGE('',*,*,#12226,.T.);
#16464=ORIENTED_EDGE('',*,*,#12243,.T.);
#16465=ORIENTED_EDGE('',*,*,#12240,.F.);
#16466=ORIENTED_EDGE('',*,*,#12243,.F.);
#16467=ORIENTED_EDGE('',*,*,#12225,.F.);
#16468=ORIENTED_EDGE('',*,*,#12229,.F.);
#16469=ORIENTED_EDGE('',*,*,#12232,.F.);
#16470=ORIENTED_EDGE('',*,*,#12235,.F.);
#16471=ORIENTED_EDGE('',*,*,#12238,.F.);
#16472=ORIENTED_EDGE('',*,*,#12241,.F.);
#16473=ORIENTED_EDGE('',*,*,#12244,.T.);
#16474=ORIENTED_EDGE('',*,*,#12245,.T.);
#16475=ORIENTED_EDGE('',*,*,#12246,.T.);
#16476=ORIENTED_EDGE('',*,*,#12247,.T.);
#16477=ORIENTED_EDGE('',*,*,#12245,.F.);
#16478=ORIENTED_EDGE('',*,*,#12248,.F.);
#16479=ORIENTED_EDGE('',*,*,#12244,.F.);
#16480=ORIENTED_EDGE('',*,*,#12246,.F.);
#16481=ORIENTED_EDGE('',*,*,#12247,.F.);
#16482=ORIENTED_EDGE('',*,*,#12249,.T.);
#16483=ORIENTED_EDGE('',*,*,#12250,.F.);
#16484=ORIENTED_EDGE('',*,*,#12249,.F.);
#16485=ORIENTED_EDGE('',*,*,#12251,.T.);
#16486=ORIENTED_EDGE('',*,*,#12252,.T.);
#16487=ORIENTED_EDGE('',*,*,#12253,.T.);
#16488=ORIENTED_EDGE('',*,*,#12254,.T.);
#16489=ORIENTED_EDGE('',*,*,#12252,.F.);
#16490=ORIENTED_EDGE('',*,*,#12255,.F.);
#16491=ORIENTED_EDGE('',*,*,#12251,.F.);
#16492=ORIENTED_EDGE('',*,*,#12253,.F.);
#16493=ORIENTED_EDGE('',*,*,#12254,.F.);
#16494=ORIENTED_EDGE('',*,*,#12256,.T.);
#16495=ORIENTED_EDGE('',*,*,#12257,.F.);
#16496=ORIENTED_EDGE('',*,*,#12256,.F.);
#16497=ORIENTED_EDGE('',*,*,#12258,.T.);
#16498=ORIENTED_EDGE('',*,*,#12259,.T.);
#16499=ORIENTED_EDGE('',*,*,#12260,.T.);
#16500=ORIENTED_EDGE('',*,*,#12261,.T.);
#16501=ORIENTED_EDGE('',*,*,#12259,.F.);
#16502=ORIENTED_EDGE('',*,*,#12262,.F.);
#16503=ORIENTED_EDGE('',*,*,#12258,.F.);
#16504=ORIENTED_EDGE('',*,*,#12260,.F.);
#16505=ORIENTED_EDGE('',*,*,#12261,.F.);
#16506=ORIENTED_EDGE('',*,*,#12263,.T.);
#16507=ORIENTED_EDGE('',*,*,#12264,.F.);
#16508=ORIENTED_EDGE('',*,*,#12263,.F.);
#16509=ORIENTED_EDGE('',*,*,#12265,.T.);
#16510=ORIENTED_EDGE('',*,*,#12266,.T.);
#16511=ORIENTED_EDGE('',*,*,#12267,.T.);
#16512=ORIENTED_EDGE('',*,*,#12268,.T.);
#16513=ORIENTED_EDGE('',*,*,#12266,.F.);
#16514=ORIENTED_EDGE('',*,*,#12269,.F.);
#16515=ORIENTED_EDGE('',*,*,#12265,.F.);
#16516=ORIENTED_EDGE('',*,*,#12267,.F.);
#16517=ORIENTED_EDGE('',*,*,#12268,.F.);
#16518=ORIENTED_EDGE('',*,*,#12270,.T.);
#16519=ORIENTED_EDGE('',*,*,#12271,.F.);
#16520=ORIENTED_EDGE('',*,*,#12270,.F.);
#16521=ORIENTED_EDGE('',*,*,#12272,.T.);
#16522=ORIENTED_EDGE('',*,*,#12273,.T.);
#16523=ORIENTED_EDGE('',*,*,#12274,.T.);
#16524=ORIENTED_EDGE('',*,*,#12275,.T.);
#16525=ORIENTED_EDGE('',*,*,#12273,.F.);
#16526=ORIENTED_EDGE('',*,*,#12276,.F.);
#16527=ORIENTED_EDGE('',*,*,#12272,.F.);
#16528=ORIENTED_EDGE('',*,*,#12274,.F.);
#16529=ORIENTED_EDGE('',*,*,#12275,.F.);
#16530=ORIENTED_EDGE('',*,*,#12277,.T.);
#16531=ORIENTED_EDGE('',*,*,#12278,.F.);
#16532=ORIENTED_EDGE('',*,*,#12277,.F.);
#16533=ORIENTED_EDGE('',*,*,#12279,.T.);
#16534=ORIENTED_EDGE('',*,*,#12280,.T.);
#16535=ORIENTED_EDGE('',*,*,#12281,.T.);
#16536=ORIENTED_EDGE('',*,*,#12282,.T.);
#16537=ORIENTED_EDGE('',*,*,#12280,.F.);
#16538=ORIENTED_EDGE('',*,*,#12283,.F.);
#16539=ORIENTED_EDGE('',*,*,#12279,.F.);
#16540=ORIENTED_EDGE('',*,*,#12281,.F.);
#16541=ORIENTED_EDGE('',*,*,#12282,.F.);
#16542=ORIENTED_EDGE('',*,*,#12284,.T.);
#16543=ORIENTED_EDGE('',*,*,#12285,.F.);
#16544=ORIENTED_EDGE('',*,*,#12284,.F.);
#16545=ORIENTED_EDGE('',*,*,#12286,.F.);
#16546=ORIENTED_EDGE('',*,*,#12287,.F.);
#16547=ORIENTED_EDGE('',*,*,#12288,.F.);
#16548=ORIENTED_EDGE('',*,*,#12289,.T.);
#16549=ORIENTED_EDGE('',*,*,#12283,.T.);
#16550=ORIENTED_EDGE('',*,*,#12289,.F.);
#16551=ORIENTED_EDGE('',*,*,#12290,.T.);
#16552=ORIENTED_EDGE('',*,*,#12291,.T.);
#16553=ORIENTED_EDGE('',*,*,#12292,.T.);
#16554=ORIENTED_EDGE('',*,*,#12293,.T.);
#16555=ORIENTED_EDGE('',*,*,#12294,.T.);
#16556=ORIENTED_EDGE('',*,*,#12295,.T.);
#16557=ORIENTED_EDGE('',*,*,#12296,.T.);
#16558=ORIENTED_EDGE('',*,*,#12297,.T.);
#16559=ORIENTED_EDGE('',*,*,#12298,.T.);
#16560=ORIENTED_EDGE('',*,*,#12299,.T.);
#16561=ORIENTED_EDGE('',*,*,#12300,.T.);
#16562=ORIENTED_EDGE('',*,*,#12287,.T.);
#16563=ORIENTED_EDGE('',*,*,#12301,.T.);
#16564=ORIENTED_EDGE('',*,*,#12302,.T.);
#16565=ORIENTED_EDGE('',*,*,#12303,.T.);
#16566=ORIENTED_EDGE('',*,*,#12304,.T.);
#16567=ORIENTED_EDGE('',*,*,#12291,.F.);
#16568=ORIENTED_EDGE('',*,*,#12302,.F.);
#16569=ORIENTED_EDGE('',*,*,#12305,.F.);
#16570=ORIENTED_EDGE('',*,*,#12306,.T.);
#16571=ORIENTED_EDGE('',*,*,#12276,.T.);
#16572=ORIENTED_EDGE('',*,*,#12306,.F.);
#16573=ORIENTED_EDGE('',*,*,#12307,.F.);
#16574=ORIENTED_EDGE('',*,*,#12308,.F.);
#16575=ORIENTED_EDGE('',*,*,#12286,.T.);
#16576=ORIENTED_EDGE('',*,*,#12288,.T.);
#16577=ORIENTED_EDGE('',*,*,#12300,.F.);
#16578=ORIENTED_EDGE('',*,*,#12309,.T.);
#16579=ORIENTED_EDGE('',*,*,#12297,.F.);
#16580=ORIENTED_EDGE('',*,*,#12310,.T.);
#16581=ORIENTED_EDGE('',*,*,#12311,.T.);
#16582=ORIENTED_EDGE('',*,*,#12295,.F.);
#16583=ORIENTED_EDGE('',*,*,#12312,.T.);
#16584=ORIENTED_EDGE('',*,*,#12313,.T.);
#16585=ORIENTED_EDGE('',*,*,#12293,.F.);
#16586=ORIENTED_EDGE('',*,*,#12314,.T.);
#16587=ORIENTED_EDGE('',*,*,#12315,.T.);
#16588=ORIENTED_EDGE('',*,*,#12303,.F.);
#16589=ORIENTED_EDGE('',*,*,#12307,.T.);
#16590=ORIENTED_EDGE('',*,*,#12305,.T.);
#16591=ORIENTED_EDGE('',*,*,#12301,.F.);
#16592=ORIENTED_EDGE('',*,*,#12314,.F.);
#16593=ORIENTED_EDGE('',*,*,#12292,.F.);
#16594=ORIENTED_EDGE('',*,*,#12304,.F.);
#16595=ORIENTED_EDGE('',*,*,#12315,.F.);
#16596=ORIENTED_EDGE('',*,*,#12316,.T.);
#16597=ORIENTED_EDGE('',*,*,#12269,.T.);
#16598=ORIENTED_EDGE('',*,*,#12316,.F.);
#16599=ORIENTED_EDGE('',*,*,#12294,.F.);
#16600=ORIENTED_EDGE('',*,*,#12313,.F.);
#16601=ORIENTED_EDGE('',*,*,#12317,.T.);
#16602=ORIENTED_EDGE('',*,*,#12262,.T.);
#16603=ORIENTED_EDGE('',*,*,#12317,.F.);
#16604=ORIENTED_EDGE('',*,*,#12312,.F.);
#16605=ORIENTED_EDGE('',*,*,#12310,.F.);
#16606=ORIENTED_EDGE('',*,*,#12296,.F.);
#16607=ORIENTED_EDGE('',*,*,#12311,.F.);
#16608=ORIENTED_EDGE('',*,*,#12318,.T.);
#16609=ORIENTED_EDGE('',*,*,#12255,.T.);
#16610=ORIENTED_EDGE('',*,*,#12318,.F.);
#16611=ORIENTED_EDGE('',*,*,#12298,.F.);
#16612=ORIENTED_EDGE('',*,*,#12309,.F.);
#16613=ORIENTED_EDGE('',*,*,#12299,.F.);
#16614=ORIENTED_EDGE('',*,*,#12319,.T.);
#16615=ORIENTED_EDGE('',*,*,#12248,.T.);
#16616=ORIENTED_EDGE('',*,*,#12319,.F.);
#16617=ORIENTED_EDGE('',*,*,#12320,.T.);
#16618=ORIENTED_EDGE('',*,*,#12321,.T.);
#16619=ORIENTED_EDGE('',*,*,#12322,.T.);
#16620=ORIENTED_EDGE('',*,*,#12321,.F.);
#16621=ORIENTED_EDGE('',*,*,#12322,.F.);
#16622=ORIENTED_EDGE('',*,*,#12323,.T.);
#16623=ORIENTED_EDGE('',*,*,#12324,.F.);
#16624=ORIENTED_EDGE('',*,*,#12325,.F.);
#16625=ORIENTED_EDGE('',*,*,#12323,.F.);
#16626=ORIENTED_EDGE('',*,*,#12326,.F.);
#16627=ORIENTED_EDGE('',*,*,#12320,.F.);
#16628=ORIENTED_EDGE('',*,*,#12326,.T.);
#16629=ORIENTED_EDGE('',*,*,#12327,.T.);
#16630=ORIENTED_EDGE('',*,*,#12328,.T.);
#16631=ORIENTED_EDGE('',*,*,#12327,.F.);
#16632=ORIENTED_EDGE('',*,*,#12328,.F.);
#16633=ORIENTED_EDGE('',*,*,#12329,.T.);
#16634=ORIENTED_EDGE('',*,*,#12330,.F.);
#16635=ORIENTED_EDGE('',*,*,#12331,.F.);
#16636=ORIENTED_EDGE('',*,*,#12329,.F.);
#16637=ORIENTED_EDGE('',*,*,#12332,.T.);
#16638=ORIENTED_EDGE('',*,*,#12333,.T.);
#16639=ORIENTED_EDGE('',*,*,#12334,.T.);
#16640=ORIENTED_EDGE('',*,*,#12335,.T.);
#16641=ORIENTED_EDGE('',*,*,#12334,.F.);
#16642=ORIENTED_EDGE('',*,*,#12336,.T.);
#16643=ORIENTED_EDGE('',*,*,#12285,.T.);
#16644=ORIENTED_EDGE('',*,*,#12278,.T.);
#16645=ORIENTED_EDGE('',*,*,#12271,.T.);
#16646=ORIENTED_EDGE('',*,*,#12264,.T.);
#16647=ORIENTED_EDGE('',*,*,#12257,.T.);
#16648=ORIENTED_EDGE('',*,*,#12250,.T.);
#16649=ORIENTED_EDGE('',*,*,#12335,.F.);
#16650=ORIENTED_EDGE('',*,*,#12332,.F.);
#16651=ORIENTED_EDGE('',*,*,#12333,.F.);
#16652=ORIENTED_EDGE('',*,*,#12337,.T.);
#16653=ORIENTED_EDGE('',*,*,#12338,.F.);
#16654=ORIENTED_EDGE('',*,*,#12337,.F.);
#16655=ORIENTED_EDGE('',*,*,#12324,.T.);
#16656=ORIENTED_EDGE('',*,*,#12325,.T.);
#16657=ORIENTED_EDGE('',*,*,#12339,.T.);
#16658=ORIENTED_EDGE('',*,*,#12340,.T.);
#16659=ORIENTED_EDGE('',*,*,#12341,.T.);
#16660=ORIENTED_EDGE('',*,*,#12342,.T.);
#16661=ORIENTED_EDGE('',*,*,#12340,.F.);
#16662=ORIENTED_EDGE('',*,*,#12343,.T.);
#16663=ORIENTED_EDGE('',*,*,#12344,.T.);
#16664=ORIENTED_EDGE('',*,*,#12341,.F.);
#16665=ORIENTED_EDGE('',*,*,#12342,.F.);
#16666=ORIENTED_EDGE('',*,*,#12344,.F.);
#16667=ORIENTED_EDGE('',*,*,#12345,.F.);
#16668=ORIENTED_EDGE('',*,*,#12223,.T.);
#16669=ORIENTED_EDGE('',*,*,#12242,.T.);
#16670=ORIENTED_EDGE('',*,*,#12239,.T.);
#16671=ORIENTED_EDGE('',*,*,#12236,.T.);
#16672=ORIENTED_EDGE('',*,*,#12233,.T.);
#16673=ORIENTED_EDGE('',*,*,#12230,.T.);
#16674=ORIENTED_EDGE('',*,*,#12227,.T.);
#16675=ORIENTED_EDGE('',*,*,#12339,.F.);
#16676=ORIENTED_EDGE('',*,*,#12346,.T.);
#16677=ORIENTED_EDGE('',*,*,#12347,.T.);
#16678=ORIENTED_EDGE('',*,*,#12348,.T.);
#16679=ORIENTED_EDGE('',*,*,#12347,.F.);
#16680=ORIENTED_EDGE('',*,*,#12290,.F.);
#16681=ORIENTED_EDGE('',*,*,#12349,.T.);
#16682=ORIENTED_EDGE('',*,*,#12346,.F.);
#16683=ORIENTED_EDGE('',*,*,#12349,.F.);
#16684=ORIENTED_EDGE('',*,*,#12330,.T.);
#16685=ORIENTED_EDGE('',*,*,#12331,.T.);
#16686=ORIENTED_EDGE('',*,*,#12348,.F.);
#16687=ORIENTED_EDGE('',*,*,#12350,.T.);
#16688=ORIENTED_EDGE('',*,*,#12351,.T.);
#16689=ORIENTED_EDGE('',*,*,#12350,.F.);
#16690=ORIENTED_EDGE('',*,*,#12352,.F.);
#16691=ORIENTED_EDGE('',*,*,#12353,.T.);
#16692=ORIENTED_EDGE('',*,*,#12345,.T.);
#16693=ORIENTED_EDGE('',*,*,#12353,.F.);
#16694=ORIENTED_EDGE('',*,*,#12351,.F.);
#16695=ORIENTED_EDGE('',*,*,#12354,.T.);
#16696=ORIENTED_EDGE('',*,*,#12352,.T.);
#16697=ORIENTED_EDGE('',*,*,#12354,.F.);
#16698=ORIENTED_EDGE('',*,*,#12355,.F.);
#16699=ORIENTED_EDGE('',*,*,#12356,.T.);
#16700=ORIENTED_EDGE('',*,*,#12308,.T.);
#16701=ORIENTED_EDGE('',*,*,#12356,.F.);
#16702=ORIENTED_EDGE('',*,*,#12357,.F.);
#16703=ORIENTED_EDGE('',*,*,#12358,.T.);
#16704=ORIENTED_EDGE('',*,*,#12355,.T.);
#16705=ORIENTED_EDGE('',*,*,#12358,.F.);
#16706=ORIENTED_EDGE('',*,*,#12336,.F.);
#16707=ORIENTED_EDGE('',*,*,#12359,.T.);
#16708=ORIENTED_EDGE('',*,*,#12357,.T.);
#16709=ORIENTED_EDGE('',*,*,#12359,.F.);
#16710=ORIENTED_EDGE('',*,*,#12338,.T.);
#16711=ORIENTED_EDGE('',*,*,#12360,.F.);
#16712=ORIENTED_EDGE('',*,*,#12360,.T.);
#16713=ORIENTED_EDGE('',*,*,#12361,.T.);
#16714=ORIENTED_EDGE('',*,*,#12362,.F.);
#16715=ORIENTED_EDGE('',*,*,#12361,.F.);
#16716=ORIENTED_EDGE('',*,*,#12362,.T.);
#16717=ORIENTED_EDGE('',*,*,#12363,.F.);
#16718=ORIENTED_EDGE('',*,*,#12363,.T.);
#16719=ORIENTED_EDGE('',*,*,#12364,.T.);
#16720=ORIENTED_EDGE('',*,*,#12365,.F.);
#16721=ORIENTED_EDGE('',*,*,#12364,.F.);
#16722=ORIENTED_EDGE('',*,*,#12366,.F.);
#16723=ORIENTED_EDGE('',*,*,#12365,.T.);
#16724=ORIENTED_EDGE('',*,*,#12366,.T.);
#16725=ORIENTED_EDGE('',*,*,#12367,.T.);
#16726=ORIENTED_EDGE('',*,*,#12368,.F.);
#16727=ORIENTED_EDGE('',*,*,#12367,.F.);
#16728=ORIENTED_EDGE('',*,*,#12368,.T.);
#16729=ORIENTED_EDGE('',*,*,#12369,.F.);
#16730=ORIENTED_EDGE('',*,*,#12369,.T.);
#16731=ORIENTED_EDGE('',*,*,#12370,.T.);
#16732=ORIENTED_EDGE('',*,*,#12371,.F.);
#16733=ORIENTED_EDGE('',*,*,#12370,.F.);
#16734=ORIENTED_EDGE('',*,*,#12371,.T.);
#16735=ORIENTED_EDGE('',*,*,#12343,.F.);
#16736=ORIENTED_EDGE('',*,*,#12372,.T.);
#16737=ORIENTED_EDGE('',*,*,#12373,.T.);
#16738=ORIENTED_EDGE('',*,*,#12374,.T.);
#16739=ORIENTED_EDGE('',*,*,#12373,.F.);
#16740=ORIENTED_EDGE('',*,*,#12375,.F.);
#16741=ORIENTED_EDGE('',*,*,#12376,.T.);
#16742=ORIENTED_EDGE('',*,*,#12374,.F.);
#16743=ORIENTED_EDGE('',*,*,#12376,.F.);
#16744=ORIENTED_EDGE('',*,*,#12377,.T.);
#16745=ORIENTED_EDGE('',*,*,#12378,.T.);
#16746=ORIENTED_EDGE('',*,*,#12379,.T.);
#16747=ORIENTED_EDGE('',*,*,#12380,.T.);
#16748=ORIENTED_EDGE('',*,*,#12381,.F.);
#16749=ORIENTED_EDGE('',*,*,#12382,.F.);
#16750=ORIENTED_EDGE('',*,*,#12383,.F.);
#16751=ORIENTED_EDGE('',*,*,#12384,.F.);
#16752=ORIENTED_EDGE('',*,*,#12385,.T.);
#16753=ORIENTED_EDGE('',*,*,#12386,.F.);
#16754=ORIENTED_EDGE('',*,*,#12387,.F.);
#16755=ORIENTED_EDGE('',*,*,#12372,.F.);
#16756=ORIENTED_EDGE('',*,*,#12388,.T.);
#16757=ORIENTED_EDGE('',*,*,#12389,.T.);
#16758=ORIENTED_EDGE('',*,*,#12375,.T.);
#16759=ORIENTED_EDGE('',*,*,#12389,.F.);
#16760=ORIENTED_EDGE('',*,*,#12390,.T.);
#16761=ORIENTED_EDGE('',*,*,#12391,.F.);
#16762=ORIENTED_EDGE('',*,*,#12392,.T.);
#16763=ORIENTED_EDGE('',*,*,#12393,.F.);
#16764=ORIENTED_EDGE('',*,*,#12394,.F.);
#16765=ORIENTED_EDGE('',*,*,#12395,.F.);
#16766=ORIENTED_EDGE('',*,*,#12396,.F.);
#16767=ORIENTED_EDGE('',*,*,#12397,.T.);
#16768=ORIENTED_EDGE('',*,*,#12398,.T.);
#16769=ORIENTED_EDGE('',*,*,#12399,.T.);
#16770=ORIENTED_EDGE('',*,*,#12400,.T.);
#16771=ORIENTED_EDGE('',*,*,#12401,.T.);
#16772=ORIENTED_EDGE('',*,*,#12402,.T.);
#16773=ORIENTED_EDGE('',*,*,#12403,.T.);
#16774=ORIENTED_EDGE('',*,*,#12404,.T.);
#16775=ORIENTED_EDGE('',*,*,#12405,.F.);
#16776=ORIENTED_EDGE('',*,*,#12406,.F.);
#16777=ORIENTED_EDGE('',*,*,#12407,.F.);
#16778=ORIENTED_EDGE('',*,*,#12388,.F.);
#16779=ORIENTED_EDGE('',*,*,#12381,.T.);
#16780=ORIENTED_EDGE('',*,*,#12408,.T.);
#16781=ORIENTED_EDGE('',*,*,#12409,.T.);
#16782=ORIENTED_EDGE('',*,*,#12408,.F.);
#16783=ORIENTED_EDGE('',*,*,#12410,.F.);
#16784=ORIENTED_EDGE('',*,*,#12411,.T.);
#16785=ORIENTED_EDGE('',*,*,#12409,.F.);
#16786=ORIENTED_EDGE('',*,*,#12411,.F.);
#16787=ORIENTED_EDGE('',*,*,#12394,.T.);
#16788=ORIENTED_EDGE('',*,*,#12412,.T.);
#16789=ORIENTED_EDGE('',*,*,#12410,.T.);
#16790=ORIENTED_EDGE('',*,*,#12412,.F.);
#16791=ORIENTED_EDGE('',*,*,#12387,.T.);
#16792=ORIENTED_EDGE('',*,*,#12413,.T.);
#16793=ORIENTED_EDGE('',*,*,#12414,.T.);
#16794=ORIENTED_EDGE('',*,*,#12413,.F.);
#16795=ORIENTED_EDGE('',*,*,#12415,.F.);
#16796=ORIENTED_EDGE('',*,*,#12416,.T.);
#16797=ORIENTED_EDGE('',*,*,#12414,.F.);
#16798=ORIENTED_EDGE('',*,*,#12416,.F.);
#16799=ORIENTED_EDGE('',*,*,#12407,.T.);
#16800=ORIENTED_EDGE('',*,*,#12417,.T.);
#16801=ORIENTED_EDGE('',*,*,#12415,.T.);
#16802=ORIENTED_EDGE('',*,*,#12417,.F.);
#16803=ORIENTED_EDGE('',*,*,#12382,.T.);
#16804=ORIENTED_EDGE('',*,*,#12418,.T.);
#16805=ORIENTED_EDGE('',*,*,#12419,.T.);
#16806=ORIENTED_EDGE('',*,*,#12418,.F.);
#16807=ORIENTED_EDGE('',*,*,#12420,.F.);
#16808=ORIENTED_EDGE('',*,*,#12421,.T.);
#16809=ORIENTED_EDGE('',*,*,#12419,.F.);
#16810=ORIENTED_EDGE('',*,*,#12421,.F.);
#16811=ORIENTED_EDGE('',*,*,#12395,.T.);
#16812=ORIENTED_EDGE('',*,*,#12422,.T.);
#16813=ORIENTED_EDGE('',*,*,#12420,.T.);
#16814=ORIENTED_EDGE('',*,*,#12422,.F.);
#16815=ORIENTED_EDGE('',*,*,#12386,.T.);
#16816=ORIENTED_EDGE('',*,*,#12423,.T.);
#16817=ORIENTED_EDGE('',*,*,#12424,.T.);
#16818=ORIENTED_EDGE('',*,*,#12423,.F.);
#16819=ORIENTED_EDGE('',*,*,#12425,.F.);
#16820=ORIENTED_EDGE('',*,*,#12426,.T.);
#16821=ORIENTED_EDGE('',*,*,#12424,.F.);
#16822=ORIENTED_EDGE('',*,*,#12426,.F.);
#16823=ORIENTED_EDGE('',*,*,#12406,.T.);
#16824=ORIENTED_EDGE('',*,*,#12427,.T.);
#16825=ORIENTED_EDGE('',*,*,#12425,.T.);
#16826=ORIENTED_EDGE('',*,*,#12427,.F.);
#16827=ORIENTED_EDGE('',*,*,#12383,.T.);
#16828=ORIENTED_EDGE('',*,*,#12428,.T.);
#16829=ORIENTED_EDGE('',*,*,#12429,.T.);
#16830=ORIENTED_EDGE('',*,*,#12428,.F.);
#16831=ORIENTED_EDGE('',*,*,#12430,.F.);
#16832=ORIENTED_EDGE('',*,*,#12431,.T.);
#16833=ORIENTED_EDGE('',*,*,#12429,.F.);
#16834=ORIENTED_EDGE('',*,*,#12431,.F.);
#16835=ORIENTED_EDGE('',*,*,#12396,.T.);
#16836=ORIENTED_EDGE('',*,*,#12432,.T.);
#16837=ORIENTED_EDGE('',*,*,#12430,.T.);
#16838=ORIENTED_EDGE('',*,*,#12432,.F.);
#16839=ORIENTED_EDGE('',*,*,#12433,.F.);
#16840=ORIENTED_EDGE('',*,*,#12434,.F.);
#16841=ORIENTED_EDGE('',*,*,#12435,.T.);
#16842=ORIENTED_EDGE('',*,*,#12385,.F.);
#16843=ORIENTED_EDGE('',*,*,#12435,.F.);
#16844=ORIENTED_EDGE('',*,*,#12436,.T.);
#16845=ORIENTED_EDGE('',*,*,#12437,.T.);
#16846=ORIENTED_EDGE('',*,*,#12438,.T.);
#16847=ORIENTED_EDGE('',*,*,#12437,.F.);
#16848=ORIENTED_EDGE('',*,*,#12439,.F.);
#16849=ORIENTED_EDGE('',*,*,#12440,.T.);
#16850=ORIENTED_EDGE('',*,*,#12438,.F.);
#16851=ORIENTED_EDGE('',*,*,#12440,.F.);
#16852=ORIENTED_EDGE('',*,*,#12379,.F.);
#16853=ORIENTED_EDGE('',*,*,#12441,.F.);
#16854=ORIENTED_EDGE('',*,*,#12442,.F.);
#16855=ORIENTED_EDGE('',*,*,#12443,.F.);
#16856=ORIENTED_EDGE('',*,*,#12392,.F.);
#16857=ORIENTED_EDGE('',*,*,#12444,.F.);
#16858=ORIENTED_EDGE('',*,*,#12445,.F.);
#16859=ORIENTED_EDGE('',*,*,#12446,.F.);
#16860=ORIENTED_EDGE('',*,*,#12436,.F.);
#16861=ORIENTED_EDGE('',*,*,#12447,.T.);
#16862=ORIENTED_EDGE('',*,*,#12448,.T.);
#16863=ORIENTED_EDGE('',*,*,#12449,.T.);
#16864=ORIENTED_EDGE('',*,*,#12448,.F.);
#16865=ORIENTED_EDGE('',*,*,#12449,.F.);
#16866=ORIENTED_EDGE('',*,*,#12450,.T.);
#16867=ORIENTED_EDGE('',*,*,#12451,.T.);
#16868=ORIENTED_EDGE('',*,*,#12450,.F.);
#16869=ORIENTED_EDGE('',*,*,#12377,.F.);
#16870=ORIENTED_EDGE('',*,*,#12452,.F.);
#16871=ORIENTED_EDGE('',*,*,#12453,.F.);
#16872=ORIENTED_EDGE('',*,*,#12454,.F.);
#16873=ORIENTED_EDGE('',*,*,#12390,.F.);
#16874=ORIENTED_EDGE('',*,*,#12455,.F.);
#16875=ORIENTED_EDGE('',*,*,#12456,.F.);
#16876=ORIENTED_EDGE('',*,*,#12457,.F.);
#16877=ORIENTED_EDGE('',*,*,#12447,.F.);
#16878=ORIENTED_EDGE('',*,*,#12458,.F.);
#16879=ORIENTED_EDGE('',*,*,#12459,.T.);
#16880=ORIENTED_EDGE('',*,*,#12460,.F.);
#16881=ORIENTED_EDGE('',*,*,#12461,.F.);
#16882=ORIENTED_EDGE('',*,*,#12462,.T.);
#16883=ORIENTED_EDGE('',*,*,#12463,.F.);
#16884=ORIENTED_EDGE('',*,*,#12464,.F.);
#16885=ORIENTED_EDGE('',*,*,#12459,.F.);
#16886=ORIENTED_EDGE('',*,*,#12465,.F.);
#16887=ORIENTED_EDGE('',*,*,#12466,.T.);
#16888=ORIENTED_EDGE('',*,*,#12467,.T.);
#16889=ORIENTED_EDGE('',*,*,#12451,.F.);
#16890=ORIENTED_EDGE('',*,*,#12458,.T.);
#16891=ORIENTED_EDGE('',*,*,#12468,.F.);
#16892=ORIENTED_EDGE('',*,*,#12469,.F.);
#16893=ORIENTED_EDGE('',*,*,#12462,.F.);
#16894=ORIENTED_EDGE('',*,*,#12470,.F.);
#16895=ORIENTED_EDGE('',*,*,#12471,.F.);
#16896=ORIENTED_EDGE('',*,*,#12467,.F.);
#16897=ORIENTED_EDGE('',*,*,#12472,.T.);
#16898=ORIENTED_EDGE('',*,*,#12472,.F.);
#16899=ORIENTED_EDGE('',*,*,#12466,.F.);
#16900=ORIENTED_EDGE('',*,*,#12468,.T.);
#16901=ORIENTED_EDGE('',*,*,#12465,.T.);
#16902=ORIENTED_EDGE('',*,*,#12471,.T.);
#16903=ORIENTED_EDGE('',*,*,#12473,.T.);
#16904=ORIENTED_EDGE('',*,*,#12474,.F.);
#16905=ORIENTED_EDGE('',*,*,#12401,.F.);
#16906=ORIENTED_EDGE('',*,*,#12475,.T.);
#16907=ORIENTED_EDGE('',*,*,#12476,.T.);
#16908=ORIENTED_EDGE('',*,*,#12470,.T.);
#16909=ORIENTED_EDGE('',*,*,#12461,.T.);
#16910=ORIENTED_EDGE('',*,*,#12477,.F.);
#16911=ORIENTED_EDGE('',*,*,#12478,.F.);
#16912=ORIENTED_EDGE('',*,*,#12473,.F.);
#16913=ORIENTED_EDGE('',*,*,#12454,.T.);
#16914=ORIENTED_EDGE('',*,*,#12479,.F.);
#16915=ORIENTED_EDGE('',*,*,#12444,.T.);
#16916=ORIENTED_EDGE('',*,*,#12391,.T.);
#16917=ORIENTED_EDGE('',*,*,#12453,.T.);
#16918=ORIENTED_EDGE('',*,*,#12480,.F.);
#16919=ORIENTED_EDGE('',*,*,#12445,.T.);
#16920=ORIENTED_EDGE('',*,*,#12479,.T.);
#16921=ORIENTED_EDGE('',*,*,#12452,.T.);
#16922=ORIENTED_EDGE('',*,*,#12380,.F.);
#16923=ORIENTED_EDGE('',*,*,#12446,.T.);
#16924=ORIENTED_EDGE('',*,*,#12480,.T.);
#16925=ORIENTED_EDGE('',*,*,#12481,.F.);
#16926=ORIENTED_EDGE('',*,*,#12482,.F.);
#16927=ORIENTED_EDGE('',*,*,#12483,.T.);
#16928=ORIENTED_EDGE('',*,*,#12484,.T.);
#16929=ORIENTED_EDGE('',*,*,#12483,.F.);
#16930=ORIENTED_EDGE('',*,*,#12485,.F.);
#16931=ORIENTED_EDGE('',*,*,#12486,.F.);
#16932=ORIENTED_EDGE('',*,*,#12487,.F.);
#16933=ORIENTED_EDGE('',*,*,#12433,.T.);
#16934=ORIENTED_EDGE('',*,*,#12434,.T.);
#16935=ORIENTED_EDGE('',*,*,#12488,.F.);
#16936=ORIENTED_EDGE('',*,*,#12489,.F.);
#16937=ORIENTED_EDGE('',*,*,#12490,.F.);
#16938=ORIENTED_EDGE('',*,*,#12491,.T.);
#16939=ORIENTED_EDGE('',*,*,#12489,.T.);
#16940=ORIENTED_EDGE('',*,*,#12492,.F.);
#16941=ORIENTED_EDGE('',*,*,#12493,.F.);
#16942=ORIENTED_EDGE('',*,*,#12487,.T.);
#16943=ORIENTED_EDGE('',*,*,#12494,.F.);
#16944=ORIENTED_EDGE('',*,*,#12495,.F.);
#16945=ORIENTED_EDGE('',*,*,#12490,.T.);
#16946=ORIENTED_EDGE('',*,*,#12491,.F.);
#16947=ORIENTED_EDGE('',*,*,#12439,.T.);
#16948=ORIENTED_EDGE('',*,*,#12484,.F.);
#16949=ORIENTED_EDGE('',*,*,#12492,.T.);
#16950=ORIENTED_EDGE('',*,*,#12488,.T.);
#16951=ORIENTED_EDGE('',*,*,#12495,.T.);
#16952=ORIENTED_EDGE('',*,*,#12496,.T.);
#16953=ORIENTED_EDGE('',*,*,#12497,.F.);
#16954=ORIENTED_EDGE('',*,*,#12397,.F.);
#16955=ORIENTED_EDGE('',*,*,#12498,.T.);
#16956=ORIENTED_EDGE('',*,*,#12499,.T.);
#16957=ORIENTED_EDGE('',*,*,#12494,.T.);
#16958=ORIENTED_EDGE('',*,*,#12486,.T.);
#16959=ORIENTED_EDGE('',*,*,#12500,.F.);
#16960=ORIENTED_EDGE('',*,*,#12501,.F.);
#16961=ORIENTED_EDGE('',*,*,#12496,.F.);
#16962=ORIENTED_EDGE('',*,*,#12400,.F.);
#16963=ORIENTED_EDGE('',*,*,#12502,.T.);
#16964=ORIENTED_EDGE('',*,*,#12503,.T.);
#16965=ORIENTED_EDGE('',*,*,#12498,.F.);
#16966=ORIENTED_EDGE('',*,*,#12485,.T.);
#16967=ORIENTED_EDGE('',*,*,#12482,.T.);
#16968=ORIENTED_EDGE('',*,*,#12504,.T.);
#16969=ORIENTED_EDGE('',*,*,#12502,.F.);
#16970=ORIENTED_EDGE('',*,*,#12399,.F.);
#16971=ORIENTED_EDGE('',*,*,#12505,.T.);
#16972=ORIENTED_EDGE('',*,*,#12500,.T.);
#16973=ORIENTED_EDGE('',*,*,#12398,.F.);
#16974=ORIENTED_EDGE('',*,*,#12497,.T.);
#16975=ORIENTED_EDGE('',*,*,#12501,.T.);
#16976=ORIENTED_EDGE('',*,*,#12505,.F.);
#16977=ORIENTED_EDGE('',*,*,#12493,.T.);
#16978=ORIENTED_EDGE('',*,*,#12499,.F.);
#16979=ORIENTED_EDGE('',*,*,#12503,.F.);
#16980=ORIENTED_EDGE('',*,*,#12504,.F.);
#16981=ORIENTED_EDGE('',*,*,#12481,.T.);
#16982=ORIENTED_EDGE('',*,*,#12404,.F.);
#16983=ORIENTED_EDGE('',*,*,#12506,.T.);
#16984=ORIENTED_EDGE('',*,*,#12507,.T.);
#16985=ORIENTED_EDGE('',*,*,#12475,.F.);
#16986=ORIENTED_EDGE('',*,*,#12460,.T.);
#16987=ORIENTED_EDGE('',*,*,#12464,.T.);
#16988=ORIENTED_EDGE('',*,*,#12508,.T.);
#16989=ORIENTED_EDGE('',*,*,#12506,.F.);
#16990=ORIENTED_EDGE('',*,*,#12403,.F.);
#16991=ORIENTED_EDGE('',*,*,#12509,.T.);
#16992=ORIENTED_EDGE('',*,*,#12477,.T.);
#16993=ORIENTED_EDGE('',*,*,#12402,.F.);
#16994=ORIENTED_EDGE('',*,*,#12474,.T.);
#16995=ORIENTED_EDGE('',*,*,#12478,.T.);
#16996=ORIENTED_EDGE('',*,*,#12509,.F.);
#16997=ORIENTED_EDGE('',*,*,#12469,.T.);
#16998=ORIENTED_EDGE('',*,*,#12476,.F.);
#16999=ORIENTED_EDGE('',*,*,#12507,.F.);
#17000=ORIENTED_EDGE('',*,*,#12508,.F.);
#17001=ORIENTED_EDGE('',*,*,#12463,.T.);
#17002=ORIENTED_EDGE('',*,*,#12405,.T.);
#17003=ORIENTED_EDGE('',*,*,#12510,.T.);
#17004=ORIENTED_EDGE('',*,*,#12511,.T.);
#17005=ORIENTED_EDGE('',*,*,#12512,.T.);
#17006=ORIENTED_EDGE('',*,*,#12510,.F.);
#17007=ORIENTED_EDGE('',*,*,#12513,.F.);
#17008=ORIENTED_EDGE('',*,*,#12514,.F.);
#17009=ORIENTED_EDGE('',*,*,#12515,.T.);
#17010=ORIENTED_EDGE('',*,*,#12511,.F.);
#17011=ORIENTED_EDGE('',*,*,#12512,.F.);
#17012=ORIENTED_EDGE('',*,*,#12515,.F.);
#17013=ORIENTED_EDGE('',*,*,#12513,.T.);
#17014=ORIENTED_EDGE('',*,*,#12514,.T.);
#17015=ORIENTED_EDGE('',*,*,#12516,.T.);
#17016=ORIENTED_EDGE('',*,*,#12384,.T.);
#17017=ORIENTED_EDGE('',*,*,#12516,.F.);
#17018=ORIENTED_EDGE('',*,*,#12455,.T.);
#17019=ORIENTED_EDGE('',*,*,#12393,.T.);
#17020=ORIENTED_EDGE('',*,*,#12443,.T.);
#17021=ORIENTED_EDGE('',*,*,#12517,.F.);
#17022=ORIENTED_EDGE('',*,*,#12456,.T.);
#17023=ORIENTED_EDGE('',*,*,#12517,.T.);
#17024=ORIENTED_EDGE('',*,*,#12442,.T.);
#17025=ORIENTED_EDGE('',*,*,#12518,.F.);
#17026=ORIENTED_EDGE('',*,*,#12457,.T.);
#17027=ORIENTED_EDGE('',*,*,#12518,.T.);
#17028=ORIENTED_EDGE('',*,*,#12441,.T.);
#17029=ORIENTED_EDGE('',*,*,#12378,.F.);
#17030=ORIENTED_EDGE('',*,*,#12519,.F.);
#17031=ORIENTED_EDGE('',*,*,#12520,.T.);
#17032=ORIENTED_EDGE('',*,*,#12521,.T.);
#17033=ORIENTED_EDGE('',*,*,#12522,.F.);
#17034=ORIENTED_EDGE('',*,*,#12523,.F.);
#17035=ORIENTED_EDGE('',*,*,#12524,.T.);
#17036=ORIENTED_EDGE('',*,*,#12525,.T.);
#17037=ORIENTED_EDGE('',*,*,#12520,.F.);
#17038=ORIENTED_EDGE('',*,*,#12526,.F.);
#17039=ORIENTED_EDGE('',*,*,#12527,.T.);
#17040=ORIENTED_EDGE('',*,*,#12528,.T.);
#17041=ORIENTED_EDGE('',*,*,#12524,.F.);
#17042=ORIENTED_EDGE('',*,*,#12529,.F.);
#17043=ORIENTED_EDGE('',*,*,#12530,.T.);
#17044=ORIENTED_EDGE('',*,*,#12531,.T.);
#17045=ORIENTED_EDGE('',*,*,#12527,.F.);
#17046=ORIENTED_EDGE('',*,*,#12532,.F.);
#17047=ORIENTED_EDGE('',*,*,#12533,.T.);
#17048=ORIENTED_EDGE('',*,*,#12534,.T.);
#17049=ORIENTED_EDGE('',*,*,#12530,.F.);
#17050=ORIENTED_EDGE('',*,*,#12535,.F.);
#17051=ORIENTED_EDGE('',*,*,#12536,.T.);
#17052=ORIENTED_EDGE('',*,*,#12537,.T.);
#17053=ORIENTED_EDGE('',*,*,#12533,.F.);
#17054=ORIENTED_EDGE('',*,*,#12538,.F.);
#17055=ORIENTED_EDGE('',*,*,#12539,.T.);
#17056=ORIENTED_EDGE('',*,*,#12540,.T.);
#17057=ORIENTED_EDGE('',*,*,#12536,.F.);
#17058=ORIENTED_EDGE('',*,*,#12541,.F.);
#17059=ORIENTED_EDGE('',*,*,#12542,.T.);
#17060=ORIENTED_EDGE('',*,*,#12543,.T.);
#17061=ORIENTED_EDGE('',*,*,#12539,.F.);
#17062=ORIENTED_EDGE('',*,*,#12544,.F.);
#17063=ORIENTED_EDGE('',*,*,#12545,.T.);
#17064=ORIENTED_EDGE('',*,*,#12546,.T.);
#17065=ORIENTED_EDGE('',*,*,#12542,.F.);
#17066=ORIENTED_EDGE('',*,*,#12547,.F.);
#17067=ORIENTED_EDGE('',*,*,#12522,.T.);
#17068=ORIENTED_EDGE('',*,*,#12548,.T.);
#17069=ORIENTED_EDGE('',*,*,#12545,.F.);
#17070=ORIENTED_EDGE('',*,*,#12549,.F.);
#17071=ORIENTED_EDGE('',*,*,#12550,.T.);
#17072=ORIENTED_EDGE('',*,*,#12551,.T.);
#17073=ORIENTED_EDGE('',*,*,#12552,.F.);
#17074=ORIENTED_EDGE('',*,*,#12553,.F.);
#17075=ORIENTED_EDGE('',*,*,#12554,.T.);
#17076=ORIENTED_EDGE('',*,*,#12555,.T.);
#17077=ORIENTED_EDGE('',*,*,#12550,.F.);
#17078=ORIENTED_EDGE('',*,*,#12556,.F.);
#17079=ORIENTED_EDGE('',*,*,#12557,.T.);
#17080=ORIENTED_EDGE('',*,*,#12558,.T.);
#17081=ORIENTED_EDGE('',*,*,#12554,.F.);
#17082=ORIENTED_EDGE('',*,*,#12559,.F.);
#17083=ORIENTED_EDGE('',*,*,#12560,.T.);
#17084=ORIENTED_EDGE('',*,*,#12561,.T.);
#17085=ORIENTED_EDGE('',*,*,#12557,.F.);
#17086=ORIENTED_EDGE('',*,*,#12562,.F.);
#17087=ORIENTED_EDGE('',*,*,#12563,.T.);
#17088=ORIENTED_EDGE('',*,*,#12564,.T.);
#17089=ORIENTED_EDGE('',*,*,#12560,.F.);
#17090=ORIENTED_EDGE('',*,*,#12565,.F.);
#17091=ORIENTED_EDGE('',*,*,#12566,.T.);
#17092=ORIENTED_EDGE('',*,*,#12567,.T.);
#17093=ORIENTED_EDGE('',*,*,#12563,.F.);
#17094=ORIENTED_EDGE('',*,*,#12568,.F.);
#17095=ORIENTED_EDGE('',*,*,#12569,.T.);
#17096=ORIENTED_EDGE('',*,*,#12570,.T.);
#17097=ORIENTED_EDGE('',*,*,#12566,.F.);
#17098=ORIENTED_EDGE('',*,*,#12571,.F.);
#17099=ORIENTED_EDGE('',*,*,#12572,.T.);
#17100=ORIENTED_EDGE('',*,*,#12573,.T.);
#17101=ORIENTED_EDGE('',*,*,#12569,.F.);
#17102=ORIENTED_EDGE('',*,*,#12574,.F.);
#17103=ORIENTED_EDGE('',*,*,#12575,.T.);
#17104=ORIENTED_EDGE('',*,*,#12576,.T.);
#17105=ORIENTED_EDGE('',*,*,#12572,.F.);
#17106=ORIENTED_EDGE('',*,*,#12577,.F.);
#17107=ORIENTED_EDGE('',*,*,#12578,.T.);
#17108=ORIENTED_EDGE('',*,*,#12579,.T.);
#17109=ORIENTED_EDGE('',*,*,#12575,.F.);
#17110=ORIENTED_EDGE('',*,*,#12580,.F.);
#17111=ORIENTED_EDGE('',*,*,#12581,.T.);
#17112=ORIENTED_EDGE('',*,*,#12582,.T.);
#17113=ORIENTED_EDGE('',*,*,#12578,.F.);
#17114=ORIENTED_EDGE('',*,*,#12583,.F.);
#17115=ORIENTED_EDGE('',*,*,#12584,.T.);
#17116=ORIENTED_EDGE('',*,*,#12585,.T.);
#17117=ORIENTED_EDGE('',*,*,#12581,.F.);
#17118=ORIENTED_EDGE('',*,*,#12586,.F.);
#17119=ORIENTED_EDGE('',*,*,#12587,.T.);
#17120=ORIENTED_EDGE('',*,*,#12588,.T.);
#17121=ORIENTED_EDGE('',*,*,#12584,.F.);
#17122=ORIENTED_EDGE('',*,*,#12589,.F.);
#17123=ORIENTED_EDGE('',*,*,#12590,.T.);
#17124=ORIENTED_EDGE('',*,*,#12591,.T.);
#17125=ORIENTED_EDGE('',*,*,#12587,.F.);
#17126=ORIENTED_EDGE('',*,*,#12592,.F.);
#17127=ORIENTED_EDGE('',*,*,#12593,.T.);
#17128=ORIENTED_EDGE('',*,*,#12594,.T.);
#17129=ORIENTED_EDGE('',*,*,#12590,.F.);
#17130=ORIENTED_EDGE('',*,*,#12595,.F.);
#17131=ORIENTED_EDGE('',*,*,#12596,.T.);
#17132=ORIENTED_EDGE('',*,*,#12597,.T.);
#17133=ORIENTED_EDGE('',*,*,#12593,.F.);
#17134=ORIENTED_EDGE('',*,*,#12598,.F.);
#17135=ORIENTED_EDGE('',*,*,#12599,.T.);
#17136=ORIENTED_EDGE('',*,*,#12600,.T.);
#17137=ORIENTED_EDGE('',*,*,#12596,.F.);
#17138=ORIENTED_EDGE('',*,*,#12601,.F.);
#17139=ORIENTED_EDGE('',*,*,#12602,.T.);
#17140=ORIENTED_EDGE('',*,*,#12603,.T.);
#17141=ORIENTED_EDGE('',*,*,#12599,.F.);
#17142=ORIENTED_EDGE('',*,*,#12604,.F.);
#17143=ORIENTED_EDGE('',*,*,#12605,.T.);
#17144=ORIENTED_EDGE('',*,*,#12606,.T.);
#17145=ORIENTED_EDGE('',*,*,#12602,.F.);
#17146=ORIENTED_EDGE('',*,*,#12607,.F.);
#17147=ORIENTED_EDGE('',*,*,#12608,.T.);
#17148=ORIENTED_EDGE('',*,*,#12609,.T.);
#17149=ORIENTED_EDGE('',*,*,#12605,.F.);
#17150=ORIENTED_EDGE('',*,*,#12610,.F.);
#17151=ORIENTED_EDGE('',*,*,#12611,.T.);
#17152=ORIENTED_EDGE('',*,*,#12612,.T.);
#17153=ORIENTED_EDGE('',*,*,#12608,.F.);
#17154=ORIENTED_EDGE('',*,*,#12613,.F.);
#17155=ORIENTED_EDGE('',*,*,#12614,.T.);
#17156=ORIENTED_EDGE('',*,*,#12615,.T.);
#17157=ORIENTED_EDGE('',*,*,#12611,.F.);
#17158=ORIENTED_EDGE('',*,*,#12616,.F.);
#17159=ORIENTED_EDGE('',*,*,#12617,.T.);
#17160=ORIENTED_EDGE('',*,*,#12618,.T.);
#17161=ORIENTED_EDGE('',*,*,#12614,.F.);
#17162=ORIENTED_EDGE('',*,*,#12619,.F.);
#17163=ORIENTED_EDGE('',*,*,#12620,.T.);
#17164=ORIENTED_EDGE('',*,*,#12621,.T.);
#17165=ORIENTED_EDGE('',*,*,#12617,.F.);
#17166=ORIENTED_EDGE('',*,*,#12622,.F.);
#17167=ORIENTED_EDGE('',*,*,#12623,.T.);
#17168=ORIENTED_EDGE('',*,*,#12624,.T.);
#17169=ORIENTED_EDGE('',*,*,#12620,.F.);
#17170=ORIENTED_EDGE('',*,*,#12625,.F.);
#17171=ORIENTED_EDGE('',*,*,#12626,.T.);
#17172=ORIENTED_EDGE('',*,*,#12627,.T.);
#17173=ORIENTED_EDGE('',*,*,#12623,.F.);
#17174=ORIENTED_EDGE('',*,*,#12628,.F.);
#17175=ORIENTED_EDGE('',*,*,#12552,.T.);
#17176=ORIENTED_EDGE('',*,*,#12629,.T.);
#17177=ORIENTED_EDGE('',*,*,#12626,.F.);
#17178=ORIENTED_EDGE('',*,*,#12629,.F.);
#17179=ORIENTED_EDGE('',*,*,#12551,.F.);
#17180=ORIENTED_EDGE('',*,*,#12555,.F.);
#17181=ORIENTED_EDGE('',*,*,#12558,.F.);
#17182=ORIENTED_EDGE('',*,*,#12561,.F.);
#17183=ORIENTED_EDGE('',*,*,#12564,.F.);
#17184=ORIENTED_EDGE('',*,*,#12567,.F.);
#17185=ORIENTED_EDGE('',*,*,#12570,.F.);
#17186=ORIENTED_EDGE('',*,*,#12573,.F.);
#17187=ORIENTED_EDGE('',*,*,#12576,.F.);
#17188=ORIENTED_EDGE('',*,*,#12579,.F.);
#17189=ORIENTED_EDGE('',*,*,#12582,.F.);
#17190=ORIENTED_EDGE('',*,*,#12585,.F.);
#17191=ORIENTED_EDGE('',*,*,#12588,.F.);
#17192=ORIENTED_EDGE('',*,*,#12591,.F.);
#17193=ORIENTED_EDGE('',*,*,#12594,.F.);
#17194=ORIENTED_EDGE('',*,*,#12597,.F.);
#17195=ORIENTED_EDGE('',*,*,#12600,.F.);
#17196=ORIENTED_EDGE('',*,*,#12603,.F.);
#17197=ORIENTED_EDGE('',*,*,#12606,.F.);
#17198=ORIENTED_EDGE('',*,*,#12609,.F.);
#17199=ORIENTED_EDGE('',*,*,#12612,.F.);
#17200=ORIENTED_EDGE('',*,*,#12615,.F.);
#17201=ORIENTED_EDGE('',*,*,#12618,.F.);
#17202=ORIENTED_EDGE('',*,*,#12621,.F.);
#17203=ORIENTED_EDGE('',*,*,#12624,.F.);
#17204=ORIENTED_EDGE('',*,*,#12627,.F.);
#17205=ORIENTED_EDGE('',*,*,#12548,.F.);
#17206=ORIENTED_EDGE('',*,*,#12521,.F.);
#17207=ORIENTED_EDGE('',*,*,#12525,.F.);
#17208=ORIENTED_EDGE('',*,*,#12528,.F.);
#17209=ORIENTED_EDGE('',*,*,#12531,.F.);
#17210=ORIENTED_EDGE('',*,*,#12534,.F.);
#17211=ORIENTED_EDGE('',*,*,#12537,.F.);
#17212=ORIENTED_EDGE('',*,*,#12540,.F.);
#17213=ORIENTED_EDGE('',*,*,#12543,.F.);
#17214=ORIENTED_EDGE('',*,*,#12546,.F.);
#17215=ORIENTED_EDGE('',*,*,#12630,.F.);
#17216=ORIENTED_EDGE('',*,*,#12631,.T.);
#17217=ORIENTED_EDGE('',*,*,#12632,.T.);
#17218=ORIENTED_EDGE('',*,*,#12633,.F.);
#17219=ORIENTED_EDGE('',*,*,#12634,.F.);
#17220=ORIENTED_EDGE('',*,*,#12635,.T.);
#17221=ORIENTED_EDGE('',*,*,#12636,.T.);
#17222=ORIENTED_EDGE('',*,*,#12631,.F.);
#17223=ORIENTED_EDGE('',*,*,#12637,.F.);
#17224=ORIENTED_EDGE('',*,*,#12638,.T.);
#17225=ORIENTED_EDGE('',*,*,#12639,.T.);
#17226=ORIENTED_EDGE('',*,*,#12635,.F.);
#17227=ORIENTED_EDGE('',*,*,#12640,.F.);
#17228=ORIENTED_EDGE('',*,*,#12641,.T.);
#17229=ORIENTED_EDGE('',*,*,#12642,.T.);
#17230=ORIENTED_EDGE('',*,*,#12638,.F.);
#17231=ORIENTED_EDGE('',*,*,#12643,.F.);
#17232=ORIENTED_EDGE('',*,*,#12644,.T.);
#17233=ORIENTED_EDGE('',*,*,#12645,.T.);
#17234=ORIENTED_EDGE('',*,*,#12641,.F.);
#17235=ORIENTED_EDGE('',*,*,#12646,.F.);
#17236=ORIENTED_EDGE('',*,*,#12647,.T.);
#17237=ORIENTED_EDGE('',*,*,#12648,.T.);
#17238=ORIENTED_EDGE('',*,*,#12644,.F.);
#17239=ORIENTED_EDGE('',*,*,#12649,.F.);
#17240=ORIENTED_EDGE('',*,*,#12650,.T.);
#17241=ORIENTED_EDGE('',*,*,#12651,.T.);
#17242=ORIENTED_EDGE('',*,*,#12647,.F.);
#17243=ORIENTED_EDGE('',*,*,#12652,.F.);
#17244=ORIENTED_EDGE('',*,*,#12633,.T.);
#17245=ORIENTED_EDGE('',*,*,#12653,.T.);
#17246=ORIENTED_EDGE('',*,*,#12650,.F.);
#17247=ORIENTED_EDGE('',*,*,#12654,.F.);
#17248=ORIENTED_EDGE('',*,*,#12655,.T.);
#17249=ORIENTED_EDGE('',*,*,#12656,.T.);
#17250=ORIENTED_EDGE('',*,*,#12657,.F.);
#17251=ORIENTED_EDGE('',*,*,#12658,.F.);
#17252=ORIENTED_EDGE('',*,*,#12659,.T.);
#17253=ORIENTED_EDGE('',*,*,#12660,.T.);
#17254=ORIENTED_EDGE('',*,*,#12655,.F.);
#17255=ORIENTED_EDGE('',*,*,#12661,.F.);
#17256=ORIENTED_EDGE('',*,*,#12662,.T.);
#17257=ORIENTED_EDGE('',*,*,#12663,.T.);
#17258=ORIENTED_EDGE('',*,*,#12659,.F.);
#17259=ORIENTED_EDGE('',*,*,#12664,.F.);
#17260=ORIENTED_EDGE('',*,*,#12665,.T.);
#17261=ORIENTED_EDGE('',*,*,#12666,.T.);
#17262=ORIENTED_EDGE('',*,*,#12662,.F.);
#17263=ORIENTED_EDGE('',*,*,#12667,.F.);
#17264=ORIENTED_EDGE('',*,*,#12668,.T.);
#17265=ORIENTED_EDGE('',*,*,#12669,.T.);
#17266=ORIENTED_EDGE('',*,*,#12665,.F.);
#17267=ORIENTED_EDGE('',*,*,#12670,.F.);
#17268=ORIENTED_EDGE('',*,*,#12671,.T.);
#17269=ORIENTED_EDGE('',*,*,#12672,.T.);
#17270=ORIENTED_EDGE('',*,*,#12668,.F.);
#17271=ORIENTED_EDGE('',*,*,#12673,.F.);
#17272=ORIENTED_EDGE('',*,*,#12674,.T.);
#17273=ORIENTED_EDGE('',*,*,#12675,.T.);
#17274=ORIENTED_EDGE('',*,*,#12671,.F.);
#17275=ORIENTED_EDGE('',*,*,#12676,.F.);
#17276=ORIENTED_EDGE('',*,*,#12677,.T.);
#17277=ORIENTED_EDGE('',*,*,#12678,.T.);
#17278=ORIENTED_EDGE('',*,*,#12674,.F.);
#17279=ORIENTED_EDGE('',*,*,#12679,.F.);
#17280=ORIENTED_EDGE('',*,*,#12680,.T.);
#17281=ORIENTED_EDGE('',*,*,#12681,.T.);
#17282=ORIENTED_EDGE('',*,*,#12677,.F.);
#17283=ORIENTED_EDGE('',*,*,#12682,.F.);
#17284=ORIENTED_EDGE('',*,*,#12683,.T.);
#17285=ORIENTED_EDGE('',*,*,#12684,.T.);
#17286=ORIENTED_EDGE('',*,*,#12680,.F.);
#17287=ORIENTED_EDGE('',*,*,#12685,.F.);
#17288=ORIENTED_EDGE('',*,*,#12686,.T.);
#17289=ORIENTED_EDGE('',*,*,#12687,.T.);
#17290=ORIENTED_EDGE('',*,*,#12683,.F.);
#17291=ORIENTED_EDGE('',*,*,#12688,.F.);
#17292=ORIENTED_EDGE('',*,*,#12657,.T.);
#17293=ORIENTED_EDGE('',*,*,#12689,.T.);
#17294=ORIENTED_EDGE('',*,*,#12686,.F.);
#17295=ORIENTED_EDGE('',*,*,#12689,.F.);
#17296=ORIENTED_EDGE('',*,*,#12656,.F.);
#17297=ORIENTED_EDGE('',*,*,#12660,.F.);
#17298=ORIENTED_EDGE('',*,*,#12663,.F.);
#17299=ORIENTED_EDGE('',*,*,#12666,.F.);
#17300=ORIENTED_EDGE('',*,*,#12669,.F.);
#17301=ORIENTED_EDGE('',*,*,#12672,.F.);
#17302=ORIENTED_EDGE('',*,*,#12675,.F.);
#17303=ORIENTED_EDGE('',*,*,#12678,.F.);
#17304=ORIENTED_EDGE('',*,*,#12681,.F.);
#17305=ORIENTED_EDGE('',*,*,#12684,.F.);
#17306=ORIENTED_EDGE('',*,*,#12687,.F.);
#17307=ORIENTED_EDGE('',*,*,#12653,.F.);
#17308=ORIENTED_EDGE('',*,*,#12632,.F.);
#17309=ORIENTED_EDGE('',*,*,#12636,.F.);
#17310=ORIENTED_EDGE('',*,*,#12639,.F.);
#17311=ORIENTED_EDGE('',*,*,#12642,.F.);
#17312=ORIENTED_EDGE('',*,*,#12645,.F.);
#17313=ORIENTED_EDGE('',*,*,#12648,.F.);
#17314=ORIENTED_EDGE('',*,*,#12651,.F.);
#17315=ORIENTED_EDGE('',*,*,#12690,.F.);
#17316=ORIENTED_EDGE('',*,*,#12691,.T.);
#17317=ORIENTED_EDGE('',*,*,#12692,.T.);
#17318=ORIENTED_EDGE('',*,*,#12693,.F.);
#17319=ORIENTED_EDGE('',*,*,#12694,.F.);
#17320=ORIENTED_EDGE('',*,*,#12695,.T.);
#17321=ORIENTED_EDGE('',*,*,#12696,.T.);
#17322=ORIENTED_EDGE('',*,*,#12691,.F.);
#17323=ORIENTED_EDGE('',*,*,#12697,.F.);
#17324=ORIENTED_EDGE('',*,*,#12698,.T.);
#17325=ORIENTED_EDGE('',*,*,#12699,.T.);
#17326=ORIENTED_EDGE('',*,*,#12695,.F.);
#17327=ORIENTED_EDGE('',*,*,#12700,.F.);
#17328=ORIENTED_EDGE('',*,*,#12701,.T.);
#17329=ORIENTED_EDGE('',*,*,#12702,.T.);
#17330=ORIENTED_EDGE('',*,*,#12698,.F.);
#17331=ORIENTED_EDGE('',*,*,#12703,.F.);
#17332=ORIENTED_EDGE('',*,*,#12704,.T.);
#17333=ORIENTED_EDGE('',*,*,#12705,.T.);
#17334=ORIENTED_EDGE('',*,*,#12701,.F.);
#17335=ORIENTED_EDGE('',*,*,#12706,.F.);
#17336=ORIENTED_EDGE('',*,*,#12707,.T.);
#17337=ORIENTED_EDGE('',*,*,#12708,.T.);
#17338=ORIENTED_EDGE('',*,*,#12704,.F.);
#17339=ORIENTED_EDGE('',*,*,#12709,.F.);
#17340=ORIENTED_EDGE('',*,*,#12710,.T.);
#17341=ORIENTED_EDGE('',*,*,#12711,.T.);
#17342=ORIENTED_EDGE('',*,*,#12707,.F.);
#17343=ORIENTED_EDGE('',*,*,#12712,.F.);
#17344=ORIENTED_EDGE('',*,*,#12713,.T.);
#17345=ORIENTED_EDGE('',*,*,#12714,.T.);
#17346=ORIENTED_EDGE('',*,*,#12710,.F.);
#17347=ORIENTED_EDGE('',*,*,#12715,.F.);
#17348=ORIENTED_EDGE('',*,*,#12693,.T.);
#17349=ORIENTED_EDGE('',*,*,#12716,.T.);
#17350=ORIENTED_EDGE('',*,*,#12713,.F.);
#17351=ORIENTED_EDGE('',*,*,#12716,.F.);
#17352=ORIENTED_EDGE('',*,*,#12692,.F.);
#17353=ORIENTED_EDGE('',*,*,#12696,.F.);
#17354=ORIENTED_EDGE('',*,*,#12699,.F.);
#17355=ORIENTED_EDGE('',*,*,#12702,.F.);
#17356=ORIENTED_EDGE('',*,*,#12705,.F.);
#17357=ORIENTED_EDGE('',*,*,#12708,.F.);
#17358=ORIENTED_EDGE('',*,*,#12711,.F.);
#17359=ORIENTED_EDGE('',*,*,#12714,.F.);
#17360=ORIENTED_EDGE('',*,*,#12717,.F.);
#17361=ORIENTED_EDGE('',*,*,#12718,.T.);
#17362=ORIENTED_EDGE('',*,*,#12719,.T.);
#17363=ORIENTED_EDGE('',*,*,#12720,.F.);
#17364=ORIENTED_EDGE('',*,*,#12721,.F.);
#17365=ORIENTED_EDGE('',*,*,#12722,.T.);
#17366=ORIENTED_EDGE('',*,*,#12723,.T.);
#17367=ORIENTED_EDGE('',*,*,#12718,.F.);
#17368=ORIENTED_EDGE('',*,*,#12724,.F.);
#17369=ORIENTED_EDGE('',*,*,#12725,.T.);
#17370=ORIENTED_EDGE('',*,*,#12726,.T.);
#17371=ORIENTED_EDGE('',*,*,#12722,.F.);
#17372=ORIENTED_EDGE('',*,*,#12727,.F.);
#17373=ORIENTED_EDGE('',*,*,#12728,.T.);
#17374=ORIENTED_EDGE('',*,*,#12729,.T.);
#17375=ORIENTED_EDGE('',*,*,#12725,.F.);
#17376=ORIENTED_EDGE('',*,*,#12730,.F.);
#17377=ORIENTED_EDGE('',*,*,#12731,.T.);
#17378=ORIENTED_EDGE('',*,*,#12732,.T.);
#17379=ORIENTED_EDGE('',*,*,#12728,.F.);
#17380=ORIENTED_EDGE('',*,*,#12733,.F.);
#17381=ORIENTED_EDGE('',*,*,#12734,.T.);
#17382=ORIENTED_EDGE('',*,*,#12735,.T.);
#17383=ORIENTED_EDGE('',*,*,#12731,.F.);
#17384=ORIENTED_EDGE('',*,*,#12736,.F.);
#17385=ORIENTED_EDGE('',*,*,#12737,.T.);
#17386=ORIENTED_EDGE('',*,*,#12738,.T.);
#17387=ORIENTED_EDGE('',*,*,#12734,.F.);
#17388=ORIENTED_EDGE('',*,*,#12739,.F.);
#17389=ORIENTED_EDGE('',*,*,#12740,.T.);
#17390=ORIENTED_EDGE('',*,*,#12741,.T.);
#17391=ORIENTED_EDGE('',*,*,#12737,.F.);
#17392=ORIENTED_EDGE('',*,*,#12742,.F.);
#17393=ORIENTED_EDGE('',*,*,#12743,.T.);
#17394=ORIENTED_EDGE('',*,*,#12744,.T.);
#17395=ORIENTED_EDGE('',*,*,#12740,.F.);
#17396=ORIENTED_EDGE('',*,*,#12745,.F.);
#17397=ORIENTED_EDGE('',*,*,#12746,.T.);
#17398=ORIENTED_EDGE('',*,*,#12747,.T.);
#17399=ORIENTED_EDGE('',*,*,#12743,.F.);
#17400=ORIENTED_EDGE('',*,*,#12748,.F.);
#17401=ORIENTED_EDGE('',*,*,#12749,.T.);
#17402=ORIENTED_EDGE('',*,*,#12750,.T.);
#17403=ORIENTED_EDGE('',*,*,#12746,.F.);
#17404=ORIENTED_EDGE('',*,*,#12751,.F.);
#17405=ORIENTED_EDGE('',*,*,#12752,.T.);
#17406=ORIENTED_EDGE('',*,*,#12753,.T.);
#17407=ORIENTED_EDGE('',*,*,#12749,.F.);
#17408=ORIENTED_EDGE('',*,*,#12754,.F.);
#17409=ORIENTED_EDGE('',*,*,#12755,.T.);
#17410=ORIENTED_EDGE('',*,*,#12756,.T.);
#17411=ORIENTED_EDGE('',*,*,#12752,.F.);
#17412=ORIENTED_EDGE('',*,*,#12757,.F.);
#17413=ORIENTED_EDGE('',*,*,#12758,.T.);
#17414=ORIENTED_EDGE('',*,*,#12759,.T.);
#17415=ORIENTED_EDGE('',*,*,#12755,.F.);
#17416=ORIENTED_EDGE('',*,*,#12760,.F.);
#17417=ORIENTED_EDGE('',*,*,#12720,.T.);
#17418=ORIENTED_EDGE('',*,*,#12761,.T.);
#17419=ORIENTED_EDGE('',*,*,#12758,.F.);
#17420=ORIENTED_EDGE('',*,*,#12761,.F.);
#17421=ORIENTED_EDGE('',*,*,#12719,.F.);
#17422=ORIENTED_EDGE('',*,*,#12723,.F.);
#17423=ORIENTED_EDGE('',*,*,#12726,.F.);
#17424=ORIENTED_EDGE('',*,*,#12729,.F.);
#17425=ORIENTED_EDGE('',*,*,#12732,.F.);
#17426=ORIENTED_EDGE('',*,*,#12735,.F.);
#17427=ORIENTED_EDGE('',*,*,#12738,.F.);
#17428=ORIENTED_EDGE('',*,*,#12741,.F.);
#17429=ORIENTED_EDGE('',*,*,#12744,.F.);
#17430=ORIENTED_EDGE('',*,*,#12747,.F.);
#17431=ORIENTED_EDGE('',*,*,#12750,.F.);
#17432=ORIENTED_EDGE('',*,*,#12753,.F.);
#17433=ORIENTED_EDGE('',*,*,#12756,.F.);
#17434=ORIENTED_EDGE('',*,*,#12759,.F.);
#17435=ORIENTED_EDGE('',*,*,#12762,.F.);
#17436=ORIENTED_EDGE('',*,*,#12763,.T.);
#17437=ORIENTED_EDGE('',*,*,#12764,.T.);
#17438=ORIENTED_EDGE('',*,*,#12765,.F.);
#17439=ORIENTED_EDGE('',*,*,#12766,.F.);
#17440=ORIENTED_EDGE('',*,*,#12767,.T.);
#17441=ORIENTED_EDGE('',*,*,#12768,.T.);
#17442=ORIENTED_EDGE('',*,*,#12763,.F.);
#17443=ORIENTED_EDGE('',*,*,#12769,.F.);
#17444=ORIENTED_EDGE('',*,*,#12770,.T.);
#17445=ORIENTED_EDGE('',*,*,#12771,.T.);
#17446=ORIENTED_EDGE('',*,*,#12767,.F.);
#17447=ORIENTED_EDGE('',*,*,#12772,.F.);
#17448=ORIENTED_EDGE('',*,*,#12773,.T.);
#17449=ORIENTED_EDGE('',*,*,#12774,.T.);
#17450=ORIENTED_EDGE('',*,*,#12770,.F.);
#17451=ORIENTED_EDGE('',*,*,#12775,.F.);
#17452=ORIENTED_EDGE('',*,*,#12776,.T.);
#17453=ORIENTED_EDGE('',*,*,#12777,.T.);
#17454=ORIENTED_EDGE('',*,*,#12773,.F.);
#17455=ORIENTED_EDGE('',*,*,#12778,.F.);
#17456=ORIENTED_EDGE('',*,*,#12779,.T.);
#17457=ORIENTED_EDGE('',*,*,#12780,.T.);
#17458=ORIENTED_EDGE('',*,*,#12776,.F.);
#17459=ORIENTED_EDGE('',*,*,#12781,.F.);
#17460=ORIENTED_EDGE('',*,*,#12782,.T.);
#17461=ORIENTED_EDGE('',*,*,#12783,.T.);
#17462=ORIENTED_EDGE('',*,*,#12779,.F.);
#17463=ORIENTED_EDGE('',*,*,#12784,.F.);
#17464=ORIENTED_EDGE('',*,*,#12785,.T.);
#17465=ORIENTED_EDGE('',*,*,#12786,.T.);
#17466=ORIENTED_EDGE('',*,*,#12782,.F.);
#17467=ORIENTED_EDGE('',*,*,#12787,.F.);
#17468=ORIENTED_EDGE('',*,*,#12788,.T.);
#17469=ORIENTED_EDGE('',*,*,#12789,.T.);
#17470=ORIENTED_EDGE('',*,*,#12785,.F.);
#17471=ORIENTED_EDGE('',*,*,#12790,.F.);
#17472=ORIENTED_EDGE('',*,*,#12791,.T.);
#17473=ORIENTED_EDGE('',*,*,#12792,.T.);
#17474=ORIENTED_EDGE('',*,*,#12788,.F.);
#17475=ORIENTED_EDGE('',*,*,#12793,.F.);
#17476=ORIENTED_EDGE('',*,*,#12794,.T.);
#17477=ORIENTED_EDGE('',*,*,#12795,.T.);
#17478=ORIENTED_EDGE('',*,*,#12791,.F.);
#17479=ORIENTED_EDGE('',*,*,#12796,.F.);
#17480=ORIENTED_EDGE('',*,*,#12797,.T.);
#17481=ORIENTED_EDGE('',*,*,#12798,.T.);
#17482=ORIENTED_EDGE('',*,*,#12794,.F.);
#17483=ORIENTED_EDGE('',*,*,#12799,.F.);
#17484=ORIENTED_EDGE('',*,*,#12800,.T.);
#17485=ORIENTED_EDGE('',*,*,#12801,.T.);
#17486=ORIENTED_EDGE('',*,*,#12797,.F.);
#17487=ORIENTED_EDGE('',*,*,#12802,.F.);
#17488=ORIENTED_EDGE('',*,*,#12803,.T.);
#17489=ORIENTED_EDGE('',*,*,#12804,.T.);
#17490=ORIENTED_EDGE('',*,*,#12800,.F.);
#17491=ORIENTED_EDGE('',*,*,#12805,.F.);
#17492=ORIENTED_EDGE('',*,*,#12806,.T.);
#17493=ORIENTED_EDGE('',*,*,#12807,.T.);
#17494=ORIENTED_EDGE('',*,*,#12803,.F.);
#17495=ORIENTED_EDGE('',*,*,#12808,.F.);
#17496=ORIENTED_EDGE('',*,*,#12809,.T.);
#17497=ORIENTED_EDGE('',*,*,#12810,.T.);
#17498=ORIENTED_EDGE('',*,*,#12806,.F.);
#17499=ORIENTED_EDGE('',*,*,#12811,.F.);
#17500=ORIENTED_EDGE('',*,*,#12812,.T.);
#17501=ORIENTED_EDGE('',*,*,#12813,.T.);
#17502=ORIENTED_EDGE('',*,*,#12809,.F.);
#17503=ORIENTED_EDGE('',*,*,#12814,.F.);
#17504=ORIENTED_EDGE('',*,*,#12815,.T.);
#17505=ORIENTED_EDGE('',*,*,#12816,.T.);
#17506=ORIENTED_EDGE('',*,*,#12812,.F.);
#17507=ORIENTED_EDGE('',*,*,#12817,.F.);
#17508=ORIENTED_EDGE('',*,*,#12818,.T.);
#17509=ORIENTED_EDGE('',*,*,#12819,.T.);
#17510=ORIENTED_EDGE('',*,*,#12815,.F.);
#17511=ORIENTED_EDGE('',*,*,#12820,.F.);
#17512=ORIENTED_EDGE('',*,*,#12821,.T.);
#17513=ORIENTED_EDGE('',*,*,#12822,.T.);
#17514=ORIENTED_EDGE('',*,*,#12818,.F.);
#17515=ORIENTED_EDGE('',*,*,#12823,.F.);
#17516=ORIENTED_EDGE('',*,*,#12824,.T.);
#17517=ORIENTED_EDGE('',*,*,#12825,.T.);
#17518=ORIENTED_EDGE('',*,*,#12821,.F.);
#17519=ORIENTED_EDGE('',*,*,#12826,.F.);
#17520=ORIENTED_EDGE('',*,*,#12827,.T.);
#17521=ORIENTED_EDGE('',*,*,#12828,.T.);
#17522=ORIENTED_EDGE('',*,*,#12824,.F.);
#17523=ORIENTED_EDGE('',*,*,#12829,.F.);
#17524=ORIENTED_EDGE('',*,*,#12830,.T.);
#17525=ORIENTED_EDGE('',*,*,#12831,.T.);
#17526=ORIENTED_EDGE('',*,*,#12827,.F.);
#17527=ORIENTED_EDGE('',*,*,#12832,.F.);
#17528=ORIENTED_EDGE('',*,*,#12833,.T.);
#17529=ORIENTED_EDGE('',*,*,#12834,.T.);
#17530=ORIENTED_EDGE('',*,*,#12830,.F.);
#17531=ORIENTED_EDGE('',*,*,#12835,.F.);
#17532=ORIENTED_EDGE('',*,*,#12836,.T.);
#17533=ORIENTED_EDGE('',*,*,#12837,.T.);
#17534=ORIENTED_EDGE('',*,*,#12833,.F.);
#17535=ORIENTED_EDGE('',*,*,#12838,.F.);
#17536=ORIENTED_EDGE('',*,*,#12839,.T.);
#17537=ORIENTED_EDGE('',*,*,#12840,.T.);
#17538=ORIENTED_EDGE('',*,*,#12836,.F.);
#17539=ORIENTED_EDGE('',*,*,#12841,.F.);
#17540=ORIENTED_EDGE('',*,*,#12842,.T.);
#17541=ORIENTED_EDGE('',*,*,#12843,.T.);
#17542=ORIENTED_EDGE('',*,*,#12839,.F.);
#17543=ORIENTED_EDGE('',*,*,#12844,.F.);
#17544=ORIENTED_EDGE('',*,*,#12845,.T.);
#17545=ORIENTED_EDGE('',*,*,#12846,.T.);
#17546=ORIENTED_EDGE('',*,*,#12842,.F.);
#17547=ORIENTED_EDGE('',*,*,#12847,.F.);
#17548=ORIENTED_EDGE('',*,*,#12848,.T.);
#17549=ORIENTED_EDGE('',*,*,#12849,.T.);
#17550=ORIENTED_EDGE('',*,*,#12845,.F.);
#17551=ORIENTED_EDGE('',*,*,#12850,.F.);
#17552=ORIENTED_EDGE('',*,*,#12765,.T.);
#17553=ORIENTED_EDGE('',*,*,#12851,.T.);
#17554=ORIENTED_EDGE('',*,*,#12848,.F.);
#17555=ORIENTED_EDGE('',*,*,#12851,.F.);
#17556=ORIENTED_EDGE('',*,*,#12764,.F.);
#17557=ORIENTED_EDGE('',*,*,#12768,.F.);
#17558=ORIENTED_EDGE('',*,*,#12771,.F.);
#17559=ORIENTED_EDGE('',*,*,#12774,.F.);
#17560=ORIENTED_EDGE('',*,*,#12777,.F.);
#17561=ORIENTED_EDGE('',*,*,#12780,.F.);
#17562=ORIENTED_EDGE('',*,*,#12783,.F.);
#17563=ORIENTED_EDGE('',*,*,#12786,.F.);
#17564=ORIENTED_EDGE('',*,*,#12789,.F.);
#17565=ORIENTED_EDGE('',*,*,#12792,.F.);
#17566=ORIENTED_EDGE('',*,*,#12795,.F.);
#17567=ORIENTED_EDGE('',*,*,#12798,.F.);
#17568=ORIENTED_EDGE('',*,*,#12801,.F.);
#17569=ORIENTED_EDGE('',*,*,#12804,.F.);
#17570=ORIENTED_EDGE('',*,*,#12807,.F.);
#17571=ORIENTED_EDGE('',*,*,#12810,.F.);
#17572=ORIENTED_EDGE('',*,*,#12813,.F.);
#17573=ORIENTED_EDGE('',*,*,#12816,.F.);
#17574=ORIENTED_EDGE('',*,*,#12819,.F.);
#17575=ORIENTED_EDGE('',*,*,#12822,.F.);
#17576=ORIENTED_EDGE('',*,*,#12825,.F.);
#17577=ORIENTED_EDGE('',*,*,#12828,.F.);
#17578=ORIENTED_EDGE('',*,*,#12831,.F.);
#17579=ORIENTED_EDGE('',*,*,#12834,.F.);
#17580=ORIENTED_EDGE('',*,*,#12837,.F.);
#17581=ORIENTED_EDGE('',*,*,#12840,.F.);
#17582=ORIENTED_EDGE('',*,*,#12843,.F.);
#17583=ORIENTED_EDGE('',*,*,#12846,.F.);
#17584=ORIENTED_EDGE('',*,*,#12849,.F.);
#17585=ORIENTED_EDGE('',*,*,#12852,.F.);
#17586=ORIENTED_EDGE('',*,*,#12853,.T.);
#17587=ORIENTED_EDGE('',*,*,#12854,.T.);
#17588=ORIENTED_EDGE('',*,*,#12855,.F.);
#17589=ORIENTED_EDGE('',*,*,#12856,.F.);
#17590=ORIENTED_EDGE('',*,*,#12857,.T.);
#17591=ORIENTED_EDGE('',*,*,#12858,.T.);
#17592=ORIENTED_EDGE('',*,*,#12853,.F.);
#17593=ORIENTED_EDGE('',*,*,#12859,.F.);
#17594=ORIENTED_EDGE('',*,*,#12860,.T.);
#17595=ORIENTED_EDGE('',*,*,#12861,.T.);
#17596=ORIENTED_EDGE('',*,*,#12857,.F.);
#17597=ORIENTED_EDGE('',*,*,#12862,.F.);
#17598=ORIENTED_EDGE('',*,*,#12855,.T.);
#17599=ORIENTED_EDGE('',*,*,#12863,.T.);
#17600=ORIENTED_EDGE('',*,*,#12860,.F.);
#17601=ORIENTED_EDGE('',*,*,#12863,.F.);
#17602=ORIENTED_EDGE('',*,*,#12854,.F.);
#17603=ORIENTED_EDGE('',*,*,#12858,.F.);
#17604=ORIENTED_EDGE('',*,*,#12861,.F.);
#17605=ORIENTED_EDGE('',*,*,#12864,.F.);
#17606=ORIENTED_EDGE('',*,*,#12865,.T.);
#17607=ORIENTED_EDGE('',*,*,#12866,.T.);
#17608=ORIENTED_EDGE('',*,*,#12867,.F.);
#17609=ORIENTED_EDGE('',*,*,#12868,.F.);
#17610=ORIENTED_EDGE('',*,*,#12869,.T.);
#17611=ORIENTED_EDGE('',*,*,#12870,.T.);
#17612=ORIENTED_EDGE('',*,*,#12865,.F.);
#17613=ORIENTED_EDGE('',*,*,#12871,.F.);
#17614=ORIENTED_EDGE('',*,*,#12872,.T.);
#17615=ORIENTED_EDGE('',*,*,#12873,.T.);
#17616=ORIENTED_EDGE('',*,*,#12869,.F.);
#17617=ORIENTED_EDGE('',*,*,#12874,.F.);
#17618=ORIENTED_EDGE('',*,*,#12875,.T.);
#17619=ORIENTED_EDGE('',*,*,#12876,.T.);
#17620=ORIENTED_EDGE('',*,*,#12872,.F.);
#17621=ORIENTED_EDGE('',*,*,#12877,.F.);
#17622=ORIENTED_EDGE('',*,*,#12867,.T.);
#17623=ORIENTED_EDGE('',*,*,#12878,.T.);
#17624=ORIENTED_EDGE('',*,*,#12875,.F.);
#17625=ORIENTED_EDGE('',*,*,#12879,.F.);
#17626=ORIENTED_EDGE('',*,*,#12880,.T.);
#17627=ORIENTED_EDGE('',*,*,#12881,.T.);
#17628=ORIENTED_EDGE('',*,*,#12882,.F.);
#17629=ORIENTED_EDGE('',*,*,#12883,.F.);
#17630=ORIENTED_EDGE('',*,*,#12884,.T.);
#17631=ORIENTED_EDGE('',*,*,#12885,.T.);
#17632=ORIENTED_EDGE('',*,*,#12880,.F.);
#17633=ORIENTED_EDGE('',*,*,#12886,.F.);
#17634=ORIENTED_EDGE('',*,*,#12887,.T.);
#17635=ORIENTED_EDGE('',*,*,#12888,.T.);
#17636=ORIENTED_EDGE('',*,*,#12884,.F.);
#17637=ORIENTED_EDGE('',*,*,#12889,.F.);
#17638=ORIENTED_EDGE('',*,*,#12890,.T.);
#17639=ORIENTED_EDGE('',*,*,#12891,.T.);
#17640=ORIENTED_EDGE('',*,*,#12887,.F.);
#17641=ORIENTED_EDGE('',*,*,#12892,.F.);
#17642=ORIENTED_EDGE('',*,*,#12893,.T.);
#17643=ORIENTED_EDGE('',*,*,#12894,.T.);
#17644=ORIENTED_EDGE('',*,*,#12890,.F.);
#17645=ORIENTED_EDGE('',*,*,#12895,.F.);
#17646=ORIENTED_EDGE('',*,*,#12896,.T.);
#17647=ORIENTED_EDGE('',*,*,#12897,.T.);
#17648=ORIENTED_EDGE('',*,*,#12893,.F.);
#17649=ORIENTED_EDGE('',*,*,#12898,.F.);
#17650=ORIENTED_EDGE('',*,*,#12899,.T.);
#17651=ORIENTED_EDGE('',*,*,#12900,.T.);
#17652=ORIENTED_EDGE('',*,*,#12896,.F.);
#17653=ORIENTED_EDGE('',*,*,#12901,.F.);
#17654=ORIENTED_EDGE('',*,*,#12882,.T.);
#17655=ORIENTED_EDGE('',*,*,#12902,.T.);
#17656=ORIENTED_EDGE('',*,*,#12899,.F.);
#17657=ORIENTED_EDGE('',*,*,#12902,.F.);
#17658=ORIENTED_EDGE('',*,*,#12881,.F.);
#17659=ORIENTED_EDGE('',*,*,#12885,.F.);
#17660=ORIENTED_EDGE('',*,*,#12888,.F.);
#17661=ORIENTED_EDGE('',*,*,#12891,.F.);
#17662=ORIENTED_EDGE('',*,*,#12894,.F.);
#17663=ORIENTED_EDGE('',*,*,#12897,.F.);
#17664=ORIENTED_EDGE('',*,*,#12900,.F.);
#17665=ORIENTED_EDGE('',*,*,#12878,.F.);
#17666=ORIENTED_EDGE('',*,*,#12866,.F.);
#17667=ORIENTED_EDGE('',*,*,#12870,.F.);
#17668=ORIENTED_EDGE('',*,*,#12873,.F.);
#17669=ORIENTED_EDGE('',*,*,#12876,.F.);
#17670=ORIENTED_EDGE('',*,*,#12903,.F.);
#17671=ORIENTED_EDGE('',*,*,#12904,.T.);
#17672=ORIENTED_EDGE('',*,*,#12905,.T.);
#17673=ORIENTED_EDGE('',*,*,#12906,.F.);
#17674=ORIENTED_EDGE('',*,*,#12907,.F.);
#17675=ORIENTED_EDGE('',*,*,#12908,.T.);
#17676=ORIENTED_EDGE('',*,*,#12909,.T.);
#17677=ORIENTED_EDGE('',*,*,#12904,.F.);
#17678=ORIENTED_EDGE('',*,*,#12910,.F.);
#17679=ORIENTED_EDGE('',*,*,#12911,.T.);
#17680=ORIENTED_EDGE('',*,*,#12912,.T.);
#17681=ORIENTED_EDGE('',*,*,#12908,.F.);
#17682=ORIENTED_EDGE('',*,*,#12913,.F.);
#17683=ORIENTED_EDGE('',*,*,#12914,.T.);
#17684=ORIENTED_EDGE('',*,*,#12915,.T.);
#17685=ORIENTED_EDGE('',*,*,#12911,.F.);
#17686=ORIENTED_EDGE('',*,*,#12916,.F.);
#17687=ORIENTED_EDGE('',*,*,#12917,.T.);
#17688=ORIENTED_EDGE('',*,*,#12918,.T.);
#17689=ORIENTED_EDGE('',*,*,#12914,.F.);
#17690=ORIENTED_EDGE('',*,*,#12919,.F.);
#17691=ORIENTED_EDGE('',*,*,#12920,.T.);
#17692=ORIENTED_EDGE('',*,*,#12921,.T.);
#17693=ORIENTED_EDGE('',*,*,#12917,.F.);
#17694=ORIENTED_EDGE('',*,*,#12922,.F.);
#17695=ORIENTED_EDGE('',*,*,#12923,.T.);
#17696=ORIENTED_EDGE('',*,*,#12924,.T.);
#17697=ORIENTED_EDGE('',*,*,#12920,.F.);
#17698=ORIENTED_EDGE('',*,*,#12925,.F.);
#17699=ORIENTED_EDGE('',*,*,#12926,.T.);
#17700=ORIENTED_EDGE('',*,*,#12927,.T.);
#17701=ORIENTED_EDGE('',*,*,#12923,.F.);
#17702=ORIENTED_EDGE('',*,*,#12928,.F.);
#17703=ORIENTED_EDGE('',*,*,#12929,.T.);
#17704=ORIENTED_EDGE('',*,*,#12930,.T.);
#17705=ORIENTED_EDGE('',*,*,#12926,.F.);
#17706=ORIENTED_EDGE('',*,*,#12931,.F.);
#17707=ORIENTED_EDGE('',*,*,#12932,.T.);
#17708=ORIENTED_EDGE('',*,*,#12933,.T.);
#17709=ORIENTED_EDGE('',*,*,#12929,.F.);
#17710=ORIENTED_EDGE('',*,*,#12934,.F.);
#17711=ORIENTED_EDGE('',*,*,#12935,.T.);
#17712=ORIENTED_EDGE('',*,*,#12936,.T.);
#17713=ORIENTED_EDGE('',*,*,#12932,.F.);
#17714=ORIENTED_EDGE('',*,*,#12937,.F.);
#17715=ORIENTED_EDGE('',*,*,#12938,.T.);
#17716=ORIENTED_EDGE('',*,*,#12939,.T.);
#17717=ORIENTED_EDGE('',*,*,#12935,.F.);
#17718=ORIENTED_EDGE('',*,*,#12940,.F.);
#17719=ORIENTED_EDGE('',*,*,#12941,.T.);
#17720=ORIENTED_EDGE('',*,*,#12942,.T.);
#17721=ORIENTED_EDGE('',*,*,#12938,.F.);
#17722=ORIENTED_EDGE('',*,*,#12943,.F.);
#17723=ORIENTED_EDGE('',*,*,#12944,.T.);
#17724=ORIENTED_EDGE('',*,*,#12945,.T.);
#17725=ORIENTED_EDGE('',*,*,#12941,.F.);
#17726=ORIENTED_EDGE('',*,*,#12946,.F.);
#17727=ORIENTED_EDGE('',*,*,#12947,.T.);
#17728=ORIENTED_EDGE('',*,*,#12948,.T.);
#17729=ORIENTED_EDGE('',*,*,#12944,.F.);
#17730=ORIENTED_EDGE('',*,*,#12949,.F.);
#17731=ORIENTED_EDGE('',*,*,#12950,.T.);
#17732=ORIENTED_EDGE('',*,*,#12951,.T.);
#17733=ORIENTED_EDGE('',*,*,#12947,.F.);
#17734=ORIENTED_EDGE('',*,*,#12952,.F.);
#17735=ORIENTED_EDGE('',*,*,#12953,.T.);
#17736=ORIENTED_EDGE('',*,*,#12954,.T.);
#17737=ORIENTED_EDGE('',*,*,#12950,.F.);
#17738=ORIENTED_EDGE('',*,*,#12955,.F.);
#17739=ORIENTED_EDGE('',*,*,#12956,.T.);
#17740=ORIENTED_EDGE('',*,*,#12957,.T.);
#17741=ORIENTED_EDGE('',*,*,#12953,.F.);
#17742=ORIENTED_EDGE('',*,*,#12958,.F.);
#17743=ORIENTED_EDGE('',*,*,#12959,.T.);
#17744=ORIENTED_EDGE('',*,*,#12960,.T.);
#17745=ORIENTED_EDGE('',*,*,#12956,.F.);
#17746=ORIENTED_EDGE('',*,*,#12961,.F.);
#17747=ORIENTED_EDGE('',*,*,#12962,.T.);
#17748=ORIENTED_EDGE('',*,*,#12963,.T.);
#17749=ORIENTED_EDGE('',*,*,#12959,.F.);
#17750=ORIENTED_EDGE('',*,*,#12964,.F.);
#17751=ORIENTED_EDGE('',*,*,#12965,.T.);
#17752=ORIENTED_EDGE('',*,*,#12966,.T.);
#17753=ORIENTED_EDGE('',*,*,#12962,.F.);
#17754=ORIENTED_EDGE('',*,*,#12967,.F.);
#17755=ORIENTED_EDGE('',*,*,#12968,.T.);
#17756=ORIENTED_EDGE('',*,*,#12969,.T.);
#17757=ORIENTED_EDGE('',*,*,#12965,.F.);
#17758=ORIENTED_EDGE('',*,*,#12970,.F.);
#17759=ORIENTED_EDGE('',*,*,#12971,.T.);
#17760=ORIENTED_EDGE('',*,*,#12972,.T.);
#17761=ORIENTED_EDGE('',*,*,#12968,.F.);
#17762=ORIENTED_EDGE('',*,*,#12973,.F.);
#17763=ORIENTED_EDGE('',*,*,#12974,.T.);
#17764=ORIENTED_EDGE('',*,*,#12975,.T.);
#17765=ORIENTED_EDGE('',*,*,#12971,.F.);
#17766=ORIENTED_EDGE('',*,*,#12976,.F.);
#17767=ORIENTED_EDGE('',*,*,#12977,.T.);
#17768=ORIENTED_EDGE('',*,*,#12978,.T.);
#17769=ORIENTED_EDGE('',*,*,#12974,.F.);
#17770=ORIENTED_EDGE('',*,*,#12979,.F.);
#17771=ORIENTED_EDGE('',*,*,#12980,.T.);
#17772=ORIENTED_EDGE('',*,*,#12981,.T.);
#17773=ORIENTED_EDGE('',*,*,#12977,.F.);
#17774=ORIENTED_EDGE('',*,*,#12982,.F.);
#17775=ORIENTED_EDGE('',*,*,#12983,.T.);
#17776=ORIENTED_EDGE('',*,*,#12984,.T.);
#17777=ORIENTED_EDGE('',*,*,#12980,.F.);
#17778=ORIENTED_EDGE('',*,*,#12985,.F.);
#17779=ORIENTED_EDGE('',*,*,#12986,.T.);
#17780=ORIENTED_EDGE('',*,*,#12987,.T.);
#17781=ORIENTED_EDGE('',*,*,#12983,.F.);
#17782=ORIENTED_EDGE('',*,*,#12988,.F.);
#17783=ORIENTED_EDGE('',*,*,#12989,.T.);
#17784=ORIENTED_EDGE('',*,*,#12990,.T.);
#17785=ORIENTED_EDGE('',*,*,#12986,.F.);
#17786=ORIENTED_EDGE('',*,*,#12991,.F.);
#17787=ORIENTED_EDGE('',*,*,#12992,.T.);
#17788=ORIENTED_EDGE('',*,*,#12993,.T.);
#17789=ORIENTED_EDGE('',*,*,#12989,.F.);
#17790=ORIENTED_EDGE('',*,*,#12994,.F.);
#17791=ORIENTED_EDGE('',*,*,#12995,.T.);
#17792=ORIENTED_EDGE('',*,*,#12996,.T.);
#17793=ORIENTED_EDGE('',*,*,#12992,.F.);
#17794=ORIENTED_EDGE('',*,*,#12997,.F.);
#17795=ORIENTED_EDGE('',*,*,#12998,.T.);
#17796=ORIENTED_EDGE('',*,*,#12999,.T.);
#17797=ORIENTED_EDGE('',*,*,#12995,.F.);
#17798=ORIENTED_EDGE('',*,*,#13000,.F.);
#17799=ORIENTED_EDGE('',*,*,#13001,.T.);
#17800=ORIENTED_EDGE('',*,*,#13002,.T.);
#17801=ORIENTED_EDGE('',*,*,#12998,.F.);
#17802=ORIENTED_EDGE('',*,*,#13003,.F.);
#17803=ORIENTED_EDGE('',*,*,#13004,.T.);
#17804=ORIENTED_EDGE('',*,*,#13005,.T.);
#17805=ORIENTED_EDGE('',*,*,#13001,.F.);
#17806=ORIENTED_EDGE('',*,*,#13006,.F.);
#17807=ORIENTED_EDGE('',*,*,#12906,.T.);
#17808=ORIENTED_EDGE('',*,*,#13007,.T.);
#17809=ORIENTED_EDGE('',*,*,#13004,.F.);
#17810=ORIENTED_EDGE('',*,*,#13007,.F.);
#17811=ORIENTED_EDGE('',*,*,#12905,.F.);
#17812=ORIENTED_EDGE('',*,*,#12909,.F.);
#17813=ORIENTED_EDGE('',*,*,#12912,.F.);
#17814=ORIENTED_EDGE('',*,*,#12915,.F.);
#17815=ORIENTED_EDGE('',*,*,#12918,.F.);
#17816=ORIENTED_EDGE('',*,*,#12921,.F.);
#17817=ORIENTED_EDGE('',*,*,#12924,.F.);
#17818=ORIENTED_EDGE('',*,*,#12927,.F.);
#17819=ORIENTED_EDGE('',*,*,#12930,.F.);
#17820=ORIENTED_EDGE('',*,*,#12933,.F.);
#17821=ORIENTED_EDGE('',*,*,#12936,.F.);
#17822=ORIENTED_EDGE('',*,*,#12939,.F.);
#17823=ORIENTED_EDGE('',*,*,#12942,.F.);
#17824=ORIENTED_EDGE('',*,*,#12945,.F.);
#17825=ORIENTED_EDGE('',*,*,#12948,.F.);
#17826=ORIENTED_EDGE('',*,*,#12951,.F.);
#17827=ORIENTED_EDGE('',*,*,#12954,.F.);
#17828=ORIENTED_EDGE('',*,*,#12957,.F.);
#17829=ORIENTED_EDGE('',*,*,#12960,.F.);
#17830=ORIENTED_EDGE('',*,*,#12963,.F.);
#17831=ORIENTED_EDGE('',*,*,#12966,.F.);
#17832=ORIENTED_EDGE('',*,*,#12969,.F.);
#17833=ORIENTED_EDGE('',*,*,#12972,.F.);
#17834=ORIENTED_EDGE('',*,*,#12975,.F.);
#17835=ORIENTED_EDGE('',*,*,#12978,.F.);
#17836=ORIENTED_EDGE('',*,*,#12981,.F.);
#17837=ORIENTED_EDGE('',*,*,#12984,.F.);
#17838=ORIENTED_EDGE('',*,*,#12987,.F.);
#17839=ORIENTED_EDGE('',*,*,#12990,.F.);
#17840=ORIENTED_EDGE('',*,*,#12993,.F.);
#17841=ORIENTED_EDGE('',*,*,#12996,.F.);
#17842=ORIENTED_EDGE('',*,*,#12999,.F.);
#17843=ORIENTED_EDGE('',*,*,#13002,.F.);
#17844=ORIENTED_EDGE('',*,*,#13005,.F.);
#17845=ORIENTED_EDGE('',*,*,#13008,.F.);
#17846=ORIENTED_EDGE('',*,*,#13009,.T.);
#17847=ORIENTED_EDGE('',*,*,#13010,.T.);
#17848=ORIENTED_EDGE('',*,*,#13011,.F.);
#17849=ORIENTED_EDGE('',*,*,#13012,.F.);
#17850=ORIENTED_EDGE('',*,*,#13013,.T.);
#17851=ORIENTED_EDGE('',*,*,#13014,.T.);
#17852=ORIENTED_EDGE('',*,*,#13009,.F.);
#17853=ORIENTED_EDGE('',*,*,#13015,.F.);
#17854=ORIENTED_EDGE('',*,*,#13016,.T.);
#17855=ORIENTED_EDGE('',*,*,#13017,.T.);
#17856=ORIENTED_EDGE('',*,*,#13013,.F.);
#17857=ORIENTED_EDGE('',*,*,#13018,.F.);
#17858=ORIENTED_EDGE('',*,*,#13019,.T.);
#17859=ORIENTED_EDGE('',*,*,#13020,.T.);
#17860=ORIENTED_EDGE('',*,*,#13016,.F.);
#17861=ORIENTED_EDGE('',*,*,#13021,.F.);
#17862=ORIENTED_EDGE('',*,*,#13022,.T.);
#17863=ORIENTED_EDGE('',*,*,#13023,.T.);
#17864=ORIENTED_EDGE('',*,*,#13019,.F.);
#17865=ORIENTED_EDGE('',*,*,#13024,.F.);
#17866=ORIENTED_EDGE('',*,*,#13025,.T.);
#17867=ORIENTED_EDGE('',*,*,#13026,.T.);
#17868=ORIENTED_EDGE('',*,*,#13022,.F.);
#17869=ORIENTED_EDGE('',*,*,#13027,.F.);
#17870=ORIENTED_EDGE('',*,*,#13028,.T.);
#17871=ORIENTED_EDGE('',*,*,#13029,.T.);
#17872=ORIENTED_EDGE('',*,*,#13025,.F.);
#17873=ORIENTED_EDGE('',*,*,#13030,.F.);
#17874=ORIENTED_EDGE('',*,*,#13031,.T.);
#17875=ORIENTED_EDGE('',*,*,#13032,.T.);
#17876=ORIENTED_EDGE('',*,*,#13028,.F.);
#17877=ORIENTED_EDGE('',*,*,#13033,.F.);
#17878=ORIENTED_EDGE('',*,*,#13034,.T.);
#17879=ORIENTED_EDGE('',*,*,#13035,.T.);
#17880=ORIENTED_EDGE('',*,*,#13031,.F.);
#17881=ORIENTED_EDGE('',*,*,#13036,.F.);
#17882=ORIENTED_EDGE('',*,*,#13037,.T.);
#17883=ORIENTED_EDGE('',*,*,#13038,.T.);
#17884=ORIENTED_EDGE('',*,*,#13034,.F.);
#17885=ORIENTED_EDGE('',*,*,#13039,.F.);
#17886=ORIENTED_EDGE('',*,*,#13040,.T.);
#17887=ORIENTED_EDGE('',*,*,#13041,.T.);
#17888=ORIENTED_EDGE('',*,*,#13037,.F.);
#17889=ORIENTED_EDGE('',*,*,#13042,.F.);
#17890=ORIENTED_EDGE('',*,*,#13043,.T.);
#17891=ORIENTED_EDGE('',*,*,#13044,.T.);
#17892=ORIENTED_EDGE('',*,*,#13040,.F.);
#17893=ORIENTED_EDGE('',*,*,#13045,.F.);
#17894=ORIENTED_EDGE('',*,*,#13046,.T.);
#17895=ORIENTED_EDGE('',*,*,#13047,.T.);
#17896=ORIENTED_EDGE('',*,*,#13043,.F.);
#17897=ORIENTED_EDGE('',*,*,#13048,.F.);
#17898=ORIENTED_EDGE('',*,*,#13049,.T.);
#17899=ORIENTED_EDGE('',*,*,#13050,.T.);
#17900=ORIENTED_EDGE('',*,*,#13046,.F.);
#17901=ORIENTED_EDGE('',*,*,#13051,.F.);
#17902=ORIENTED_EDGE('',*,*,#13052,.T.);
#17903=ORIENTED_EDGE('',*,*,#13053,.T.);
#17904=ORIENTED_EDGE('',*,*,#13049,.F.);
#17905=ORIENTED_EDGE('',*,*,#13054,.F.);
#17906=ORIENTED_EDGE('',*,*,#13055,.T.);
#17907=ORIENTED_EDGE('',*,*,#13056,.T.);
#17908=ORIENTED_EDGE('',*,*,#13052,.F.);
#17909=ORIENTED_EDGE('',*,*,#13057,.F.);
#17910=ORIENTED_EDGE('',*,*,#13058,.T.);
#17911=ORIENTED_EDGE('',*,*,#13059,.T.);
#17912=ORIENTED_EDGE('',*,*,#13055,.F.);
#17913=ORIENTED_EDGE('',*,*,#13060,.F.);
#17914=ORIENTED_EDGE('',*,*,#13061,.T.);
#17915=ORIENTED_EDGE('',*,*,#13062,.T.);
#17916=ORIENTED_EDGE('',*,*,#13058,.F.);
#17917=ORIENTED_EDGE('',*,*,#13063,.F.);
#17918=ORIENTED_EDGE('',*,*,#13064,.T.);
#17919=ORIENTED_EDGE('',*,*,#13065,.T.);
#17920=ORIENTED_EDGE('',*,*,#13061,.F.);
#17921=ORIENTED_EDGE('',*,*,#13066,.F.);
#17922=ORIENTED_EDGE('',*,*,#13067,.T.);
#17923=ORIENTED_EDGE('',*,*,#13068,.T.);
#17924=ORIENTED_EDGE('',*,*,#13064,.F.);
#17925=ORIENTED_EDGE('',*,*,#13069,.F.);
#17926=ORIENTED_EDGE('',*,*,#13070,.T.);
#17927=ORIENTED_EDGE('',*,*,#13071,.T.);
#17928=ORIENTED_EDGE('',*,*,#13067,.F.);
#17929=ORIENTED_EDGE('',*,*,#13072,.F.);
#17930=ORIENTED_EDGE('',*,*,#13073,.T.);
#17931=ORIENTED_EDGE('',*,*,#13074,.T.);
#17932=ORIENTED_EDGE('',*,*,#13070,.F.);
#17933=ORIENTED_EDGE('',*,*,#13075,.F.);
#17934=ORIENTED_EDGE('',*,*,#13076,.T.);
#17935=ORIENTED_EDGE('',*,*,#13077,.T.);
#17936=ORIENTED_EDGE('',*,*,#13073,.F.);
#17937=ORIENTED_EDGE('',*,*,#13078,.F.);
#17938=ORIENTED_EDGE('',*,*,#13079,.T.);
#17939=ORIENTED_EDGE('',*,*,#13080,.T.);
#17940=ORIENTED_EDGE('',*,*,#13076,.F.);
#17941=ORIENTED_EDGE('',*,*,#13081,.F.);
#17942=ORIENTED_EDGE('',*,*,#13082,.T.);
#17943=ORIENTED_EDGE('',*,*,#13083,.T.);
#17944=ORIENTED_EDGE('',*,*,#13079,.F.);
#17945=ORIENTED_EDGE('',*,*,#13084,.F.);
#17946=ORIENTED_EDGE('',*,*,#13085,.T.);
#17947=ORIENTED_EDGE('',*,*,#13086,.T.);
#17948=ORIENTED_EDGE('',*,*,#13082,.F.);
#17949=ORIENTED_EDGE('',*,*,#13087,.F.);
#17950=ORIENTED_EDGE('',*,*,#13088,.T.);
#17951=ORIENTED_EDGE('',*,*,#13089,.T.);
#17952=ORIENTED_EDGE('',*,*,#13085,.F.);
#17953=ORIENTED_EDGE('',*,*,#13090,.F.);
#17954=ORIENTED_EDGE('',*,*,#13091,.T.);
#17955=ORIENTED_EDGE('',*,*,#13092,.T.);
#17956=ORIENTED_EDGE('',*,*,#13088,.F.);
#17957=ORIENTED_EDGE('',*,*,#13093,.F.);
#17958=ORIENTED_EDGE('',*,*,#13094,.T.);
#17959=ORIENTED_EDGE('',*,*,#13095,.T.);
#17960=ORIENTED_EDGE('',*,*,#13091,.F.);
#17961=ORIENTED_EDGE('',*,*,#13096,.F.);
#17962=ORIENTED_EDGE('',*,*,#13011,.T.);
#17963=ORIENTED_EDGE('',*,*,#13097,.T.);
#17964=ORIENTED_EDGE('',*,*,#13094,.F.);
#17965=ORIENTED_EDGE('',*,*,#13097,.F.);
#17966=ORIENTED_EDGE('',*,*,#13010,.F.);
#17967=ORIENTED_EDGE('',*,*,#13014,.F.);
#17968=ORIENTED_EDGE('',*,*,#13017,.F.);
#17969=ORIENTED_EDGE('',*,*,#13020,.F.);
#17970=ORIENTED_EDGE('',*,*,#13023,.F.);
#17971=ORIENTED_EDGE('',*,*,#13026,.F.);
#17972=ORIENTED_EDGE('',*,*,#13029,.F.);
#17973=ORIENTED_EDGE('',*,*,#13032,.F.);
#17974=ORIENTED_EDGE('',*,*,#13035,.F.);
#17975=ORIENTED_EDGE('',*,*,#13038,.F.);
#17976=ORIENTED_EDGE('',*,*,#13041,.F.);
#17977=ORIENTED_EDGE('',*,*,#13044,.F.);
#17978=ORIENTED_EDGE('',*,*,#13047,.F.);
#17979=ORIENTED_EDGE('',*,*,#13050,.F.);
#17980=ORIENTED_EDGE('',*,*,#13053,.F.);
#17981=ORIENTED_EDGE('',*,*,#13056,.F.);
#17982=ORIENTED_EDGE('',*,*,#13059,.F.);
#17983=ORIENTED_EDGE('',*,*,#13062,.F.);
#17984=ORIENTED_EDGE('',*,*,#13065,.F.);
#17985=ORIENTED_EDGE('',*,*,#13068,.F.);
#17986=ORIENTED_EDGE('',*,*,#13071,.F.);
#17987=ORIENTED_EDGE('',*,*,#13074,.F.);
#17988=ORIENTED_EDGE('',*,*,#13077,.F.);
#17989=ORIENTED_EDGE('',*,*,#13080,.F.);
#17990=ORIENTED_EDGE('',*,*,#13083,.F.);
#17991=ORIENTED_EDGE('',*,*,#13086,.F.);
#17992=ORIENTED_EDGE('',*,*,#13089,.F.);
#17993=ORIENTED_EDGE('',*,*,#13092,.F.);
#17994=ORIENTED_EDGE('',*,*,#13095,.F.);
#17995=ORIENTED_EDGE('',*,*,#13098,.F.);
#17996=ORIENTED_EDGE('',*,*,#13099,.T.);
#17997=ORIENTED_EDGE('',*,*,#13100,.T.);
#17998=ORIENTED_EDGE('',*,*,#13101,.F.);
#17999=ORIENTED_EDGE('',*,*,#13102,.F.);
#18000=ORIENTED_EDGE('',*,*,#13103,.T.);
#18001=ORIENTED_EDGE('',*,*,#13104,.T.);
#18002=ORIENTED_EDGE('',*,*,#13099,.F.);
#18003=ORIENTED_EDGE('',*,*,#13105,.F.);
#18004=ORIENTED_EDGE('',*,*,#13106,.T.);
#18005=ORIENTED_EDGE('',*,*,#13107,.T.);
#18006=ORIENTED_EDGE('',*,*,#13103,.F.);
#18007=ORIENTED_EDGE('',*,*,#13108,.F.);
#18008=ORIENTED_EDGE('',*,*,#13109,.T.);
#18009=ORIENTED_EDGE('',*,*,#13110,.T.);
#18010=ORIENTED_EDGE('',*,*,#13106,.F.);
#18011=ORIENTED_EDGE('',*,*,#13111,.F.);
#18012=ORIENTED_EDGE('',*,*,#13112,.T.);
#18013=ORIENTED_EDGE('',*,*,#13113,.T.);
#18014=ORIENTED_EDGE('',*,*,#13109,.F.);
#18015=ORIENTED_EDGE('',*,*,#13114,.F.);
#18016=ORIENTED_EDGE('',*,*,#13115,.T.);
#18017=ORIENTED_EDGE('',*,*,#13116,.T.);
#18018=ORIENTED_EDGE('',*,*,#13112,.F.);
#18019=ORIENTED_EDGE('',*,*,#13117,.F.);
#18020=ORIENTED_EDGE('',*,*,#13118,.T.);
#18021=ORIENTED_EDGE('',*,*,#13119,.T.);
#18022=ORIENTED_EDGE('',*,*,#13115,.F.);
#18023=ORIENTED_EDGE('',*,*,#13120,.F.);
#18024=ORIENTED_EDGE('',*,*,#13121,.T.);
#18025=ORIENTED_EDGE('',*,*,#13122,.T.);
#18026=ORIENTED_EDGE('',*,*,#13118,.F.);
#18027=ORIENTED_EDGE('',*,*,#13123,.F.);
#18028=ORIENTED_EDGE('',*,*,#13124,.T.);
#18029=ORIENTED_EDGE('',*,*,#13125,.T.);
#18030=ORIENTED_EDGE('',*,*,#13121,.F.);
#18031=ORIENTED_EDGE('',*,*,#13126,.F.);
#18032=ORIENTED_EDGE('',*,*,#13127,.T.);
#18033=ORIENTED_EDGE('',*,*,#13128,.T.);
#18034=ORIENTED_EDGE('',*,*,#13124,.F.);
#18035=ORIENTED_EDGE('',*,*,#13129,.F.);
#18036=ORIENTED_EDGE('',*,*,#13130,.T.);
#18037=ORIENTED_EDGE('',*,*,#13131,.T.);
#18038=ORIENTED_EDGE('',*,*,#13127,.F.);
#18039=ORIENTED_EDGE('',*,*,#13132,.F.);
#18040=ORIENTED_EDGE('',*,*,#13133,.T.);
#18041=ORIENTED_EDGE('',*,*,#13134,.T.);
#18042=ORIENTED_EDGE('',*,*,#13130,.F.);
#18043=ORIENTED_EDGE('',*,*,#13135,.F.);
#18044=ORIENTED_EDGE('',*,*,#13136,.T.);
#18045=ORIENTED_EDGE('',*,*,#13137,.T.);
#18046=ORIENTED_EDGE('',*,*,#13133,.F.);
#18047=ORIENTED_EDGE('',*,*,#13138,.F.);
#18048=ORIENTED_EDGE('',*,*,#13139,.T.);
#18049=ORIENTED_EDGE('',*,*,#13140,.T.);
#18050=ORIENTED_EDGE('',*,*,#13136,.F.);
#18051=ORIENTED_EDGE('',*,*,#13141,.F.);
#18052=ORIENTED_EDGE('',*,*,#13142,.T.);
#18053=ORIENTED_EDGE('',*,*,#13143,.T.);
#18054=ORIENTED_EDGE('',*,*,#13139,.F.);
#18055=ORIENTED_EDGE('',*,*,#13144,.F.);
#18056=ORIENTED_EDGE('',*,*,#13145,.T.);
#18057=ORIENTED_EDGE('',*,*,#13146,.T.);
#18058=ORIENTED_EDGE('',*,*,#13142,.F.);
#18059=ORIENTED_EDGE('',*,*,#13147,.F.);
#18060=ORIENTED_EDGE('',*,*,#13148,.T.);
#18061=ORIENTED_EDGE('',*,*,#13149,.T.);
#18062=ORIENTED_EDGE('',*,*,#13145,.F.);
#18063=ORIENTED_EDGE('',*,*,#13150,.F.);
#18064=ORIENTED_EDGE('',*,*,#13151,.T.);
#18065=ORIENTED_EDGE('',*,*,#13152,.T.);
#18066=ORIENTED_EDGE('',*,*,#13148,.F.);
#18067=ORIENTED_EDGE('',*,*,#13153,.F.);
#18068=ORIENTED_EDGE('',*,*,#13154,.T.);
#18069=ORIENTED_EDGE('',*,*,#13155,.T.);
#18070=ORIENTED_EDGE('',*,*,#13151,.F.);
#18071=ORIENTED_EDGE('',*,*,#13156,.F.);
#18072=ORIENTED_EDGE('',*,*,#13157,.T.);
#18073=ORIENTED_EDGE('',*,*,#13158,.T.);
#18074=ORIENTED_EDGE('',*,*,#13154,.F.);
#18075=ORIENTED_EDGE('',*,*,#13159,.F.);
#18076=ORIENTED_EDGE('',*,*,#13160,.T.);
#18077=ORIENTED_EDGE('',*,*,#13161,.T.);
#18078=ORIENTED_EDGE('',*,*,#13157,.F.);
#18079=ORIENTED_EDGE('',*,*,#13162,.F.);
#18080=ORIENTED_EDGE('',*,*,#13101,.T.);
#18081=ORIENTED_EDGE('',*,*,#13163,.T.);
#18082=ORIENTED_EDGE('',*,*,#13160,.F.);
#18083=ORIENTED_EDGE('',*,*,#13163,.F.);
#18084=ORIENTED_EDGE('',*,*,#13100,.F.);
#18085=ORIENTED_EDGE('',*,*,#13104,.F.);
#18086=ORIENTED_EDGE('',*,*,#13107,.F.);
#18087=ORIENTED_EDGE('',*,*,#13110,.F.);
#18088=ORIENTED_EDGE('',*,*,#13113,.F.);
#18089=ORIENTED_EDGE('',*,*,#13116,.F.);
#18090=ORIENTED_EDGE('',*,*,#13119,.F.);
#18091=ORIENTED_EDGE('',*,*,#13122,.F.);
#18092=ORIENTED_EDGE('',*,*,#13125,.F.);
#18093=ORIENTED_EDGE('',*,*,#13128,.F.);
#18094=ORIENTED_EDGE('',*,*,#13131,.F.);
#18095=ORIENTED_EDGE('',*,*,#13134,.F.);
#18096=ORIENTED_EDGE('',*,*,#13137,.F.);
#18097=ORIENTED_EDGE('',*,*,#13140,.F.);
#18098=ORIENTED_EDGE('',*,*,#13143,.F.);
#18099=ORIENTED_EDGE('',*,*,#13146,.F.);
#18100=ORIENTED_EDGE('',*,*,#13149,.F.);
#18101=ORIENTED_EDGE('',*,*,#13152,.F.);
#18102=ORIENTED_EDGE('',*,*,#13155,.F.);
#18103=ORIENTED_EDGE('',*,*,#13158,.F.);
#18104=ORIENTED_EDGE('',*,*,#13161,.F.);
#18105=ORIENTED_EDGE('',*,*,#13164,.F.);
#18106=ORIENTED_EDGE('',*,*,#13165,.T.);
#18107=ORIENTED_EDGE('',*,*,#13166,.T.);
#18108=ORIENTED_EDGE('',*,*,#13167,.F.);
#18109=ORIENTED_EDGE('',*,*,#13168,.F.);
#18110=ORIENTED_EDGE('',*,*,#13169,.T.);
#18111=ORIENTED_EDGE('',*,*,#13170,.T.);
#18112=ORIENTED_EDGE('',*,*,#13165,.F.);
#18113=ORIENTED_EDGE('',*,*,#13171,.F.);
#18114=ORIENTED_EDGE('',*,*,#13172,.T.);
#18115=ORIENTED_EDGE('',*,*,#13173,.T.);
#18116=ORIENTED_EDGE('',*,*,#13169,.F.);
#18117=ORIENTED_EDGE('',*,*,#13174,.F.);
#18118=ORIENTED_EDGE('',*,*,#13175,.T.);
#18119=ORIENTED_EDGE('',*,*,#13176,.T.);
#18120=ORIENTED_EDGE('',*,*,#13172,.F.);
#18121=ORIENTED_EDGE('',*,*,#13177,.F.);
#18122=ORIENTED_EDGE('',*,*,#13178,.T.);
#18123=ORIENTED_EDGE('',*,*,#13179,.T.);
#18124=ORIENTED_EDGE('',*,*,#13175,.F.);
#18125=ORIENTED_EDGE('',*,*,#13180,.F.);
#18126=ORIENTED_EDGE('',*,*,#13181,.T.);
#18127=ORIENTED_EDGE('',*,*,#13182,.T.);
#18128=ORIENTED_EDGE('',*,*,#13178,.F.);
#18129=ORIENTED_EDGE('',*,*,#13183,.F.);
#18130=ORIENTED_EDGE('',*,*,#13184,.T.);
#18131=ORIENTED_EDGE('',*,*,#13185,.T.);
#18132=ORIENTED_EDGE('',*,*,#13181,.F.);
#18133=ORIENTED_EDGE('',*,*,#13186,.F.);
#18134=ORIENTED_EDGE('',*,*,#13167,.T.);
#18135=ORIENTED_EDGE('',*,*,#13187,.T.);
#18136=ORIENTED_EDGE('',*,*,#13184,.F.);
#18137=ORIENTED_EDGE('',*,*,#13188,.F.);
#18138=ORIENTED_EDGE('',*,*,#13189,.T.);
#18139=ORIENTED_EDGE('',*,*,#13190,.T.);
#18140=ORIENTED_EDGE('',*,*,#13191,.F.);
#18141=ORIENTED_EDGE('',*,*,#13192,.F.);
#18142=ORIENTED_EDGE('',*,*,#13193,.T.);
#18143=ORIENTED_EDGE('',*,*,#13194,.T.);
#18144=ORIENTED_EDGE('',*,*,#13189,.F.);
#18145=ORIENTED_EDGE('',*,*,#13195,.F.);
#18146=ORIENTED_EDGE('',*,*,#13196,.T.);
#18147=ORIENTED_EDGE('',*,*,#13197,.T.);
#18148=ORIENTED_EDGE('',*,*,#13193,.F.);
#18149=ORIENTED_EDGE('',*,*,#13198,.F.);
#18150=ORIENTED_EDGE('',*,*,#13199,.T.);
#18151=ORIENTED_EDGE('',*,*,#13200,.T.);
#18152=ORIENTED_EDGE('',*,*,#13196,.F.);
#18153=ORIENTED_EDGE('',*,*,#13201,.F.);
#18154=ORIENTED_EDGE('',*,*,#13202,.T.);
#18155=ORIENTED_EDGE('',*,*,#13203,.T.);
#18156=ORIENTED_EDGE('',*,*,#13199,.F.);
#18157=ORIENTED_EDGE('',*,*,#13204,.F.);
#18158=ORIENTED_EDGE('',*,*,#13205,.T.);
#18159=ORIENTED_EDGE('',*,*,#13206,.T.);
#18160=ORIENTED_EDGE('',*,*,#13202,.F.);
#18161=ORIENTED_EDGE('',*,*,#13207,.F.);
#18162=ORIENTED_EDGE('',*,*,#13208,.T.);
#18163=ORIENTED_EDGE('',*,*,#13209,.T.);
#18164=ORIENTED_EDGE('',*,*,#13205,.F.);
#18165=ORIENTED_EDGE('',*,*,#13210,.F.);
#18166=ORIENTED_EDGE('',*,*,#13211,.T.);
#18167=ORIENTED_EDGE('',*,*,#13212,.T.);
#18168=ORIENTED_EDGE('',*,*,#13208,.F.);
#18169=ORIENTED_EDGE('',*,*,#13213,.F.);
#18170=ORIENTED_EDGE('',*,*,#13214,.T.);
#18171=ORIENTED_EDGE('',*,*,#13215,.T.);
#18172=ORIENTED_EDGE('',*,*,#13211,.F.);
#18173=ORIENTED_EDGE('',*,*,#13216,.F.);
#18174=ORIENTED_EDGE('',*,*,#13217,.T.);
#18175=ORIENTED_EDGE('',*,*,#13218,.T.);
#18176=ORIENTED_EDGE('',*,*,#13214,.F.);
#18177=ORIENTED_EDGE('',*,*,#13219,.F.);
#18178=ORIENTED_EDGE('',*,*,#13191,.T.);
#18179=ORIENTED_EDGE('',*,*,#13220,.T.);
#18180=ORIENTED_EDGE('',*,*,#13217,.F.);
#18181=ORIENTED_EDGE('',*,*,#13220,.F.);
#18182=ORIENTED_EDGE('',*,*,#13190,.F.);
#18183=ORIENTED_EDGE('',*,*,#13194,.F.);
#18184=ORIENTED_EDGE('',*,*,#13197,.F.);
#18185=ORIENTED_EDGE('',*,*,#13200,.F.);
#18186=ORIENTED_EDGE('',*,*,#13203,.F.);
#18187=ORIENTED_EDGE('',*,*,#13206,.F.);
#18188=ORIENTED_EDGE('',*,*,#13209,.F.);
#18189=ORIENTED_EDGE('',*,*,#13212,.F.);
#18190=ORIENTED_EDGE('',*,*,#13215,.F.);
#18191=ORIENTED_EDGE('',*,*,#13218,.F.);
#18192=ORIENTED_EDGE('',*,*,#13187,.F.);
#18193=ORIENTED_EDGE('',*,*,#13166,.F.);
#18194=ORIENTED_EDGE('',*,*,#13170,.F.);
#18195=ORIENTED_EDGE('',*,*,#13173,.F.);
#18196=ORIENTED_EDGE('',*,*,#13176,.F.);
#18197=ORIENTED_EDGE('',*,*,#13179,.F.);
#18198=ORIENTED_EDGE('',*,*,#13182,.F.);
#18199=ORIENTED_EDGE('',*,*,#13185,.F.);
#18200=ORIENTED_EDGE('',*,*,#13221,.F.);
#18201=ORIENTED_EDGE('',*,*,#13222,.T.);
#18202=ORIENTED_EDGE('',*,*,#13223,.T.);
#18203=ORIENTED_EDGE('',*,*,#13224,.F.);
#18204=ORIENTED_EDGE('',*,*,#13225,.F.);
#18205=ORIENTED_EDGE('',*,*,#13226,.T.);
#18206=ORIENTED_EDGE('',*,*,#13227,.T.);
#18207=ORIENTED_EDGE('',*,*,#13222,.F.);
#18208=ORIENTED_EDGE('',*,*,#13228,.F.);
#18209=ORIENTED_EDGE('',*,*,#13229,.T.);
#18210=ORIENTED_EDGE('',*,*,#13230,.T.);
#18211=ORIENTED_EDGE('',*,*,#13226,.F.);
#18212=ORIENTED_EDGE('',*,*,#13231,.F.);
#18213=ORIENTED_EDGE('',*,*,#13232,.T.);
#18214=ORIENTED_EDGE('',*,*,#13233,.T.);
#18215=ORIENTED_EDGE('',*,*,#13229,.F.);
#18216=ORIENTED_EDGE('',*,*,#13234,.F.);
#18217=ORIENTED_EDGE('',*,*,#13235,.T.);
#18218=ORIENTED_EDGE('',*,*,#13236,.T.);
#18219=ORIENTED_EDGE('',*,*,#13232,.F.);
#18220=ORIENTED_EDGE('',*,*,#13237,.F.);
#18221=ORIENTED_EDGE('',*,*,#13238,.T.);
#18222=ORIENTED_EDGE('',*,*,#13239,.T.);
#18223=ORIENTED_EDGE('',*,*,#13235,.F.);
#18224=ORIENTED_EDGE('',*,*,#13240,.F.);
#18225=ORIENTED_EDGE('',*,*,#13241,.T.);
#18226=ORIENTED_EDGE('',*,*,#13242,.T.);
#18227=ORIENTED_EDGE('',*,*,#13238,.F.);
#18228=ORIENTED_EDGE('',*,*,#13243,.F.);
#18229=ORIENTED_EDGE('',*,*,#13244,.T.);
#18230=ORIENTED_EDGE('',*,*,#13245,.T.);
#18231=ORIENTED_EDGE('',*,*,#13241,.F.);
#18232=ORIENTED_EDGE('',*,*,#13246,.F.);
#18233=ORIENTED_EDGE('',*,*,#13224,.T.);
#18234=ORIENTED_EDGE('',*,*,#13247,.T.);
#18235=ORIENTED_EDGE('',*,*,#13244,.F.);
#18236=ORIENTED_EDGE('',*,*,#13248,.F.);
#18237=ORIENTED_EDGE('',*,*,#13249,.T.);
#18238=ORIENTED_EDGE('',*,*,#13250,.T.);
#18239=ORIENTED_EDGE('',*,*,#13251,.F.);
#18240=ORIENTED_EDGE('',*,*,#13252,.F.);
#18241=ORIENTED_EDGE('',*,*,#13253,.T.);
#18242=ORIENTED_EDGE('',*,*,#13254,.T.);
#18243=ORIENTED_EDGE('',*,*,#13249,.F.);
#18244=ORIENTED_EDGE('',*,*,#13255,.F.);
#18245=ORIENTED_EDGE('',*,*,#13256,.T.);
#18246=ORIENTED_EDGE('',*,*,#13257,.T.);
#18247=ORIENTED_EDGE('',*,*,#13253,.F.);
#18248=ORIENTED_EDGE('',*,*,#13258,.F.);
#18249=ORIENTED_EDGE('',*,*,#13259,.T.);
#18250=ORIENTED_EDGE('',*,*,#13260,.T.);
#18251=ORIENTED_EDGE('',*,*,#13256,.F.);
#18252=ORIENTED_EDGE('',*,*,#13261,.F.);
#18253=ORIENTED_EDGE('',*,*,#13262,.T.);
#18254=ORIENTED_EDGE('',*,*,#13263,.T.);
#18255=ORIENTED_EDGE('',*,*,#13259,.F.);
#18256=ORIENTED_EDGE('',*,*,#13264,.F.);
#18257=ORIENTED_EDGE('',*,*,#13265,.T.);
#18258=ORIENTED_EDGE('',*,*,#13266,.T.);
#18259=ORIENTED_EDGE('',*,*,#13262,.F.);
#18260=ORIENTED_EDGE('',*,*,#13267,.F.);
#18261=ORIENTED_EDGE('',*,*,#13268,.T.);
#18262=ORIENTED_EDGE('',*,*,#13269,.T.);
#18263=ORIENTED_EDGE('',*,*,#13265,.F.);
#18264=ORIENTED_EDGE('',*,*,#13270,.F.);
#18265=ORIENTED_EDGE('',*,*,#13271,.T.);
#18266=ORIENTED_EDGE('',*,*,#13272,.T.);
#18267=ORIENTED_EDGE('',*,*,#13268,.F.);
#18268=ORIENTED_EDGE('',*,*,#13273,.F.);
#18269=ORIENTED_EDGE('',*,*,#13274,.T.);
#18270=ORIENTED_EDGE('',*,*,#13275,.T.);
#18271=ORIENTED_EDGE('',*,*,#13271,.F.);
#18272=ORIENTED_EDGE('',*,*,#13276,.F.);
#18273=ORIENTED_EDGE('',*,*,#13277,.T.);
#18274=ORIENTED_EDGE('',*,*,#13278,.T.);
#18275=ORIENTED_EDGE('',*,*,#13274,.F.);
#18276=ORIENTED_EDGE('',*,*,#13279,.F.);
#18277=ORIENTED_EDGE('',*,*,#13280,.T.);
#18278=ORIENTED_EDGE('',*,*,#13281,.T.);
#18279=ORIENTED_EDGE('',*,*,#13277,.F.);
#18280=ORIENTED_EDGE('',*,*,#13282,.F.);
#18281=ORIENTED_EDGE('',*,*,#13283,.T.);
#18282=ORIENTED_EDGE('',*,*,#13284,.T.);
#18283=ORIENTED_EDGE('',*,*,#13280,.F.);
#18284=ORIENTED_EDGE('',*,*,#13285,.F.);
#18285=ORIENTED_EDGE('',*,*,#13286,.T.);
#18286=ORIENTED_EDGE('',*,*,#13287,.T.);
#18287=ORIENTED_EDGE('',*,*,#13283,.F.);
#18288=ORIENTED_EDGE('',*,*,#13288,.F.);
#18289=ORIENTED_EDGE('',*,*,#13289,.T.);
#18290=ORIENTED_EDGE('',*,*,#13290,.T.);
#18291=ORIENTED_EDGE('',*,*,#13286,.F.);
#18292=ORIENTED_EDGE('',*,*,#13291,.F.);
#18293=ORIENTED_EDGE('',*,*,#13292,.T.);
#18294=ORIENTED_EDGE('',*,*,#13293,.T.);
#18295=ORIENTED_EDGE('',*,*,#13289,.F.);
#18296=ORIENTED_EDGE('',*,*,#13294,.F.);
#18297=ORIENTED_EDGE('',*,*,#13295,.T.);
#18298=ORIENTED_EDGE('',*,*,#13296,.T.);
#18299=ORIENTED_EDGE('',*,*,#13292,.F.);
#18300=ORIENTED_EDGE('',*,*,#13297,.F.);
#18301=ORIENTED_EDGE('',*,*,#13298,.T.);
#18302=ORIENTED_EDGE('',*,*,#13299,.T.);
#18303=ORIENTED_EDGE('',*,*,#13295,.F.);
#18304=ORIENTED_EDGE('',*,*,#13300,.F.);
#18305=ORIENTED_EDGE('',*,*,#13301,.T.);
#18306=ORIENTED_EDGE('',*,*,#13302,.T.);
#18307=ORIENTED_EDGE('',*,*,#13298,.F.);
#18308=ORIENTED_EDGE('',*,*,#13303,.F.);
#18309=ORIENTED_EDGE('',*,*,#13251,.T.);
#18310=ORIENTED_EDGE('',*,*,#13304,.T.);
#18311=ORIENTED_EDGE('',*,*,#13301,.F.);
#18312=ORIENTED_EDGE('',*,*,#13304,.F.);
#18313=ORIENTED_EDGE('',*,*,#13250,.F.);
#18314=ORIENTED_EDGE('',*,*,#13254,.F.);
#18315=ORIENTED_EDGE('',*,*,#13257,.F.);
#18316=ORIENTED_EDGE('',*,*,#13260,.F.);
#18317=ORIENTED_EDGE('',*,*,#13263,.F.);
#18318=ORIENTED_EDGE('',*,*,#13266,.F.);
#18319=ORIENTED_EDGE('',*,*,#13269,.F.);
#18320=ORIENTED_EDGE('',*,*,#13272,.F.);
#18321=ORIENTED_EDGE('',*,*,#13275,.F.);
#18322=ORIENTED_EDGE('',*,*,#13278,.F.);
#18323=ORIENTED_EDGE('',*,*,#13281,.F.);
#18324=ORIENTED_EDGE('',*,*,#13284,.F.);
#18325=ORIENTED_EDGE('',*,*,#13287,.F.);
#18326=ORIENTED_EDGE('',*,*,#13290,.F.);
#18327=ORIENTED_EDGE('',*,*,#13293,.F.);
#18328=ORIENTED_EDGE('',*,*,#13296,.F.);
#18329=ORIENTED_EDGE('',*,*,#13299,.F.);
#18330=ORIENTED_EDGE('',*,*,#13302,.F.);
#18331=ORIENTED_EDGE('',*,*,#13247,.F.);
#18332=ORIENTED_EDGE('',*,*,#13223,.F.);
#18333=ORIENTED_EDGE('',*,*,#13227,.F.);
#18334=ORIENTED_EDGE('',*,*,#13230,.F.);
#18335=ORIENTED_EDGE('',*,*,#13233,.F.);
#18336=ORIENTED_EDGE('',*,*,#13236,.F.);
#18337=ORIENTED_EDGE('',*,*,#13239,.F.);
#18338=ORIENTED_EDGE('',*,*,#13242,.F.);
#18339=ORIENTED_EDGE('',*,*,#13245,.F.);
#18340=ORIENTED_EDGE('',*,*,#13305,.F.);
#18341=ORIENTED_EDGE('',*,*,#13306,.T.);
#18342=ORIENTED_EDGE('',*,*,#13307,.T.);
#18343=ORIENTED_EDGE('',*,*,#13308,.F.);
#18344=ORIENTED_EDGE('',*,*,#13309,.F.);
#18345=ORIENTED_EDGE('',*,*,#13310,.T.);
#18346=ORIENTED_EDGE('',*,*,#13311,.T.);
#18347=ORIENTED_EDGE('',*,*,#13306,.F.);
#18348=ORIENTED_EDGE('',*,*,#13312,.F.);
#18349=ORIENTED_EDGE('',*,*,#13313,.T.);
#18350=ORIENTED_EDGE('',*,*,#13314,.T.);
#18351=ORIENTED_EDGE('',*,*,#13310,.F.);
#18352=ORIENTED_EDGE('',*,*,#13315,.F.);
#18353=ORIENTED_EDGE('',*,*,#13316,.T.);
#18354=ORIENTED_EDGE('',*,*,#13317,.T.);
#18355=ORIENTED_EDGE('',*,*,#13313,.F.);
#18356=ORIENTED_EDGE('',*,*,#13318,.F.);
#18357=ORIENTED_EDGE('',*,*,#13319,.T.);
#18358=ORIENTED_EDGE('',*,*,#13320,.T.);
#18359=ORIENTED_EDGE('',*,*,#13316,.F.);
#18360=ORIENTED_EDGE('',*,*,#13321,.F.);
#18361=ORIENTED_EDGE('',*,*,#13322,.T.);
#18362=ORIENTED_EDGE('',*,*,#13323,.T.);
#18363=ORIENTED_EDGE('',*,*,#13319,.F.);
#18364=ORIENTED_EDGE('',*,*,#13324,.F.);
#18365=ORIENTED_EDGE('',*,*,#13325,.T.);
#18366=ORIENTED_EDGE('',*,*,#13326,.T.);
#18367=ORIENTED_EDGE('',*,*,#13322,.F.);
#18368=ORIENTED_EDGE('',*,*,#13327,.F.);
#18369=ORIENTED_EDGE('',*,*,#13308,.T.);
#18370=ORIENTED_EDGE('',*,*,#13328,.T.);
#18371=ORIENTED_EDGE('',*,*,#13325,.F.);
#18372=ORIENTED_EDGE('',*,*,#13329,.F.);
#18373=ORIENTED_EDGE('',*,*,#13330,.T.);
#18374=ORIENTED_EDGE('',*,*,#13331,.T.);
#18375=ORIENTED_EDGE('',*,*,#13332,.F.);
#18376=ORIENTED_EDGE('',*,*,#13333,.F.);
#18377=ORIENTED_EDGE('',*,*,#13334,.T.);
#18378=ORIENTED_EDGE('',*,*,#13335,.T.);
#18379=ORIENTED_EDGE('',*,*,#13330,.F.);
#18380=ORIENTED_EDGE('',*,*,#13336,.F.);
#18381=ORIENTED_EDGE('',*,*,#13337,.T.);
#18382=ORIENTED_EDGE('',*,*,#13338,.T.);
#18383=ORIENTED_EDGE('',*,*,#13334,.F.);
#18384=ORIENTED_EDGE('',*,*,#13339,.F.);
#18385=ORIENTED_EDGE('',*,*,#13340,.T.);
#18386=ORIENTED_EDGE('',*,*,#13341,.T.);
#18387=ORIENTED_EDGE('',*,*,#13337,.F.);
#18388=ORIENTED_EDGE('',*,*,#13342,.F.);
#18389=ORIENTED_EDGE('',*,*,#13343,.T.);
#18390=ORIENTED_EDGE('',*,*,#13344,.T.);
#18391=ORIENTED_EDGE('',*,*,#13340,.F.);
#18392=ORIENTED_EDGE('',*,*,#13345,.F.);
#18393=ORIENTED_EDGE('',*,*,#13346,.T.);
#18394=ORIENTED_EDGE('',*,*,#13347,.T.);
#18395=ORIENTED_EDGE('',*,*,#13343,.F.);
#18396=ORIENTED_EDGE('',*,*,#13348,.F.);
#18397=ORIENTED_EDGE('',*,*,#13349,.T.);
#18398=ORIENTED_EDGE('',*,*,#13350,.T.);
#18399=ORIENTED_EDGE('',*,*,#13346,.F.);
#18400=ORIENTED_EDGE('',*,*,#13351,.F.);
#18401=ORIENTED_EDGE('',*,*,#13352,.T.);
#18402=ORIENTED_EDGE('',*,*,#13353,.T.);
#18403=ORIENTED_EDGE('',*,*,#13349,.F.);
#18404=ORIENTED_EDGE('',*,*,#13354,.F.);
#18405=ORIENTED_EDGE('',*,*,#13355,.T.);
#18406=ORIENTED_EDGE('',*,*,#13356,.T.);
#18407=ORIENTED_EDGE('',*,*,#13352,.F.);
#18408=ORIENTED_EDGE('',*,*,#13357,.F.);
#18409=ORIENTED_EDGE('',*,*,#13358,.T.);
#18410=ORIENTED_EDGE('',*,*,#13359,.T.);
#18411=ORIENTED_EDGE('',*,*,#13355,.F.);
#18412=ORIENTED_EDGE('',*,*,#13360,.F.);
#18413=ORIENTED_EDGE('',*,*,#13361,.T.);
#18414=ORIENTED_EDGE('',*,*,#13362,.T.);
#18415=ORIENTED_EDGE('',*,*,#13358,.F.);
#18416=ORIENTED_EDGE('',*,*,#13363,.F.);
#18417=ORIENTED_EDGE('',*,*,#13364,.T.);
#18418=ORIENTED_EDGE('',*,*,#13365,.T.);
#18419=ORIENTED_EDGE('',*,*,#13361,.F.);
#18420=ORIENTED_EDGE('',*,*,#13366,.F.);
#18421=ORIENTED_EDGE('',*,*,#13332,.T.);
#18422=ORIENTED_EDGE('',*,*,#13367,.T.);
#18423=ORIENTED_EDGE('',*,*,#13364,.F.);
#18424=ORIENTED_EDGE('',*,*,#13367,.F.);
#18425=ORIENTED_EDGE('',*,*,#13331,.F.);
#18426=ORIENTED_EDGE('',*,*,#13335,.F.);
#18427=ORIENTED_EDGE('',*,*,#13338,.F.);
#18428=ORIENTED_EDGE('',*,*,#13341,.F.);
#18429=ORIENTED_EDGE('',*,*,#13344,.F.);
#18430=ORIENTED_EDGE('',*,*,#13347,.F.);
#18431=ORIENTED_EDGE('',*,*,#13350,.F.);
#18432=ORIENTED_EDGE('',*,*,#13353,.F.);
#18433=ORIENTED_EDGE('',*,*,#13356,.F.);
#18434=ORIENTED_EDGE('',*,*,#13359,.F.);
#18435=ORIENTED_EDGE('',*,*,#13362,.F.);
#18436=ORIENTED_EDGE('',*,*,#13365,.F.);
#18437=ORIENTED_EDGE('',*,*,#13328,.F.);
#18438=ORIENTED_EDGE('',*,*,#13307,.F.);
#18439=ORIENTED_EDGE('',*,*,#13311,.F.);
#18440=ORIENTED_EDGE('',*,*,#13314,.F.);
#18441=ORIENTED_EDGE('',*,*,#13317,.F.);
#18442=ORIENTED_EDGE('',*,*,#13320,.F.);
#18443=ORIENTED_EDGE('',*,*,#13323,.F.);
#18444=ORIENTED_EDGE('',*,*,#13326,.F.);
#18445=ORIENTED_EDGE('',*,*,#13368,.F.);
#18446=ORIENTED_EDGE('',*,*,#13369,.T.);
#18447=ORIENTED_EDGE('',*,*,#13370,.T.);
#18448=ORIENTED_EDGE('',*,*,#13371,.F.);
#18449=ORIENTED_EDGE('',*,*,#13372,.F.);
#18450=ORIENTED_EDGE('',*,*,#13373,.T.);
#18451=ORIENTED_EDGE('',*,*,#13374,.T.);
#18452=ORIENTED_EDGE('',*,*,#13369,.F.);
#18453=ORIENTED_EDGE('',*,*,#13375,.F.);
#18454=ORIENTED_EDGE('',*,*,#13376,.T.);
#18455=ORIENTED_EDGE('',*,*,#13377,.T.);
#18456=ORIENTED_EDGE('',*,*,#13373,.F.);
#18457=ORIENTED_EDGE('',*,*,#13378,.F.);
#18458=ORIENTED_EDGE('',*,*,#13379,.T.);
#18459=ORIENTED_EDGE('',*,*,#13380,.T.);
#18460=ORIENTED_EDGE('',*,*,#13376,.F.);
#18461=ORIENTED_EDGE('',*,*,#13381,.F.);
#18462=ORIENTED_EDGE('',*,*,#13382,.T.);
#18463=ORIENTED_EDGE('',*,*,#13383,.T.);
#18464=ORIENTED_EDGE('',*,*,#13379,.F.);
#18465=ORIENTED_EDGE('',*,*,#13384,.F.);
#18466=ORIENTED_EDGE('',*,*,#13385,.T.);
#18467=ORIENTED_EDGE('',*,*,#13386,.T.);
#18468=ORIENTED_EDGE('',*,*,#13382,.F.);
#18469=ORIENTED_EDGE('',*,*,#13387,.F.);
#18470=ORIENTED_EDGE('',*,*,#13388,.T.);
#18471=ORIENTED_EDGE('',*,*,#13389,.T.);
#18472=ORIENTED_EDGE('',*,*,#13385,.F.);
#18473=ORIENTED_EDGE('',*,*,#13390,.F.);
#18474=ORIENTED_EDGE('',*,*,#13391,.T.);
#18475=ORIENTED_EDGE('',*,*,#13392,.T.);
#18476=ORIENTED_EDGE('',*,*,#13388,.F.);
#18477=ORIENTED_EDGE('',*,*,#13393,.F.);
#18478=ORIENTED_EDGE('',*,*,#13394,.T.);
#18479=ORIENTED_EDGE('',*,*,#13395,.T.);
#18480=ORIENTED_EDGE('',*,*,#13391,.F.);
#18481=ORIENTED_EDGE('',*,*,#13396,.F.);
#18482=ORIENTED_EDGE('',*,*,#13397,.T.);
#18483=ORIENTED_EDGE('',*,*,#13398,.T.);
#18484=ORIENTED_EDGE('',*,*,#13394,.F.);
#18485=ORIENTED_EDGE('',*,*,#13399,.F.);
#18486=ORIENTED_EDGE('',*,*,#13400,.T.);
#18487=ORIENTED_EDGE('',*,*,#13401,.T.);
#18488=ORIENTED_EDGE('',*,*,#13397,.F.);
#18489=ORIENTED_EDGE('',*,*,#13402,.F.);
#18490=ORIENTED_EDGE('',*,*,#13403,.T.);
#18491=ORIENTED_EDGE('',*,*,#13404,.T.);
#18492=ORIENTED_EDGE('',*,*,#13400,.F.);
#18493=ORIENTED_EDGE('',*,*,#13405,.F.);
#18494=ORIENTED_EDGE('',*,*,#13371,.T.);
#18495=ORIENTED_EDGE('',*,*,#13406,.T.);
#18496=ORIENTED_EDGE('',*,*,#13403,.F.);
#18497=ORIENTED_EDGE('',*,*,#13406,.F.);
#18498=ORIENTED_EDGE('',*,*,#13370,.F.);
#18499=ORIENTED_EDGE('',*,*,#13374,.F.);
#18500=ORIENTED_EDGE('',*,*,#13377,.F.);
#18501=ORIENTED_EDGE('',*,*,#13380,.F.);
#18502=ORIENTED_EDGE('',*,*,#13383,.F.);
#18503=ORIENTED_EDGE('',*,*,#13386,.F.);
#18504=ORIENTED_EDGE('',*,*,#13389,.F.);
#18505=ORIENTED_EDGE('',*,*,#13392,.F.);
#18506=ORIENTED_EDGE('',*,*,#13395,.F.);
#18507=ORIENTED_EDGE('',*,*,#13398,.F.);
#18508=ORIENTED_EDGE('',*,*,#13401,.F.);
#18509=ORIENTED_EDGE('',*,*,#13404,.F.);
#18510=ORIENTED_EDGE('',*,*,#13305,.T.);
#18511=ORIENTED_EDGE('',*,*,#13327,.T.);
#18512=ORIENTED_EDGE('',*,*,#13324,.T.);
#18513=ORIENTED_EDGE('',*,*,#13321,.T.);
#18514=ORIENTED_EDGE('',*,*,#13318,.T.);
#18515=ORIENTED_EDGE('',*,*,#13315,.T.);
#18516=ORIENTED_EDGE('',*,*,#13312,.T.);
#18517=ORIENTED_EDGE('',*,*,#13309,.T.);
#18518=ORIENTED_EDGE('',*,*,#13221,.T.);
#18519=ORIENTED_EDGE('',*,*,#13246,.T.);
#18520=ORIENTED_EDGE('',*,*,#13243,.T.);
#18521=ORIENTED_EDGE('',*,*,#13240,.T.);
#18522=ORIENTED_EDGE('',*,*,#13237,.T.);
#18523=ORIENTED_EDGE('',*,*,#13234,.T.);
#18524=ORIENTED_EDGE('',*,*,#13231,.T.);
#18525=ORIENTED_EDGE('',*,*,#13228,.T.);
#18526=ORIENTED_EDGE('',*,*,#13225,.T.);
#18527=ORIENTED_EDGE('',*,*,#13164,.T.);
#18528=ORIENTED_EDGE('',*,*,#13186,.T.);
#18529=ORIENTED_EDGE('',*,*,#13183,.T.);
#18530=ORIENTED_EDGE('',*,*,#13180,.T.);
#18531=ORIENTED_EDGE('',*,*,#13177,.T.);
#18532=ORIENTED_EDGE('',*,*,#13174,.T.);
#18533=ORIENTED_EDGE('',*,*,#13171,.T.);
#18534=ORIENTED_EDGE('',*,*,#13168,.T.);
#18535=ORIENTED_EDGE('',*,*,#12864,.T.);
#18536=ORIENTED_EDGE('',*,*,#12877,.T.);
#18537=ORIENTED_EDGE('',*,*,#12874,.T.);
#18538=ORIENTED_EDGE('',*,*,#12871,.T.);
#18539=ORIENTED_EDGE('',*,*,#12868,.T.);
#18540=ORIENTED_EDGE('',*,*,#12630,.T.);
#18541=ORIENTED_EDGE('',*,*,#12652,.T.);
#18542=ORIENTED_EDGE('',*,*,#12649,.T.);
#18543=ORIENTED_EDGE('',*,*,#12646,.T.);
#18544=ORIENTED_EDGE('',*,*,#12643,.T.);
#18545=ORIENTED_EDGE('',*,*,#12640,.T.);
#18546=ORIENTED_EDGE('',*,*,#12637,.T.);
#18547=ORIENTED_EDGE('',*,*,#12634,.T.);
#18548=ORIENTED_EDGE('',*,*,#12519,.T.);
#18549=ORIENTED_EDGE('',*,*,#12547,.T.);
#18550=ORIENTED_EDGE('',*,*,#12544,.T.);
#18551=ORIENTED_EDGE('',*,*,#12541,.T.);
#18552=ORIENTED_EDGE('',*,*,#12538,.T.);
#18553=ORIENTED_EDGE('',*,*,#12535,.T.);
#18554=ORIENTED_EDGE('',*,*,#12532,.T.);
#18555=ORIENTED_EDGE('',*,*,#12529,.T.);
#18556=ORIENTED_EDGE('',*,*,#12526,.T.);
#18557=ORIENTED_EDGE('',*,*,#12523,.T.);
#18558=ORIENTED_EDGE('',*,*,#13407,.F.);
#18559=ORIENTED_EDGE('',*,*,#13408,.T.);
#18560=ORIENTED_EDGE('',*,*,#13409,.F.);
#18561=ORIENTED_EDGE('',*,*,#13410,.F.);
#18562=ORIENTED_EDGE('',*,*,#13411,.F.);
#18563=ORIENTED_EDGE('',*,*,#13412,.F.);
#18564=ORIENTED_EDGE('',*,*,#13408,.F.);
#18565=ORIENTED_EDGE('',*,*,#13413,.T.);
#18566=ORIENTED_EDGE('',*,*,#13414,.T.);
#18567=ORIENTED_EDGE('',*,*,#13415,.T.);
#18568=ORIENTED_EDGE('',*,*,#13414,.F.);
#18569=ORIENTED_EDGE('',*,*,#13416,.F.);
#18570=ORIENTED_EDGE('',*,*,#13417,.T.);
#18571=ORIENTED_EDGE('',*,*,#13415,.F.);
#18572=ORIENTED_EDGE('',*,*,#13417,.F.);
#18573=ORIENTED_EDGE('',*,*,#13418,.F.);
#18574=ORIENTED_EDGE('',*,*,#13419,.F.);
#18575=ORIENTED_EDGE('',*,*,#13420,.F.);
#18576=ORIENTED_EDGE('',*,*,#13421,.F.);
#18577=ORIENTED_EDGE('',*,*,#13413,.F.);
#18578=ORIENTED_EDGE('',*,*,#13422,.T.);
#18579=ORIENTED_EDGE('',*,*,#13423,.T.);
#18580=ORIENTED_EDGE('',*,*,#13422,.F.);
#18581=ORIENTED_EDGE('',*,*,#13423,.F.);
#18582=ORIENTED_EDGE('',*,*,#13424,.T.);
#18583=ORIENTED_EDGE('',*,*,#13409,.T.);
#18584=ORIENTED_EDGE('',*,*,#13412,.T.);
#18585=ORIENTED_EDGE('',*,*,#13425,.T.);
#18586=ORIENTED_EDGE('',*,*,#13426,.T.);
#18587=ORIENTED_EDGE('',*,*,#13425,.F.);
#18588=ORIENTED_EDGE('',*,*,#13411,.T.);
#18589=ORIENTED_EDGE('',*,*,#13410,.T.);
#18590=ORIENTED_EDGE('',*,*,#13424,.F.);
#18591=ORIENTED_EDGE('',*,*,#13416,.T.);
#18592=ORIENTED_EDGE('',*,*,#13426,.F.);
#18593=ORIENTED_EDGE('',*,*,#13427,.F.);
#18594=ORIENTED_EDGE('',*,*,#13421,.T.);
#18595=ORIENTED_EDGE('',*,*,#13418,.T.);
#18596=ORIENTED_EDGE('',*,*,#13427,.T.);
#18597=ORIENTED_EDGE('',*,*,#13420,.T.);
#18598=ORIENTED_EDGE('',*,*,#13428,.F.);
#18599=ORIENTED_EDGE('',*,*,#13429,.T.);
#18600=ORIENTED_EDGE('',*,*,#13430,.T.);
#18601=ORIENTED_EDGE('',*,*,#13429,.F.);
#18602=ORIENTED_EDGE('',*,*,#13431,.F.);
#18603=ORIENTED_EDGE('',*,*,#13432,.T.);
#18604=ORIENTED_EDGE('',*,*,#13433,.T.);
#18605=ORIENTED_EDGE('',*,*,#13428,.T.);
#18606=ORIENTED_EDGE('',*,*,#13419,.T.);
#18607=ORIENTED_EDGE('',*,*,#13431,.T.);
#18608=ORIENTED_EDGE('',*,*,#13433,.F.);
#18609=ORIENTED_EDGE('',*,*,#13434,.T.);
#18610=ORIENTED_EDGE('',*,*,#13435,.T.);
#18611=ORIENTED_EDGE('',*,*,#13436,.T.);
#18612=ORIENTED_EDGE('',*,*,#13435,.F.);
#18613=ORIENTED_EDGE('',*,*,#13437,.F.);
#18614=ORIENTED_EDGE('',*,*,#13434,.F.);
#18615=ORIENTED_EDGE('',*,*,#13438,.F.);
#18616=ORIENTED_EDGE('',*,*,#13439,.F.);
#18617=ORIENTED_EDGE('',*,*,#13440,.F.);
#18618=ORIENTED_EDGE('',*,*,#13441,.F.);
#18619=ORIENTED_EDGE('',*,*,#13442,.F.);
#18620=ORIENTED_EDGE('',*,*,#13443,.F.);
#18621=ORIENTED_EDGE('',*,*,#13407,.T.);
#18622=ORIENTED_EDGE('',*,*,#13436,.F.);
#18623=ORIENTED_EDGE('',*,*,#13444,.T.);
#18624=ORIENTED_EDGE('',*,*,#13445,.T.);
#18625=ORIENTED_EDGE('',*,*,#13444,.F.);
#18626=ORIENTED_EDGE('',*,*,#13443,.T.);
#18627=ORIENTED_EDGE('',*,*,#13446,.T.);
#18628=ORIENTED_EDGE('',*,*,#13447,.T.);
#18629=ORIENTED_EDGE('',*,*,#13446,.F.);
#18630=ORIENTED_EDGE('',*,*,#13447,.F.);
#18631=ORIENTED_EDGE('',*,*,#13448,.T.);
#18632=ORIENTED_EDGE('',*,*,#13449,.T.);
#18633=ORIENTED_EDGE('',*,*,#13448,.F.);
#18634=ORIENTED_EDGE('',*,*,#13438,.T.);
#18635=ORIENTED_EDGE('',*,*,#13450,.T.);
#18636=ORIENTED_EDGE('',*,*,#13451,.T.);
#18637=ORIENTED_EDGE('',*,*,#13450,.F.);
#18638=ORIENTED_EDGE('',*,*,#13451,.F.);
#18639=ORIENTED_EDGE('',*,*,#13452,.T.);
#18640=ORIENTED_EDGE('',*,*,#13453,.T.);
#18641=ORIENTED_EDGE('',*,*,#13452,.F.);
#18642=ORIENTED_EDGE('',*,*,#13442,.T.);
#18643=ORIENTED_EDGE('',*,*,#13454,.T.);
#18644=ORIENTED_EDGE('',*,*,#13455,.T.);
#18645=ORIENTED_EDGE('',*,*,#13454,.F.);
#18646=ORIENTED_EDGE('',*,*,#13455,.F.);
#18647=ORIENTED_EDGE('',*,*,#13456,.T.);
#18648=ORIENTED_EDGE('',*,*,#13457,.T.);
#18649=ORIENTED_EDGE('',*,*,#13456,.F.);
#18650=ORIENTED_EDGE('',*,*,#13439,.T.);
#18651=ORIENTED_EDGE('',*,*,#13458,.T.);
#18652=ORIENTED_EDGE('',*,*,#13459,.T.);
#18653=ORIENTED_EDGE('',*,*,#13458,.F.);
#18654=ORIENTED_EDGE('',*,*,#13459,.F.);
#18655=ORIENTED_EDGE('',*,*,#13460,.T.);
#18656=ORIENTED_EDGE('',*,*,#13461,.T.);
#18657=ORIENTED_EDGE('',*,*,#13460,.F.);
#18658=ORIENTED_EDGE('',*,*,#13441,.T.);
#18659=ORIENTED_EDGE('',*,*,#13462,.T.);
#18660=ORIENTED_EDGE('',*,*,#13463,.T.);
#18661=ORIENTED_EDGE('',*,*,#13462,.F.);
#18662=ORIENTED_EDGE('',*,*,#13463,.F.);
#18663=ORIENTED_EDGE('',*,*,#13464,.T.);
#18664=ORIENTED_EDGE('',*,*,#13465,.T.);
#18665=ORIENTED_EDGE('',*,*,#13464,.F.);
#18666=ORIENTED_EDGE('',*,*,#13465,.F.);
#18667=ORIENTED_EDGE('',*,*,#13466,.T.);
#18668=ORIENTED_EDGE('',*,*,#13466,.F.);
#18669=ORIENTED_EDGE('',*,*,#13461,.F.);
#18670=ORIENTED_EDGE('',*,*,#13467,.T.);
#18671=ORIENTED_EDGE('',*,*,#13467,.F.);
#18672=ORIENTED_EDGE('',*,*,#13457,.F.);
#18673=ORIENTED_EDGE('',*,*,#13468,.T.);
#18674=ORIENTED_EDGE('',*,*,#13468,.F.);
#18675=ORIENTED_EDGE('',*,*,#13453,.F.);
#18676=ORIENTED_EDGE('',*,*,#13469,.T.);
#18677=ORIENTED_EDGE('',*,*,#13469,.F.);
#18678=ORIENTED_EDGE('',*,*,#13449,.F.);
#18679=ORIENTED_EDGE('',*,*,#13470,.T.);
#18680=ORIENTED_EDGE('',*,*,#13470,.F.);
#18681=ORIENTED_EDGE('',*,*,#13445,.F.);
#18682=ORIENTED_EDGE('',*,*,#13471,.T.);
#18683=ORIENTED_EDGE('',*,*,#13471,.F.);
#18684=ORIENTED_EDGE('',*,*,#13440,.T.);
#18685=ORIENTED_EDGE('',*,*,#13472,.T.);
#18686=ORIENTED_EDGE('',*,*,#13473,.T.);
#18687=ORIENTED_EDGE('',*,*,#13474,.T.);
#18688=ORIENTED_EDGE('',*,*,#13472,.F.);
#18689=ORIENTED_EDGE('',*,*,#13475,.T.);
#18690=ORIENTED_EDGE('',*,*,#13476,.T.);
#18691=ORIENTED_EDGE('',*,*,#13473,.F.);
#18692=ORIENTED_EDGE('',*,*,#13474,.F.);
#18693=ORIENTED_EDGE('',*,*,#13476,.F.);
#18694=ORIENTED_EDGE('',*,*,#13432,.F.);
#18695=ORIENTED_EDGE('',*,*,#13368,.T.);
#18696=ORIENTED_EDGE('',*,*,#13405,.T.);
#18697=ORIENTED_EDGE('',*,*,#13402,.T.);
#18698=ORIENTED_EDGE('',*,*,#13399,.T.);
#18699=ORIENTED_EDGE('',*,*,#13396,.T.);
#18700=ORIENTED_EDGE('',*,*,#13393,.T.);
#18701=ORIENTED_EDGE('',*,*,#13390,.T.);
#18702=ORIENTED_EDGE('',*,*,#13387,.T.);
#18703=ORIENTED_EDGE('',*,*,#13384,.T.);
#18704=ORIENTED_EDGE('',*,*,#13381,.T.);
#18705=ORIENTED_EDGE('',*,*,#13378,.T.);
#18706=ORIENTED_EDGE('',*,*,#13375,.T.);
#18707=ORIENTED_EDGE('',*,*,#13372,.T.);
#18708=ORIENTED_EDGE('',*,*,#13329,.T.);
#18709=ORIENTED_EDGE('',*,*,#13366,.T.);
#18710=ORIENTED_EDGE('',*,*,#13363,.T.);
#18711=ORIENTED_EDGE('',*,*,#13360,.T.);
#18712=ORIENTED_EDGE('',*,*,#13357,.T.);
#18713=ORIENTED_EDGE('',*,*,#13354,.T.);
#18714=ORIENTED_EDGE('',*,*,#13351,.T.);
#18715=ORIENTED_EDGE('',*,*,#13348,.T.);
#18716=ORIENTED_EDGE('',*,*,#13345,.T.);
#18717=ORIENTED_EDGE('',*,*,#13342,.T.);
#18718=ORIENTED_EDGE('',*,*,#13339,.T.);
#18719=ORIENTED_EDGE('',*,*,#13336,.T.);
#18720=ORIENTED_EDGE('',*,*,#13333,.T.);
#18721=ORIENTED_EDGE('',*,*,#13248,.T.);
#18722=ORIENTED_EDGE('',*,*,#13303,.T.);
#18723=ORIENTED_EDGE('',*,*,#13300,.T.);
#18724=ORIENTED_EDGE('',*,*,#13297,.T.);
#18725=ORIENTED_EDGE('',*,*,#13294,.T.);
#18726=ORIENTED_EDGE('',*,*,#13291,.T.);
#18727=ORIENTED_EDGE('',*,*,#13288,.T.);
#18728=ORIENTED_EDGE('',*,*,#13285,.T.);
#18729=ORIENTED_EDGE('',*,*,#13282,.T.);
#18730=ORIENTED_EDGE('',*,*,#13279,.T.);
#18731=ORIENTED_EDGE('',*,*,#13276,.T.);
#18732=ORIENTED_EDGE('',*,*,#13273,.T.);
#18733=ORIENTED_EDGE('',*,*,#13270,.T.);
#18734=ORIENTED_EDGE('',*,*,#13267,.T.);
#18735=ORIENTED_EDGE('',*,*,#13264,.T.);
#18736=ORIENTED_EDGE('',*,*,#13261,.T.);
#18737=ORIENTED_EDGE('',*,*,#13258,.T.);
#18738=ORIENTED_EDGE('',*,*,#13255,.T.);
#18739=ORIENTED_EDGE('',*,*,#13252,.T.);
#18740=ORIENTED_EDGE('',*,*,#13188,.T.);
#18741=ORIENTED_EDGE('',*,*,#13219,.T.);
#18742=ORIENTED_EDGE('',*,*,#13216,.T.);
#18743=ORIENTED_EDGE('',*,*,#13213,.T.);
#18744=ORIENTED_EDGE('',*,*,#13210,.T.);
#18745=ORIENTED_EDGE('',*,*,#13207,.T.);
#18746=ORIENTED_EDGE('',*,*,#13204,.T.);
#18747=ORIENTED_EDGE('',*,*,#13201,.T.);
#18748=ORIENTED_EDGE('',*,*,#13198,.T.);
#18749=ORIENTED_EDGE('',*,*,#13195,.T.);
#18750=ORIENTED_EDGE('',*,*,#13192,.T.);
#18751=ORIENTED_EDGE('',*,*,#13098,.T.);
#18752=ORIENTED_EDGE('',*,*,#13162,.T.);
#18753=ORIENTED_EDGE('',*,*,#13159,.T.);
#18754=ORIENTED_EDGE('',*,*,#13156,.T.);
#18755=ORIENTED_EDGE('',*,*,#13153,.T.);
#18756=ORIENTED_EDGE('',*,*,#13150,.T.);
#18757=ORIENTED_EDGE('',*,*,#13147,.T.);
#18758=ORIENTED_EDGE('',*,*,#13144,.T.);
#18759=ORIENTED_EDGE('',*,*,#13141,.T.);
#18760=ORIENTED_EDGE('',*,*,#13138,.T.);
#18761=ORIENTED_EDGE('',*,*,#13135,.T.);
#18762=ORIENTED_EDGE('',*,*,#13132,.T.);
#18763=ORIENTED_EDGE('',*,*,#13129,.T.);
#18764=ORIENTED_EDGE('',*,*,#13126,.T.);
#18765=ORIENTED_EDGE('',*,*,#13123,.T.);
#18766=ORIENTED_EDGE('',*,*,#13120,.T.);
#18767=ORIENTED_EDGE('',*,*,#13117,.T.);
#18768=ORIENTED_EDGE('',*,*,#13114,.T.);
#18769=ORIENTED_EDGE('',*,*,#13111,.T.);
#18770=ORIENTED_EDGE('',*,*,#13108,.T.);
#18771=ORIENTED_EDGE('',*,*,#13105,.T.);
#18772=ORIENTED_EDGE('',*,*,#13102,.T.);
#18773=ORIENTED_EDGE('',*,*,#13008,.T.);
#18774=ORIENTED_EDGE('',*,*,#13096,.T.);
#18775=ORIENTED_EDGE('',*,*,#13093,.T.);
#18776=ORIENTED_EDGE('',*,*,#13090,.T.);
#18777=ORIENTED_EDGE('',*,*,#13087,.T.);
#18778=ORIENTED_EDGE('',*,*,#13084,.T.);
#18779=ORIENTED_EDGE('',*,*,#13081,.T.);
#18780=ORIENTED_EDGE('',*,*,#13078,.T.);
#18781=ORIENTED_EDGE('',*,*,#13075,.T.);
#18782=ORIENTED_EDGE('',*,*,#13072,.T.);
#18783=ORIENTED_EDGE('',*,*,#13069,.T.);
#18784=ORIENTED_EDGE('',*,*,#13066,.T.);
#18785=ORIENTED_EDGE('',*,*,#13063,.T.);
#18786=ORIENTED_EDGE('',*,*,#13060,.T.);
#18787=ORIENTED_EDGE('',*,*,#13057,.T.);
#18788=ORIENTED_EDGE('',*,*,#13054,.T.);
#18789=ORIENTED_EDGE('',*,*,#13051,.T.);
#18790=ORIENTED_EDGE('',*,*,#13048,.T.);
#18791=ORIENTED_EDGE('',*,*,#13045,.T.);
#18792=ORIENTED_EDGE('',*,*,#13042,.T.);
#18793=ORIENTED_EDGE('',*,*,#13039,.T.);
#18794=ORIENTED_EDGE('',*,*,#13036,.T.);
#18795=ORIENTED_EDGE('',*,*,#13033,.T.);
#18796=ORIENTED_EDGE('',*,*,#13030,.T.);
#18797=ORIENTED_EDGE('',*,*,#13027,.T.);
#18798=ORIENTED_EDGE('',*,*,#13024,.T.);
#18799=ORIENTED_EDGE('',*,*,#13021,.T.);
#18800=ORIENTED_EDGE('',*,*,#13018,.T.);
#18801=ORIENTED_EDGE('',*,*,#13015,.T.);
#18802=ORIENTED_EDGE('',*,*,#13012,.T.);
#18803=ORIENTED_EDGE('',*,*,#12903,.T.);
#18804=ORIENTED_EDGE('',*,*,#13006,.T.);
#18805=ORIENTED_EDGE('',*,*,#13003,.T.);
#18806=ORIENTED_EDGE('',*,*,#13000,.T.);
#18807=ORIENTED_EDGE('',*,*,#12997,.T.);
#18808=ORIENTED_EDGE('',*,*,#12994,.T.);
#18809=ORIENTED_EDGE('',*,*,#12991,.T.);
#18810=ORIENTED_EDGE('',*,*,#12988,.T.);
#18811=ORIENTED_EDGE('',*,*,#12985,.T.);
#18812=ORIENTED_EDGE('',*,*,#12982,.T.);
#18813=ORIENTED_EDGE('',*,*,#12979,.T.);
#18814=ORIENTED_EDGE('',*,*,#12976,.T.);
#18815=ORIENTED_EDGE('',*,*,#12973,.T.);
#18816=ORIENTED_EDGE('',*,*,#12970,.T.);
#18817=ORIENTED_EDGE('',*,*,#12967,.T.);
#18818=ORIENTED_EDGE('',*,*,#12964,.T.);
#18819=ORIENTED_EDGE('',*,*,#12961,.T.);
#18820=ORIENTED_EDGE('',*,*,#12958,.T.);
#18821=ORIENTED_EDGE('',*,*,#12955,.T.);
#18822=ORIENTED_EDGE('',*,*,#12952,.T.);
#18823=ORIENTED_EDGE('',*,*,#12949,.T.);
#18824=ORIENTED_EDGE('',*,*,#12946,.T.);
#18825=ORIENTED_EDGE('',*,*,#12943,.T.);
#18826=ORIENTED_EDGE('',*,*,#12940,.T.);
#18827=ORIENTED_EDGE('',*,*,#12937,.T.);
#18828=ORIENTED_EDGE('',*,*,#12934,.T.);
#18829=ORIENTED_EDGE('',*,*,#12931,.T.);
#18830=ORIENTED_EDGE('',*,*,#12928,.T.);
#18831=ORIENTED_EDGE('',*,*,#12925,.T.);
#18832=ORIENTED_EDGE('',*,*,#12922,.T.);
#18833=ORIENTED_EDGE('',*,*,#12919,.T.);
#18834=ORIENTED_EDGE('',*,*,#12916,.T.);
#18835=ORIENTED_EDGE('',*,*,#12913,.T.);
#18836=ORIENTED_EDGE('',*,*,#12910,.T.);
#18837=ORIENTED_EDGE('',*,*,#12907,.T.);
#18838=ORIENTED_EDGE('',*,*,#12879,.T.);
#18839=ORIENTED_EDGE('',*,*,#12901,.T.);
#18840=ORIENTED_EDGE('',*,*,#12898,.T.);
#18841=ORIENTED_EDGE('',*,*,#12895,.T.);
#18842=ORIENTED_EDGE('',*,*,#12892,.T.);
#18843=ORIENTED_EDGE('',*,*,#12889,.T.);
#18844=ORIENTED_EDGE('',*,*,#12886,.T.);
#18845=ORIENTED_EDGE('',*,*,#12883,.T.);
#18846=ORIENTED_EDGE('',*,*,#12852,.T.);
#18847=ORIENTED_EDGE('',*,*,#12862,.T.);
#18848=ORIENTED_EDGE('',*,*,#12859,.T.);
#18849=ORIENTED_EDGE('',*,*,#12856,.T.);
#18850=ORIENTED_EDGE('',*,*,#12762,.T.);
#18851=ORIENTED_EDGE('',*,*,#12850,.T.);
#18852=ORIENTED_EDGE('',*,*,#12847,.T.);
#18853=ORIENTED_EDGE('',*,*,#12844,.T.);
#18854=ORIENTED_EDGE('',*,*,#12841,.T.);
#18855=ORIENTED_EDGE('',*,*,#12838,.T.);
#18856=ORIENTED_EDGE('',*,*,#12835,.T.);
#18857=ORIENTED_EDGE('',*,*,#12832,.T.);
#18858=ORIENTED_EDGE('',*,*,#12829,.T.);
#18859=ORIENTED_EDGE('',*,*,#12826,.T.);
#18860=ORIENTED_EDGE('',*,*,#12823,.T.);
#18861=ORIENTED_EDGE('',*,*,#12820,.T.);
#18862=ORIENTED_EDGE('',*,*,#12817,.T.);
#18863=ORIENTED_EDGE('',*,*,#12814,.T.);
#18864=ORIENTED_EDGE('',*,*,#12811,.T.);
#18865=ORIENTED_EDGE('',*,*,#12808,.T.);
#18866=ORIENTED_EDGE('',*,*,#12805,.T.);
#18867=ORIENTED_EDGE('',*,*,#12802,.T.);
#18868=ORIENTED_EDGE('',*,*,#12799,.T.);
#18869=ORIENTED_EDGE('',*,*,#12796,.T.);
#18870=ORIENTED_EDGE('',*,*,#12793,.T.);
#18871=ORIENTED_EDGE('',*,*,#12790,.T.);
#18872=ORIENTED_EDGE('',*,*,#12787,.T.);
#18873=ORIENTED_EDGE('',*,*,#12784,.T.);
#18874=ORIENTED_EDGE('',*,*,#12781,.T.);
#18875=ORIENTED_EDGE('',*,*,#12778,.T.);
#18876=ORIENTED_EDGE('',*,*,#12775,.T.);
#18877=ORIENTED_EDGE('',*,*,#12772,.T.);
#18878=ORIENTED_EDGE('',*,*,#12769,.T.);
#18879=ORIENTED_EDGE('',*,*,#12766,.T.);
#18880=ORIENTED_EDGE('',*,*,#12717,.T.);
#18881=ORIENTED_EDGE('',*,*,#12760,.T.);
#18882=ORIENTED_EDGE('',*,*,#12757,.T.);
#18883=ORIENTED_EDGE('',*,*,#12754,.T.);
#18884=ORIENTED_EDGE('',*,*,#12751,.T.);
#18885=ORIENTED_EDGE('',*,*,#12748,.T.);
#18886=ORIENTED_EDGE('',*,*,#12745,.T.);
#18887=ORIENTED_EDGE('',*,*,#12742,.T.);
#18888=ORIENTED_EDGE('',*,*,#12739,.T.);
#18889=ORIENTED_EDGE('',*,*,#12736,.T.);
#18890=ORIENTED_EDGE('',*,*,#12733,.T.);
#18891=ORIENTED_EDGE('',*,*,#12730,.T.);
#18892=ORIENTED_EDGE('',*,*,#12727,.T.);
#18893=ORIENTED_EDGE('',*,*,#12724,.T.);
#18894=ORIENTED_EDGE('',*,*,#12721,.T.);
#18895=ORIENTED_EDGE('',*,*,#12690,.T.);
#18896=ORIENTED_EDGE('',*,*,#12715,.T.);
#18897=ORIENTED_EDGE('',*,*,#12712,.T.);
#18898=ORIENTED_EDGE('',*,*,#12709,.T.);
#18899=ORIENTED_EDGE('',*,*,#12706,.T.);
#18900=ORIENTED_EDGE('',*,*,#12703,.T.);
#18901=ORIENTED_EDGE('',*,*,#12700,.T.);
#18902=ORIENTED_EDGE('',*,*,#12697,.T.);
#18903=ORIENTED_EDGE('',*,*,#12694,.T.);
#18904=ORIENTED_EDGE('',*,*,#12654,.T.);
#18905=ORIENTED_EDGE('',*,*,#12688,.T.);
#18906=ORIENTED_EDGE('',*,*,#12685,.T.);
#18907=ORIENTED_EDGE('',*,*,#12682,.T.);
#18908=ORIENTED_EDGE('',*,*,#12679,.T.);
#18909=ORIENTED_EDGE('',*,*,#12676,.T.);
#18910=ORIENTED_EDGE('',*,*,#12673,.T.);
#18911=ORIENTED_EDGE('',*,*,#12670,.T.);
#18912=ORIENTED_EDGE('',*,*,#12667,.T.);
#18913=ORIENTED_EDGE('',*,*,#12664,.T.);
#18914=ORIENTED_EDGE('',*,*,#12661,.T.);
#18915=ORIENTED_EDGE('',*,*,#12658,.T.);
#18916=ORIENTED_EDGE('',*,*,#12549,.T.);
#18917=ORIENTED_EDGE('',*,*,#12628,.T.);
#18918=ORIENTED_EDGE('',*,*,#12625,.T.);
#18919=ORIENTED_EDGE('',*,*,#12622,.T.);
#18920=ORIENTED_EDGE('',*,*,#12619,.T.);
#18921=ORIENTED_EDGE('',*,*,#12616,.T.);
#18922=ORIENTED_EDGE('',*,*,#12613,.T.);
#18923=ORIENTED_EDGE('',*,*,#12610,.T.);
#18924=ORIENTED_EDGE('',*,*,#12607,.T.);
#18925=ORIENTED_EDGE('',*,*,#12604,.T.);
#18926=ORIENTED_EDGE('',*,*,#12601,.T.);
#18927=ORIENTED_EDGE('',*,*,#12598,.T.);
#18928=ORIENTED_EDGE('',*,*,#12595,.T.);
#18929=ORIENTED_EDGE('',*,*,#12592,.T.);
#18930=ORIENTED_EDGE('',*,*,#12589,.T.);
#18931=ORIENTED_EDGE('',*,*,#12586,.T.);
#18932=ORIENTED_EDGE('',*,*,#12583,.T.);
#18933=ORIENTED_EDGE('',*,*,#12580,.T.);
#18934=ORIENTED_EDGE('',*,*,#12577,.T.);
#18935=ORIENTED_EDGE('',*,*,#12574,.T.);
#18936=ORIENTED_EDGE('',*,*,#12571,.T.);
#18937=ORIENTED_EDGE('',*,*,#12568,.T.);
#18938=ORIENTED_EDGE('',*,*,#12565,.T.);
#18939=ORIENTED_EDGE('',*,*,#12562,.T.);
#18940=ORIENTED_EDGE('',*,*,#12559,.T.);
#18941=ORIENTED_EDGE('',*,*,#12556,.T.);
#18942=ORIENTED_EDGE('',*,*,#12553,.T.);
#18943=ORIENTED_EDGE('',*,*,#13430,.F.);
#18944=ORIENTED_EDGE('',*,*,#13477,.T.);
#18945=ORIENTED_EDGE('',*,*,#13437,.T.);
#18946=ORIENTED_EDGE('',*,*,#13477,.F.);
#18947=ORIENTED_EDGE('',*,*,#13478,.F.);
#18948=ORIENTED_EDGE('',*,*,#13478,.T.);
#18949=ORIENTED_EDGE('',*,*,#13479,.T.);
#18950=ORIENTED_EDGE('',*,*,#13480,.F.);
#18951=ORIENTED_EDGE('',*,*,#13479,.F.);
#18952=ORIENTED_EDGE('',*,*,#13475,.F.);
#18953=ORIENTED_EDGE('',*,*,#13480,.T.);
#18954=ORIENTED_EDGE('',*,*,#13481,.F.);
#18955=ORIENTED_EDGE('',*,*,#13482,.T.);
#18956=ORIENTED_EDGE('',*,*,#13483,.T.);
#18957=ORIENTED_EDGE('',*,*,#13484,.T.);
#18958=ORIENTED_EDGE('',*,*,#13482,.F.);
#18959=ORIENTED_EDGE('',*,*,#13484,.F.);
#18960=ORIENTED_EDGE('',*,*,#13485,.F.);
#18961=ORIENTED_EDGE('',*,*,#13483,.F.);
#18962=ORIENTED_EDGE('',*,*,#13485,.T.);
#18963=ORIENTED_EDGE('',*,*,#13486,.T.);
#18964=ORIENTED_EDGE('',*,*,#13487,.T.);
#18965=ORIENTED_EDGE('',*,*,#13486,.F.);
#18966=ORIENTED_EDGE('',*,*,#13487,.F.);
#18967=ORIENTED_EDGE('',*,*,#13488,.T.);
#18968=ORIENTED_EDGE('',*,*,#13489,.T.);
#18969=ORIENTED_EDGE('',*,*,#13490,.T.);
#18970=ORIENTED_EDGE('',*,*,#13488,.F.);
#18971=ORIENTED_EDGE('',*,*,#13490,.F.);
#18972=ORIENTED_EDGE('',*,*,#13491,.F.);
#18973=ORIENTED_EDGE('',*,*,#13489,.F.);
#18974=ORIENTED_EDGE('',*,*,#13491,.T.);
#18975=ORIENTED_EDGE('',*,*,#13492,.T.);
#18976=ORIENTED_EDGE('',*,*,#13493,.T.);
#18977=ORIENTED_EDGE('',*,*,#13492,.F.);
#18978=ORIENTED_EDGE('',*,*,#13494,.F.);
#18979=ORIENTED_EDGE('',*,*,#13495,.T.);
#18980=ORIENTED_EDGE('',*,*,#13496,.T.);
#18981=ORIENTED_EDGE('',*,*,#13495,.F.);
#18982=ORIENTED_EDGE('',*,*,#13497,.F.);
#18983=ORIENTED_EDGE('',*,*,#13498,.T.);
#18984=ORIENTED_EDGE('',*,*,#13494,.T.);
#18985=ORIENTED_EDGE('',*,*,#13498,.F.);
#18986=ORIENTED_EDGE('',*,*,#13493,.F.);
#18987=ORIENTED_EDGE('',*,*,#13499,.T.);
#18988=ORIENTED_EDGE('',*,*,#13497,.T.);
#18989=ORIENTED_EDGE('',*,*,#13499,.F.);
#18990=ORIENTED_EDGE('',*,*,#13500,.F.);
#18991=ORIENTED_EDGE('',*,*,#13501,.T.);
#18992=ORIENTED_EDGE('',*,*,#13481,.T.);
#18993=ORIENTED_EDGE('',*,*,#13501,.F.);
#18994=ORIENTED_EDGE('',*,*,#13502,.F.);
#18995=ORIENTED_EDGE('',*,*,#13503,.T.);
#18996=ORIENTED_EDGE('',*,*,#13500,.T.);
#18997=ORIENTED_EDGE('',*,*,#13503,.F.);
#18998=ORIENTED_EDGE('',*,*,#13502,.T.);
#18999=ORIENTED_EDGE('',*,*,#13504,.F.);
#19000=ORIENTED_EDGE('',*,*,#13504,.T.);
#19001=ORIENTED_EDGE('',*,*,#13505,.T.);
#19002=ORIENTED_EDGE('',*,*,#13506,.F.);
#19003=ORIENTED_EDGE('',*,*,#13505,.F.);
#19004=ORIENTED_EDGE('',*,*,#13506,.T.);
#19005=ORIENTED_EDGE('',*,*,#13507,.T.);
#19006=ORIENTED_EDGE('',*,*,#13508,.F.);
#19007=ORIENTED_EDGE('',*,*,#13507,.F.);
#19008=ORIENTED_EDGE('',*,*,#13508,.T.);
#19009=ORIENTED_EDGE('',*,*,#13509,.T.);
#19010=ORIENTED_EDGE('',*,*,#13510,.F.);
#19011=ORIENTED_EDGE('',*,*,#13509,.F.);
#19012=ORIENTED_EDGE('',*,*,#13496,.F.);
#19013=ORIENTED_EDGE('',*,*,#13511,.T.);
#19014=ORIENTED_EDGE('',*,*,#13510,.T.);
#19015=ORIENTED_EDGE('',*,*,#13511,.F.);
#19016=ORIENTED_EDGE('',*,*,#13512,.F.);
#19017=ORIENTED_EDGE('',*,*,#13513,.T.);
#19018=ORIENTED_EDGE('',*,*,#13514,.T.);
#19019=ORIENTED_EDGE('',*,*,#13513,.F.);
#19020=ORIENTED_EDGE('',*,*,#13515,.F.);
#19021=ORIENTED_EDGE('',*,*,#13516,.T.);
#19022=ORIENTED_EDGE('',*,*,#13517,.T.);
#19023=ORIENTED_EDGE('',*,*,#13516,.F.);
#19024=ORIENTED_EDGE('',*,*,#13517,.F.);
#19025=ORIENTED_EDGE('',*,*,#13514,.F.);
#19026=ORIENTED_EDGE('',*,*,#13518,.F.);
#19027=ORIENTED_EDGE('',*,*,#13515,.T.);
#19028=ORIENTED_EDGE('',*,*,#13519,.T.);
#19029=ORIENTED_EDGE('',*,*,#13520,.T.);
#19030=ORIENTED_EDGE('',*,*,#13521,.F.);
#19031=ORIENTED_EDGE('',*,*,#13520,.F.);
#19032=ORIENTED_EDGE('',*,*,#13521,.T.);
#19033=ORIENTED_EDGE('',*,*,#13522,.T.);
#19034=ORIENTED_EDGE('',*,*,#13523,.F.);
#19035=ORIENTED_EDGE('',*,*,#13522,.F.);
#19036=ORIENTED_EDGE('',*,*,#13524,.F.);
#19037=ORIENTED_EDGE('',*,*,#13523,.T.);
#19038=ORIENTED_EDGE('',*,*,#13524,.T.);
#19039=ORIENTED_EDGE('',*,*,#13525,.T.);
#19040=ORIENTED_EDGE('',*,*,#13526,.F.);
#19041=ORIENTED_EDGE('',*,*,#13525,.F.);
#19042=ORIENTED_EDGE('',*,*,#13512,.T.);
#19043=ORIENTED_EDGE('',*,*,#13526,.T.);
#19044=ORIENTED_EDGE('',*,*,#13527,.F.);
#19045=ORIENTED_EDGE('',*,*,#13528,.T.);
#19046=ORIENTED_EDGE('',*,*,#13518,.T.);
#19047=ORIENTED_EDGE('',*,*,#13528,.F.);
#19048=ORIENTED_EDGE('',*,*,#13529,.F.);
#19049=ORIENTED_EDGE('',*,*,#13530,.T.);
#19050=ORIENTED_EDGE('',*,*,#13527,.T.);
#19051=ORIENTED_EDGE('',*,*,#13530,.F.);
#19052=ORIENTED_EDGE('',*,*,#13531,.F.);
#19053=ORIENTED_EDGE('',*,*,#13532,.T.);
#19054=ORIENTED_EDGE('',*,*,#13529,.T.);
#19055=ORIENTED_EDGE('',*,*,#13532,.F.);
#19056=ORIENTED_EDGE('',*,*,#13531,.T.);
#19057=ORIENTED_EDGE('',*,*,#13533,.F.);
#19058=ORIENTED_EDGE('',*,*,#13534,.F.);
#19059=ORIENTED_EDGE('',*,*,#13535,.T.);
#19060=ORIENTED_EDGE('',*,*,#13533,.T.);
#19061=ORIENTED_EDGE('',*,*,#13535,.F.);
#19062=ORIENTED_EDGE('',*,*,#13536,.F.);
#19063=ORIENTED_EDGE('',*,*,#13537,.T.);
#19064=ORIENTED_EDGE('',*,*,#13534,.T.);
#19065=ORIENTED_EDGE('',*,*,#13537,.F.);
#19066=ORIENTED_EDGE('',*,*,#13536,.T.);
#19067=ORIENTED_EDGE('',*,*,#13519,.F.);
#19068=ORIENTED_EDGE('',*,*,#13538,.T.);
#19069=ORIENTED_EDGE('',*,*,#13539,.T.);
#19070=ORIENTED_EDGE('',*,*,#13540,.F.);
#19071=ORIENTED_EDGE('',*,*,#13539,.F.);
#19072=ORIENTED_EDGE('',*,*,#13541,.F.);
#19073=ORIENTED_EDGE('',*,*,#13542,.T.);
#19074=ORIENTED_EDGE('',*,*,#13543,.F.);
#19075=ORIENTED_EDGE('',*,*,#13544,.T.);
#19076=ORIENTED_EDGE('',*,*,#13545,.F.);
#19077=ORIENTED_EDGE('',*,*,#13546,.T.);
#19078=ORIENTED_EDGE('',*,*,#13547,.F.);
#19079=ORIENTED_EDGE('',*,*,#13548,.T.);
#19080=ORIENTED_EDGE('',*,*,#13549,.F.);
#19081=ORIENTED_EDGE('',*,*,#13550,.T.);
#19082=ORIENTED_EDGE('',*,*,#13551,.F.);
#19083=ORIENTED_EDGE('',*,*,#13552,.T.);
#19084=ORIENTED_EDGE('',*,*,#13553,.F.);
#19085=ORIENTED_EDGE('',*,*,#13554,.T.);
#19086=ORIENTED_EDGE('',*,*,#13555,.F.);
#19087=ORIENTED_EDGE('',*,*,#13556,.T.);
#19088=ORIENTED_EDGE('',*,*,#13557,.F.);
#19089=ORIENTED_EDGE('',*,*,#13558,.T.);
#19090=ORIENTED_EDGE('',*,*,#13559,.F.);
#19091=ORIENTED_EDGE('',*,*,#13560,.T.);
#19092=ORIENTED_EDGE('',*,*,#13561,.F.);
#19093=ORIENTED_EDGE('',*,*,#13562,.T.);
#19094=ORIENTED_EDGE('',*,*,#13563,.F.);
#19095=ORIENTED_EDGE('',*,*,#13564,.T.);
#19096=ORIENTED_EDGE('',*,*,#13565,.F.);
#19097=ORIENTED_EDGE('',*,*,#13566,.T.);
#19098=ORIENTED_EDGE('',*,*,#13567,.F.);
#19099=ORIENTED_EDGE('',*,*,#13568,.T.);
#19100=ORIENTED_EDGE('',*,*,#13569,.F.);
#19101=ORIENTED_EDGE('',*,*,#13570,.T.);
#19102=ORIENTED_EDGE('',*,*,#13571,.F.);
#19103=ORIENTED_EDGE('',*,*,#13572,.T.);
#19104=ORIENTED_EDGE('',*,*,#13573,.F.);
#19105=ORIENTED_EDGE('',*,*,#13574,.T.);
#19106=ORIENTED_EDGE('',*,*,#13575,.F.);
#19107=ORIENTED_EDGE('',*,*,#13576,.T.);
#19108=ORIENTED_EDGE('',*,*,#13577,.F.);
#19109=ORIENTED_EDGE('',*,*,#13578,.T.);
#19110=ORIENTED_EDGE('',*,*,#13579,.F.);
#19111=ORIENTED_EDGE('',*,*,#13580,.T.);
#19112=ORIENTED_EDGE('',*,*,#13581,.F.);
#19113=ORIENTED_EDGE('',*,*,#13582,.T.);
#19114=ORIENTED_EDGE('',*,*,#13583,.F.);
#19115=ORIENTED_EDGE('',*,*,#13584,.T.);
#19116=ORIENTED_EDGE('',*,*,#13585,.F.);
#19117=ORIENTED_EDGE('',*,*,#13586,.T.);
#19118=ORIENTED_EDGE('',*,*,#13587,.F.);
#19119=ORIENTED_EDGE('',*,*,#13588,.T.);
#19120=ORIENTED_EDGE('',*,*,#13589,.F.);
#19121=ORIENTED_EDGE('',*,*,#13590,.T.);
#19122=ORIENTED_EDGE('',*,*,#13591,.F.);
#19123=ORIENTED_EDGE('',*,*,#13592,.T.);
#19124=ORIENTED_EDGE('',*,*,#13593,.F.);
#19125=ORIENTED_EDGE('',*,*,#13594,.T.);
#19126=ORIENTED_EDGE('',*,*,#13595,.F.);
#19127=ORIENTED_EDGE('',*,*,#13596,.T.);
#19128=ORIENTED_EDGE('',*,*,#13597,.F.);
#19129=ORIENTED_EDGE('',*,*,#13598,.T.);
#19130=ORIENTED_EDGE('',*,*,#13599,.F.);
#19131=ORIENTED_EDGE('',*,*,#13600,.T.);
#19132=ORIENTED_EDGE('',*,*,#13601,.F.);
#19133=ORIENTED_EDGE('',*,*,#13602,.T.);
#19134=ORIENTED_EDGE('',*,*,#13603,.F.);
#19135=ORIENTED_EDGE('',*,*,#13604,.T.);
#19136=ORIENTED_EDGE('',*,*,#13605,.T.);
#19137=ORIENTED_EDGE('',*,*,#13606,.F.);
#19138=ORIENTED_EDGE('',*,*,#13607,.T.);
#19139=ORIENTED_EDGE('',*,*,#13608,.F.);
#19140=ORIENTED_EDGE('',*,*,#13609,.F.);
#19141=ORIENTED_EDGE('',*,*,#13610,.T.);
#19142=ORIENTED_EDGE('',*,*,#13611,.T.);
#19143=ORIENTED_EDGE('',*,*,#13610,.F.);
#19144=ORIENTED_EDGE('',*,*,#13612,.F.);
#19145=ORIENTED_EDGE('',*,*,#13613,.T.);
#19146=ORIENTED_EDGE('',*,*,#13614,.F.);
#19147=ORIENTED_EDGE('',*,*,#13615,.T.);
#19148=ORIENTED_EDGE('',*,*,#13616,.F.);
#19149=ORIENTED_EDGE('',*,*,#13617,.T.);
#19150=ORIENTED_EDGE('',*,*,#13618,.F.);
#19151=ORIENTED_EDGE('',*,*,#13619,.T.);
#19152=ORIENTED_EDGE('',*,*,#13620,.F.);
#19153=ORIENTED_EDGE('',*,*,#13621,.T.);
#19154=ORIENTED_EDGE('',*,*,#13622,.F.);
#19155=ORIENTED_EDGE('',*,*,#13623,.T.);
#19156=ORIENTED_EDGE('',*,*,#13624,.F.);
#19157=ORIENTED_EDGE('',*,*,#13625,.T.);
#19158=ORIENTED_EDGE('',*,*,#13626,.F.);
#19159=ORIENTED_EDGE('',*,*,#13627,.T.);
#19160=ORIENTED_EDGE('',*,*,#13628,.F.);
#19161=ORIENTED_EDGE('',*,*,#13629,.T.);
#19162=ORIENTED_EDGE('',*,*,#13630,.F.);
#19163=ORIENTED_EDGE('',*,*,#13631,.T.);
#19164=ORIENTED_EDGE('',*,*,#13632,.F.);
#19165=ORIENTED_EDGE('',*,*,#13633,.T.);
#19166=ORIENTED_EDGE('',*,*,#13634,.F.);
#19167=ORIENTED_EDGE('',*,*,#13635,.T.);
#19168=ORIENTED_EDGE('',*,*,#13636,.F.);
#19169=ORIENTED_EDGE('',*,*,#13637,.T.);
#19170=ORIENTED_EDGE('',*,*,#13638,.F.);
#19171=ORIENTED_EDGE('',*,*,#13639,.T.);
#19172=ORIENTED_EDGE('',*,*,#13640,.F.);
#19173=ORIENTED_EDGE('',*,*,#13641,.T.);
#19174=ORIENTED_EDGE('',*,*,#13642,.F.);
#19175=ORIENTED_EDGE('',*,*,#13643,.T.);
#19176=ORIENTED_EDGE('',*,*,#13644,.F.);
#19177=ORIENTED_EDGE('',*,*,#13645,.T.);
#19178=ORIENTED_EDGE('',*,*,#13646,.F.);
#19179=ORIENTED_EDGE('',*,*,#13647,.T.);
#19180=ORIENTED_EDGE('',*,*,#13648,.F.);
#19181=ORIENTED_EDGE('',*,*,#13649,.T.);
#19182=ORIENTED_EDGE('',*,*,#13650,.F.);
#19183=ORIENTED_EDGE('',*,*,#13651,.T.);
#19184=ORIENTED_EDGE('',*,*,#13652,.F.);
#19185=ORIENTED_EDGE('',*,*,#13653,.T.);
#19186=ORIENTED_EDGE('',*,*,#13654,.F.);
#19187=ORIENTED_EDGE('',*,*,#13655,.T.);
#19188=ORIENTED_EDGE('',*,*,#13656,.F.);
#19189=ORIENTED_EDGE('',*,*,#13657,.T.);
#19190=ORIENTED_EDGE('',*,*,#13658,.F.);
#19191=ORIENTED_EDGE('',*,*,#13659,.T.);
#19192=ORIENTED_EDGE('',*,*,#13660,.F.);
#19193=ORIENTED_EDGE('',*,*,#13661,.T.);
#19194=ORIENTED_EDGE('',*,*,#13662,.F.);
#19195=ORIENTED_EDGE('',*,*,#13663,.T.);
#19196=ORIENTED_EDGE('',*,*,#13664,.F.);
#19197=ORIENTED_EDGE('',*,*,#13665,.T.);
#19198=ORIENTED_EDGE('',*,*,#13666,.F.);
#19199=ORIENTED_EDGE('',*,*,#13667,.T.);
#19200=ORIENTED_EDGE('',*,*,#13668,.F.);
#19201=ORIENTED_EDGE('',*,*,#13669,.T.);
#19202=ORIENTED_EDGE('',*,*,#13670,.F.);
#19203=ORIENTED_EDGE('',*,*,#13671,.T.);
#19204=ORIENTED_EDGE('',*,*,#13672,.F.);
#19205=ORIENTED_EDGE('',*,*,#13673,.T.);
#19206=ORIENTED_EDGE('',*,*,#13674,.F.);
#19207=ORIENTED_EDGE('',*,*,#13675,.T.);
#19208=ORIENTED_EDGE('',*,*,#13676,.T.);
#19209=ORIENTED_EDGE('',*,*,#13677,.F.);
#19210=ORIENTED_EDGE('',*,*,#13678,.T.);
#19211=ORIENTED_EDGE('',*,*,#13679,.F.);
#19212=ORIENTED_EDGE('',*,*,#13611,.F.);
#19213=ORIENTED_EDGE('',*,*,#13680,.T.);
#19214=ORIENTED_EDGE('',*,*,#13540,.T.);
#19215=ORIENTED_EDGE('',*,*,#13680,.F.);
#19216=ORIENTED_EDGE('',*,*,#13609,.T.);
#19217=ORIENTED_EDGE('',*,*,#13681,.T.);
#19218=ORIENTED_EDGE('',*,*,#13538,.F.);
#19219=ORIENTED_EDGE('',*,*,#13681,.F.);
#19220=ORIENTED_EDGE('',*,*,#13614,.T.);
#19221=ORIENTED_EDGE('',*,*,#13682,.T.);
#19222=ORIENTED_EDGE('',*,*,#13543,.T.);
#19223=ORIENTED_EDGE('',*,*,#13683,.T.);
#19224=ORIENTED_EDGE('',*,*,#13684,.F.);
#19225=ORIENTED_EDGE('',*,*,#13685,.T.);
#19226=ORIENTED_EDGE('',*,*,#13615,.F.);
#19227=ORIENTED_EDGE('',*,*,#13682,.F.);
#19228=ORIENTED_EDGE('',*,*,#13613,.F.);
#19229=ORIENTED_EDGE('',*,*,#13686,.T.);
#19230=ORIENTED_EDGE('',*,*,#13542,.F.);
#19231=ORIENTED_EDGE('',*,*,#13687,.T.);
#19232=ORIENTED_EDGE('',*,*,#13688,.F.);
#19233=ORIENTED_EDGE('',*,*,#13689,.F.);
#19234=ORIENTED_EDGE('',*,*,#13683,.F.);
#19235=ORIENTED_EDGE('',*,*,#13612,.T.);
#19236=ORIENTED_EDGE('',*,*,#13686,.F.);
#19237=ORIENTED_EDGE('',*,*,#13618,.T.);
#19238=ORIENTED_EDGE('',*,*,#13690,.T.);
#19239=ORIENTED_EDGE('',*,*,#13547,.T.);
#19240=ORIENTED_EDGE('',*,*,#13691,.T.);
#19241=ORIENTED_EDGE('',*,*,#13692,.F.);
#19242=ORIENTED_EDGE('',*,*,#13693,.T.);
#19243=ORIENTED_EDGE('',*,*,#13619,.F.);
#19244=ORIENTED_EDGE('',*,*,#13690,.F.);
#19245=ORIENTED_EDGE('',*,*,#13617,.F.);
#19246=ORIENTED_EDGE('',*,*,#13694,.T.);
#19247=ORIENTED_EDGE('',*,*,#13546,.F.);
#19248=ORIENTED_EDGE('',*,*,#13695,.T.);
#19249=ORIENTED_EDGE('',*,*,#13696,.F.);
#19250=ORIENTED_EDGE('',*,*,#13697,.F.);
#19251=ORIENTED_EDGE('',*,*,#13691,.F.);
#19252=ORIENTED_EDGE('',*,*,#13616,.T.);
#19253=ORIENTED_EDGE('',*,*,#13694,.F.);
#19254=ORIENTED_EDGE('',*,*,#13622,.T.);
#19255=ORIENTED_EDGE('',*,*,#13698,.T.);
#19256=ORIENTED_EDGE('',*,*,#13551,.T.);
#19257=ORIENTED_EDGE('',*,*,#13699,.T.);
#19258=ORIENTED_EDGE('',*,*,#13700,.F.);
#19259=ORIENTED_EDGE('',*,*,#13701,.T.);
#19260=ORIENTED_EDGE('',*,*,#13623,.F.);
#19261=ORIENTED_EDGE('',*,*,#13698,.F.);
#19262=ORIENTED_EDGE('',*,*,#13621,.F.);
#19263=ORIENTED_EDGE('',*,*,#13702,.T.);
#19264=ORIENTED_EDGE('',*,*,#13550,.F.);
#19265=ORIENTED_EDGE('',*,*,#13703,.T.);
#19266=ORIENTED_EDGE('',*,*,#13704,.F.);
#19267=ORIENTED_EDGE('',*,*,#13705,.F.);
#19268=ORIENTED_EDGE('',*,*,#13699,.F.);
#19269=ORIENTED_EDGE('',*,*,#13620,.T.);
#19270=ORIENTED_EDGE('',*,*,#13702,.F.);
#19271=ORIENTED_EDGE('',*,*,#13626,.T.);
#19272=ORIENTED_EDGE('',*,*,#13706,.T.);
#19273=ORIENTED_EDGE('',*,*,#13555,.T.);
#19274=ORIENTED_EDGE('',*,*,#13707,.T.);
#19275=ORIENTED_EDGE('',*,*,#13708,.F.);
#19276=ORIENTED_EDGE('',*,*,#13709,.T.);
#19277=ORIENTED_EDGE('',*,*,#13627,.F.);
#19278=ORIENTED_EDGE('',*,*,#13706,.F.);
#19279=ORIENTED_EDGE('',*,*,#13625,.F.);
#19280=ORIENTED_EDGE('',*,*,#13710,.T.);
#19281=ORIENTED_EDGE('',*,*,#13554,.F.);
#19282=ORIENTED_EDGE('',*,*,#13711,.T.);
#19283=ORIENTED_EDGE('',*,*,#13712,.F.);
#19284=ORIENTED_EDGE('',*,*,#13713,.F.);
#19285=ORIENTED_EDGE('',*,*,#13707,.F.);
#19286=ORIENTED_EDGE('',*,*,#13624,.T.);
#19287=ORIENTED_EDGE('',*,*,#13710,.F.);
#19288=ORIENTED_EDGE('',*,*,#13630,.T.);
#19289=ORIENTED_EDGE('',*,*,#13714,.T.);
#19290=ORIENTED_EDGE('',*,*,#13559,.T.);
#19291=ORIENTED_EDGE('',*,*,#13715,.T.);
#19292=ORIENTED_EDGE('',*,*,#13716,.F.);
#19293=ORIENTED_EDGE('',*,*,#13717,.T.);
#19294=ORIENTED_EDGE('',*,*,#13631,.F.);
#19295=ORIENTED_EDGE('',*,*,#13714,.F.);
#19296=ORIENTED_EDGE('',*,*,#13629,.F.);
#19297=ORIENTED_EDGE('',*,*,#13718,.T.);
#19298=ORIENTED_EDGE('',*,*,#13558,.F.);
#19299=ORIENTED_EDGE('',*,*,#13719,.T.);
#19300=ORIENTED_EDGE('',*,*,#13720,.F.);
#19301=ORIENTED_EDGE('',*,*,#13721,.F.);
#19302=ORIENTED_EDGE('',*,*,#13715,.F.);
#19303=ORIENTED_EDGE('',*,*,#13628,.T.);
#19304=ORIENTED_EDGE('',*,*,#13718,.F.);
#19305=ORIENTED_EDGE('',*,*,#13634,.T.);
#19306=ORIENTED_EDGE('',*,*,#13722,.T.);
#19307=ORIENTED_EDGE('',*,*,#13563,.T.);
#19308=ORIENTED_EDGE('',*,*,#13723,.T.);
#19309=ORIENTED_EDGE('',*,*,#13724,.F.);
#19310=ORIENTED_EDGE('',*,*,#13725,.T.);
#19311=ORIENTED_EDGE('',*,*,#13635,.F.);
#19312=ORIENTED_EDGE('',*,*,#13722,.F.);
#19313=ORIENTED_EDGE('',*,*,#13633,.F.);
#19314=ORIENTED_EDGE('',*,*,#13726,.T.);
#19315=ORIENTED_EDGE('',*,*,#13562,.F.);
#19316=ORIENTED_EDGE('',*,*,#13727,.T.);
#19317=ORIENTED_EDGE('',*,*,#13728,.F.);
#19318=ORIENTED_EDGE('',*,*,#13729,.F.);
#19319=ORIENTED_EDGE('',*,*,#13723,.F.);
#19320=ORIENTED_EDGE('',*,*,#13632,.T.);
#19321=ORIENTED_EDGE('',*,*,#13726,.F.);
#19322=ORIENTED_EDGE('',*,*,#13638,.T.);
#19323=ORIENTED_EDGE('',*,*,#13730,.T.);
#19324=ORIENTED_EDGE('',*,*,#13567,.T.);
#19325=ORIENTED_EDGE('',*,*,#13731,.T.);
#19326=ORIENTED_EDGE('',*,*,#13732,.F.);
#19327=ORIENTED_EDGE('',*,*,#13733,.T.);
#19328=ORIENTED_EDGE('',*,*,#13639,.F.);
#19329=ORIENTED_EDGE('',*,*,#13730,.F.);
#19330=ORIENTED_EDGE('',*,*,#13637,.F.);
#19331=ORIENTED_EDGE('',*,*,#13734,.T.);
#19332=ORIENTED_EDGE('',*,*,#13566,.F.);
#19333=ORIENTED_EDGE('',*,*,#13735,.T.);
#19334=ORIENTED_EDGE('',*,*,#13736,.F.);
#19335=ORIENTED_EDGE('',*,*,#13737,.F.);
#19336=ORIENTED_EDGE('',*,*,#13731,.F.);
#19337=ORIENTED_EDGE('',*,*,#13636,.T.);
#19338=ORIENTED_EDGE('',*,*,#13734,.F.);
#19339=ORIENTED_EDGE('',*,*,#13642,.T.);
#19340=ORIENTED_EDGE('',*,*,#13738,.T.);
#19341=ORIENTED_EDGE('',*,*,#13571,.T.);
#19342=ORIENTED_EDGE('',*,*,#13739,.T.);
#19343=ORIENTED_EDGE('',*,*,#13740,.F.);
#19344=ORIENTED_EDGE('',*,*,#13741,.T.);
#19345=ORIENTED_EDGE('',*,*,#13643,.F.);
#19346=ORIENTED_EDGE('',*,*,#13738,.F.);
#19347=ORIENTED_EDGE('',*,*,#13641,.F.);
#19348=ORIENTED_EDGE('',*,*,#13742,.T.);
#19349=ORIENTED_EDGE('',*,*,#13570,.F.);
#19350=ORIENTED_EDGE('',*,*,#13743,.T.);
#19351=ORIENTED_EDGE('',*,*,#13744,.F.);
#19352=ORIENTED_EDGE('',*,*,#13745,.F.);
#19353=ORIENTED_EDGE('',*,*,#13739,.F.);
#19354=ORIENTED_EDGE('',*,*,#13640,.T.);
#19355=ORIENTED_EDGE('',*,*,#13742,.F.);
#19356=ORIENTED_EDGE('',*,*,#13646,.T.);
#19357=ORIENTED_EDGE('',*,*,#13746,.T.);
#19358=ORIENTED_EDGE('',*,*,#13575,.T.);
#19359=ORIENTED_EDGE('',*,*,#13747,.T.);
#19360=ORIENTED_EDGE('',*,*,#13748,.F.);
#19361=ORIENTED_EDGE('',*,*,#13749,.T.);
#19362=ORIENTED_EDGE('',*,*,#13647,.F.);
#19363=ORIENTED_EDGE('',*,*,#13746,.F.);
#19364=ORIENTED_EDGE('',*,*,#13645,.F.);
#19365=ORIENTED_EDGE('',*,*,#13750,.T.);
#19366=ORIENTED_EDGE('',*,*,#13574,.F.);
#19367=ORIENTED_EDGE('',*,*,#13751,.T.);
#19368=ORIENTED_EDGE('',*,*,#13752,.F.);
#19369=ORIENTED_EDGE('',*,*,#13753,.F.);
#19370=ORIENTED_EDGE('',*,*,#13747,.F.);
#19371=ORIENTED_EDGE('',*,*,#13644,.T.);
#19372=ORIENTED_EDGE('',*,*,#13750,.F.);
#19373=ORIENTED_EDGE('',*,*,#13650,.T.);
#19374=ORIENTED_EDGE('',*,*,#13754,.T.);
#19375=ORIENTED_EDGE('',*,*,#13579,.T.);
#19376=ORIENTED_EDGE('',*,*,#13755,.T.);
#19377=ORIENTED_EDGE('',*,*,#13756,.F.);
#19378=ORIENTED_EDGE('',*,*,#13757,.T.);
#19379=ORIENTED_EDGE('',*,*,#13651,.F.);
#19380=ORIENTED_EDGE('',*,*,#13754,.F.);
#19381=ORIENTED_EDGE('',*,*,#13649,.F.);
#19382=ORIENTED_EDGE('',*,*,#13758,.T.);
#19383=ORIENTED_EDGE('',*,*,#13578,.F.);
#19384=ORIENTED_EDGE('',*,*,#13759,.T.);
#19385=ORIENTED_EDGE('',*,*,#13760,.F.);
#19386=ORIENTED_EDGE('',*,*,#13761,.F.);
#19387=ORIENTED_EDGE('',*,*,#13755,.F.);
#19388=ORIENTED_EDGE('',*,*,#13648,.T.);
#19389=ORIENTED_EDGE('',*,*,#13758,.F.);
#19390=ORIENTED_EDGE('',*,*,#13654,.T.);
#19391=ORIENTED_EDGE('',*,*,#13762,.T.);
#19392=ORIENTED_EDGE('',*,*,#13583,.T.);
#19393=ORIENTED_EDGE('',*,*,#13763,.T.);
#19394=ORIENTED_EDGE('',*,*,#13764,.F.);
#19395=ORIENTED_EDGE('',*,*,#13765,.T.);
#19396=ORIENTED_EDGE('',*,*,#13655,.F.);
#19397=ORIENTED_EDGE('',*,*,#13762,.F.);
#19398=ORIENTED_EDGE('',*,*,#13653,.F.);
#19399=ORIENTED_EDGE('',*,*,#13766,.T.);
#19400=ORIENTED_EDGE('',*,*,#13582,.F.);
#19401=ORIENTED_EDGE('',*,*,#13767,.T.);
#19402=ORIENTED_EDGE('',*,*,#13768,.F.);
#19403=ORIENTED_EDGE('',*,*,#13769,.F.);
#19404=ORIENTED_EDGE('',*,*,#13763,.F.);
#19405=ORIENTED_EDGE('',*,*,#13652,.T.);
#19406=ORIENTED_EDGE('',*,*,#13766,.F.);
#19407=ORIENTED_EDGE('',*,*,#13658,.T.);
#19408=ORIENTED_EDGE('',*,*,#13770,.T.);
#19409=ORIENTED_EDGE('',*,*,#13587,.T.);
#19410=ORIENTED_EDGE('',*,*,#13771,.T.);
#19411=ORIENTED_EDGE('',*,*,#13772,.F.);
#19412=ORIENTED_EDGE('',*,*,#13773,.T.);
#19413=ORIENTED_EDGE('',*,*,#13659,.F.);
#19414=ORIENTED_EDGE('',*,*,#13770,.F.);
#19415=ORIENTED_EDGE('',*,*,#13657,.F.);
#19416=ORIENTED_EDGE('',*,*,#13774,.T.);
#19417=ORIENTED_EDGE('',*,*,#13586,.F.);
#19418=ORIENTED_EDGE('',*,*,#13775,.T.);
#19419=ORIENTED_EDGE('',*,*,#13776,.F.);
#19420=ORIENTED_EDGE('',*,*,#13777,.F.);
#19421=ORIENTED_EDGE('',*,*,#13771,.F.);
#19422=ORIENTED_EDGE('',*,*,#13656,.T.);
#19423=ORIENTED_EDGE('',*,*,#13774,.F.);
#19424=ORIENTED_EDGE('',*,*,#13662,.T.);
#19425=ORIENTED_EDGE('',*,*,#13778,.T.);
#19426=ORIENTED_EDGE('',*,*,#13591,.T.);
#19427=ORIENTED_EDGE('',*,*,#13779,.T.);
#19428=ORIENTED_EDGE('',*,*,#13780,.F.);
#19429=ORIENTED_EDGE('',*,*,#13781,.T.);
#19430=ORIENTED_EDGE('',*,*,#13663,.F.);
#19431=ORIENTED_EDGE('',*,*,#13778,.F.);
#19432=ORIENTED_EDGE('',*,*,#13661,.F.);
#19433=ORIENTED_EDGE('',*,*,#13782,.T.);
#19434=ORIENTED_EDGE('',*,*,#13590,.F.);
#19435=ORIENTED_EDGE('',*,*,#13783,.T.);
#19436=ORIENTED_EDGE('',*,*,#13784,.F.);
#19437=ORIENTED_EDGE('',*,*,#13785,.F.);
#19438=ORIENTED_EDGE('',*,*,#13779,.F.);
#19439=ORIENTED_EDGE('',*,*,#13660,.T.);
#19440=ORIENTED_EDGE('',*,*,#13782,.F.);
#19441=ORIENTED_EDGE('',*,*,#13666,.T.);
#19442=ORIENTED_EDGE('',*,*,#13786,.T.);
#19443=ORIENTED_EDGE('',*,*,#13595,.T.);
#19444=ORIENTED_EDGE('',*,*,#13787,.T.);
#19445=ORIENTED_EDGE('',*,*,#13788,.F.);
#19446=ORIENTED_EDGE('',*,*,#13789,.T.);
#19447=ORIENTED_EDGE('',*,*,#13667,.F.);
#19448=ORIENTED_EDGE('',*,*,#13786,.F.);
#19449=ORIENTED_EDGE('',*,*,#13665,.F.);
#19450=ORIENTED_EDGE('',*,*,#13790,.T.);
#19451=ORIENTED_EDGE('',*,*,#13594,.F.);
#19452=ORIENTED_EDGE('',*,*,#13791,.T.);
#19453=ORIENTED_EDGE('',*,*,#13792,.F.);
#19454=ORIENTED_EDGE('',*,*,#13793,.F.);
#19455=ORIENTED_EDGE('',*,*,#13787,.F.);
#19456=ORIENTED_EDGE('',*,*,#13664,.T.);
#19457=ORIENTED_EDGE('',*,*,#13790,.F.);
#19458=ORIENTED_EDGE('',*,*,#13670,.T.);
#19459=ORIENTED_EDGE('',*,*,#13794,.T.);
#19460=ORIENTED_EDGE('',*,*,#13599,.T.);
#19461=ORIENTED_EDGE('',*,*,#13795,.T.);
#19462=ORIENTED_EDGE('',*,*,#13796,.F.);
#19463=ORIENTED_EDGE('',*,*,#13797,.T.);
#19464=ORIENTED_EDGE('',*,*,#13671,.F.);
#19465=ORIENTED_EDGE('',*,*,#13794,.F.);
#19466=ORIENTED_EDGE('',*,*,#13669,.F.);
#19467=ORIENTED_EDGE('',*,*,#13798,.T.);
#19468=ORIENTED_EDGE('',*,*,#13598,.F.);
#19469=ORIENTED_EDGE('',*,*,#13799,.T.);
#19470=ORIENTED_EDGE('',*,*,#13800,.F.);
#19471=ORIENTED_EDGE('',*,*,#13801,.F.);
#19472=ORIENTED_EDGE('',*,*,#13795,.F.);
#19473=ORIENTED_EDGE('',*,*,#13668,.T.);
#19474=ORIENTED_EDGE('',*,*,#13798,.F.);
#19475=ORIENTED_EDGE('',*,*,#13674,.T.);
#19476=ORIENTED_EDGE('',*,*,#13802,.T.);
#19477=ORIENTED_EDGE('',*,*,#13603,.T.);
#19478=ORIENTED_EDGE('',*,*,#13803,.T.);
#19479=ORIENTED_EDGE('',*,*,#13804,.F.);
#19480=ORIENTED_EDGE('',*,*,#13805,.T.);
#19481=ORIENTED_EDGE('',*,*,#13675,.F.);
#19482=ORIENTED_EDGE('',*,*,#13802,.F.);
#19483=ORIENTED_EDGE('',*,*,#13673,.F.);
#19484=ORIENTED_EDGE('',*,*,#13806,.T.);
#19485=ORIENTED_EDGE('',*,*,#13602,.F.);
#19486=ORIENTED_EDGE('',*,*,#13807,.T.);
#19487=ORIENTED_EDGE('',*,*,#13808,.F.);
#19488=ORIENTED_EDGE('',*,*,#13809,.F.);
#19489=ORIENTED_EDGE('',*,*,#13803,.F.);
#19490=ORIENTED_EDGE('',*,*,#13672,.T.);
#19491=ORIENTED_EDGE('',*,*,#13806,.F.);
#19492=ORIENTED_EDGE('',*,*,#13677,.T.);
#19493=ORIENTED_EDGE('',*,*,#13810,.F.);
#19494=ORIENTED_EDGE('',*,*,#13679,.T.);
#19495=ORIENTED_EDGE('',*,*,#13811,.T.);
#19496=ORIENTED_EDGE('',*,*,#13606,.T.);
#19497=ORIENTED_EDGE('',*,*,#13812,.T.);
#19498=ORIENTED_EDGE('',*,*,#13813,.F.);
#19499=ORIENTED_EDGE('',*,*,#13814,.T.);
#19500=ORIENTED_EDGE('',*,*,#13678,.F.);
#19501=ORIENTED_EDGE('',*,*,#13810,.T.);
#19502=ORIENTED_EDGE('',*,*,#13676,.F.);
#19503=ORIENTED_EDGE('',*,*,#13811,.F.);
#19504=ORIENTED_EDGE('',*,*,#13605,.F.);
#19505=ORIENTED_EDGE('',*,*,#13815,.T.);
#19506=ORIENTED_EDGE('',*,*,#13816,.F.);
#19507=ORIENTED_EDGE('',*,*,#13817,.F.);
#19508=ORIENTED_EDGE('',*,*,#13812,.F.);
#19509=ORIENTED_EDGE('',*,*,#13541,.T.);
#19510=ORIENTED_EDGE('',*,*,#13818,.F.);
#19511=ORIENTED_EDGE('',*,*,#13819,.F.);
#19512=ORIENTED_EDGE('',*,*,#13687,.F.);
#19513=ORIENTED_EDGE('',*,*,#13544,.F.);
#19514=ORIENTED_EDGE('',*,*,#13685,.F.);
#19515=ORIENTED_EDGE('',*,*,#13820,.F.);
#19516=ORIENTED_EDGE('',*,*,#13821,.F.);
#19517=ORIENTED_EDGE('',*,*,#13818,.T.);
#19518=ORIENTED_EDGE('',*,*,#13822,.F.);
#19519=ORIENTED_EDGE('',*,*,#13823,.T.);
#19520=ORIENTED_EDGE('',*,*,#13824,.T.);
#19521=ORIENTED_EDGE('',*,*,#13825,.T.);
#19522=ORIENTED_EDGE('',*,*,#13740,.T.);
#19523=ORIENTED_EDGE('',*,*,#13745,.T.);
#19524=ORIENTED_EDGE('',*,*,#13826,.T.);
#19525=ORIENTED_EDGE('',*,*,#13827,.T.);
#19526=ORIENTED_EDGE('',*,*,#13732,.T.);
#19527=ORIENTED_EDGE('',*,*,#13737,.T.);
#19528=ORIENTED_EDGE('',*,*,#13828,.T.);
#19529=ORIENTED_EDGE('',*,*,#13829,.T.);
#19530=ORIENTED_EDGE('',*,*,#13724,.T.);
#19531=ORIENTED_EDGE('',*,*,#13729,.T.);
#19532=ORIENTED_EDGE('',*,*,#13830,.T.);
#19533=ORIENTED_EDGE('',*,*,#13831,.T.);
#19534=ORIENTED_EDGE('',*,*,#13716,.T.);
#19535=ORIENTED_EDGE('',*,*,#13721,.T.);
#19536=ORIENTED_EDGE('',*,*,#13832,.T.);
#19537=ORIENTED_EDGE('',*,*,#13833,.T.);
#19538=ORIENTED_EDGE('',*,*,#13708,.T.);
#19539=ORIENTED_EDGE('',*,*,#13713,.T.);
#19540=ORIENTED_EDGE('',*,*,#13834,.T.);
#19541=ORIENTED_EDGE('',*,*,#13835,.T.);
#19542=ORIENTED_EDGE('',*,*,#13700,.T.);
#19543=ORIENTED_EDGE('',*,*,#13705,.T.);
#19544=ORIENTED_EDGE('',*,*,#13836,.T.);
#19545=ORIENTED_EDGE('',*,*,#13837,.T.);
#19546=ORIENTED_EDGE('',*,*,#13692,.T.);
#19547=ORIENTED_EDGE('',*,*,#13697,.T.);
#19548=ORIENTED_EDGE('',*,*,#13838,.T.);
#19549=ORIENTED_EDGE('',*,*,#13820,.T.);
#19550=ORIENTED_EDGE('',*,*,#13684,.T.);
#19551=ORIENTED_EDGE('',*,*,#13689,.T.);
#19552=ORIENTED_EDGE('',*,*,#13839,.T.);
#19553=ORIENTED_EDGE('',*,*,#13840,.T.);
#19554=ORIENTED_EDGE('',*,*,#13813,.T.);
#19555=ORIENTED_EDGE('',*,*,#13817,.T.);
#19556=ORIENTED_EDGE('',*,*,#13841,.T.);
#19557=ORIENTED_EDGE('',*,*,#13842,.T.);
#19558=ORIENTED_EDGE('',*,*,#13804,.T.);
#19559=ORIENTED_EDGE('',*,*,#13809,.T.);
#19560=ORIENTED_EDGE('',*,*,#13843,.T.);
#19561=ORIENTED_EDGE('',*,*,#13844,.T.);
#19562=ORIENTED_EDGE('',*,*,#13796,.T.);
#19563=ORIENTED_EDGE('',*,*,#13801,.T.);
#19564=ORIENTED_EDGE('',*,*,#13845,.T.);
#19565=ORIENTED_EDGE('',*,*,#13846,.T.);
#19566=ORIENTED_EDGE('',*,*,#13788,.T.);
#19567=ORIENTED_EDGE('',*,*,#13793,.T.);
#19568=ORIENTED_EDGE('',*,*,#13847,.T.);
#19569=ORIENTED_EDGE('',*,*,#13848,.T.);
#19570=ORIENTED_EDGE('',*,*,#13780,.T.);
#19571=ORIENTED_EDGE('',*,*,#13785,.T.);
#19572=ORIENTED_EDGE('',*,*,#13849,.T.);
#19573=ORIENTED_EDGE('',*,*,#13850,.T.);
#19574=ORIENTED_EDGE('',*,*,#13772,.T.);
#19575=ORIENTED_EDGE('',*,*,#13777,.T.);
#19576=ORIENTED_EDGE('',*,*,#13851,.T.);
#19577=ORIENTED_EDGE('',*,*,#13852,.T.);
#19578=ORIENTED_EDGE('',*,*,#13764,.T.);
#19579=ORIENTED_EDGE('',*,*,#13769,.T.);
#19580=ORIENTED_EDGE('',*,*,#13853,.T.);
#19581=ORIENTED_EDGE('',*,*,#13854,.T.);
#19582=ORIENTED_EDGE('',*,*,#13756,.T.);
#19583=ORIENTED_EDGE('',*,*,#13761,.T.);
#19584=ORIENTED_EDGE('',*,*,#13855,.T.);
#19585=ORIENTED_EDGE('',*,*,#13856,.T.);
#19586=ORIENTED_EDGE('',*,*,#13748,.T.);
#19587=ORIENTED_EDGE('',*,*,#13753,.T.);
#19588=ORIENTED_EDGE('',*,*,#13857,.T.);
#19589=ORIENTED_EDGE('',*,*,#13823,.F.);
#19590=ORIENTED_EDGE('',*,*,#13545,.T.);
#19591=ORIENTED_EDGE('',*,*,#13858,.F.);
#19592=ORIENTED_EDGE('',*,*,#13859,.F.);
#19593=ORIENTED_EDGE('',*,*,#13695,.F.);
#19594=ORIENTED_EDGE('',*,*,#13548,.F.);
#19595=ORIENTED_EDGE('',*,*,#13693,.F.);
#19596=ORIENTED_EDGE('',*,*,#13837,.F.);
#19597=ORIENTED_EDGE('',*,*,#13860,.F.);
#19598=ORIENTED_EDGE('',*,*,#13858,.T.);
#19599=ORIENTED_EDGE('',*,*,#13549,.T.);
#19600=ORIENTED_EDGE('',*,*,#13861,.F.);
#19601=ORIENTED_EDGE('',*,*,#13862,.F.);
#19602=ORIENTED_EDGE('',*,*,#13703,.F.);
#19603=ORIENTED_EDGE('',*,*,#13552,.F.);
#19604=ORIENTED_EDGE('',*,*,#13701,.F.);
#19605=ORIENTED_EDGE('',*,*,#13835,.F.);
#19606=ORIENTED_EDGE('',*,*,#13863,.F.);
#19607=ORIENTED_EDGE('',*,*,#13861,.T.);
#19608=ORIENTED_EDGE('',*,*,#13553,.T.);
#19609=ORIENTED_EDGE('',*,*,#13864,.F.);
#19610=ORIENTED_EDGE('',*,*,#13865,.F.);
#19611=ORIENTED_EDGE('',*,*,#13711,.F.);
#19612=ORIENTED_EDGE('',*,*,#13556,.F.);
#19613=ORIENTED_EDGE('',*,*,#13709,.F.);
#19614=ORIENTED_EDGE('',*,*,#13833,.F.);
#19615=ORIENTED_EDGE('',*,*,#13866,.F.);
#19616=ORIENTED_EDGE('',*,*,#13864,.T.);
#19617=ORIENTED_EDGE('',*,*,#13557,.T.);
#19618=ORIENTED_EDGE('',*,*,#13867,.F.);
#19619=ORIENTED_EDGE('',*,*,#13868,.F.);
#19620=ORIENTED_EDGE('',*,*,#13719,.F.);
#19621=ORIENTED_EDGE('',*,*,#13560,.F.);
#19622=ORIENTED_EDGE('',*,*,#13717,.F.);
#19623=ORIENTED_EDGE('',*,*,#13831,.F.);
#19624=ORIENTED_EDGE('',*,*,#13869,.F.);
#19625=ORIENTED_EDGE('',*,*,#13867,.T.);
#19626=ORIENTED_EDGE('',*,*,#13561,.T.);
#19627=ORIENTED_EDGE('',*,*,#13870,.F.);
#19628=ORIENTED_EDGE('',*,*,#13871,.F.);
#19629=ORIENTED_EDGE('',*,*,#13727,.F.);
#19630=ORIENTED_EDGE('',*,*,#13564,.F.);
#19631=ORIENTED_EDGE('',*,*,#13725,.F.);
#19632=ORIENTED_EDGE('',*,*,#13829,.F.);
#19633=ORIENTED_EDGE('',*,*,#13872,.F.);
#19634=ORIENTED_EDGE('',*,*,#13870,.T.);
#19635=ORIENTED_EDGE('',*,*,#13565,.T.);
#19636=ORIENTED_EDGE('',*,*,#13873,.F.);
#19637=ORIENTED_EDGE('',*,*,#13874,.F.);
#19638=ORIENTED_EDGE('',*,*,#13735,.F.);
#19639=ORIENTED_EDGE('',*,*,#13568,.F.);
#19640=ORIENTED_EDGE('',*,*,#13733,.F.);
#19641=ORIENTED_EDGE('',*,*,#13827,.F.);
#19642=ORIENTED_EDGE('',*,*,#13875,.F.);
#19643=ORIENTED_EDGE('',*,*,#13873,.T.);
#19644=ORIENTED_EDGE('',*,*,#13569,.T.);
#19645=ORIENTED_EDGE('',*,*,#13876,.F.);
#19646=ORIENTED_EDGE('',*,*,#13877,.F.);
#19647=ORIENTED_EDGE('',*,*,#13743,.F.);
#19648=ORIENTED_EDGE('',*,*,#13572,.F.);
#19649=ORIENTED_EDGE('',*,*,#13741,.F.);
#19650=ORIENTED_EDGE('',*,*,#13825,.F.);
#19651=ORIENTED_EDGE('',*,*,#13878,.F.);
#19652=ORIENTED_EDGE('',*,*,#13876,.T.);
#19653=ORIENTED_EDGE('',*,*,#13573,.T.);
#19654=ORIENTED_EDGE('',*,*,#13879,.F.);
#19655=ORIENTED_EDGE('',*,*,#13880,.F.);
#19656=ORIENTED_EDGE('',*,*,#13751,.F.);
#19657=ORIENTED_EDGE('',*,*,#13576,.F.);
#19658=ORIENTED_EDGE('',*,*,#13749,.F.);
#19659=ORIENTED_EDGE('',*,*,#13856,.F.);
#19660=ORIENTED_EDGE('',*,*,#13881,.F.);
#19661=ORIENTED_EDGE('',*,*,#13879,.T.);
#19662=ORIENTED_EDGE('',*,*,#13577,.T.);
#19663=ORIENTED_EDGE('',*,*,#13882,.F.);
#19664=ORIENTED_EDGE('',*,*,#13883,.F.);
#19665=ORIENTED_EDGE('',*,*,#13759,.F.);
#19666=ORIENTED_EDGE('',*,*,#13580,.F.);
#19667=ORIENTED_EDGE('',*,*,#13757,.F.);
#19668=ORIENTED_EDGE('',*,*,#13854,.F.);
#19669=ORIENTED_EDGE('',*,*,#13884,.F.);
#19670=ORIENTED_EDGE('',*,*,#13882,.T.);
#19671=ORIENTED_EDGE('',*,*,#13581,.T.);
#19672=ORIENTED_EDGE('',*,*,#13885,.F.);
#19673=ORIENTED_EDGE('',*,*,#13886,.F.);
#19674=ORIENTED_EDGE('',*,*,#13767,.F.);
#19675=ORIENTED_EDGE('',*,*,#13584,.F.);
#19676=ORIENTED_EDGE('',*,*,#13765,.F.);
#19677=ORIENTED_EDGE('',*,*,#13852,.F.);
#19678=ORIENTED_EDGE('',*,*,#13887,.F.);
#19679=ORIENTED_EDGE('',*,*,#13885,.T.);
#19680=ORIENTED_EDGE('',*,*,#13585,.T.);
#19681=ORIENTED_EDGE('',*,*,#13888,.F.);
#19682=ORIENTED_EDGE('',*,*,#13889,.F.);
#19683=ORIENTED_EDGE('',*,*,#13775,.F.);
#19684=ORIENTED_EDGE('',*,*,#13588,.F.);
#19685=ORIENTED_EDGE('',*,*,#13773,.F.);
#19686=ORIENTED_EDGE('',*,*,#13850,.F.);
#19687=ORIENTED_EDGE('',*,*,#13890,.F.);
#19688=ORIENTED_EDGE('',*,*,#13888,.T.);
#19689=ORIENTED_EDGE('',*,*,#13589,.T.);
#19690=ORIENTED_EDGE('',*,*,#13891,.F.);
#19691=ORIENTED_EDGE('',*,*,#13892,.F.);
#19692=ORIENTED_EDGE('',*,*,#13783,.F.);
#19693=ORIENTED_EDGE('',*,*,#13592,.F.);
#19694=ORIENTED_EDGE('',*,*,#13781,.F.);
#19695=ORIENTED_EDGE('',*,*,#13848,.F.);
#19696=ORIENTED_EDGE('',*,*,#13893,.F.);
#19697=ORIENTED_EDGE('',*,*,#13891,.T.);
#19698=ORIENTED_EDGE('',*,*,#13593,.T.);
#19699=ORIENTED_EDGE('',*,*,#13894,.F.);
#19700=ORIENTED_EDGE('',*,*,#13895,.F.);
#19701=ORIENTED_EDGE('',*,*,#13791,.F.);
#19702=ORIENTED_EDGE('',*,*,#13596,.F.);
#19703=ORIENTED_EDGE('',*,*,#13789,.F.);
#19704=ORIENTED_EDGE('',*,*,#13846,.F.);
#19705=ORIENTED_EDGE('',*,*,#13896,.F.);
#19706=ORIENTED_EDGE('',*,*,#13894,.T.);
#19707=ORIENTED_EDGE('',*,*,#13597,.T.);
#19708=ORIENTED_EDGE('',*,*,#13897,.F.);
#19709=ORIENTED_EDGE('',*,*,#13898,.F.);
#19710=ORIENTED_EDGE('',*,*,#13799,.F.);
#19711=ORIENTED_EDGE('',*,*,#13600,.F.);
#19712=ORIENTED_EDGE('',*,*,#13797,.F.);
#19713=ORIENTED_EDGE('',*,*,#13844,.F.);
#19714=ORIENTED_EDGE('',*,*,#13899,.F.);
#19715=ORIENTED_EDGE('',*,*,#13897,.T.);
#19716=ORIENTED_EDGE('',*,*,#13601,.T.);
#19717=ORIENTED_EDGE('',*,*,#13900,.F.);
#19718=ORIENTED_EDGE('',*,*,#13901,.F.);
#19719=ORIENTED_EDGE('',*,*,#13807,.F.);
#19720=ORIENTED_EDGE('',*,*,#13604,.F.);
#19721=ORIENTED_EDGE('',*,*,#13805,.F.);
#19722=ORIENTED_EDGE('',*,*,#13842,.F.);
#19723=ORIENTED_EDGE('',*,*,#13902,.F.);
#19724=ORIENTED_EDGE('',*,*,#13900,.T.);
#19725=ORIENTED_EDGE('',*,*,#13607,.F.);
#19726=ORIENTED_EDGE('',*,*,#13814,.F.);
#19727=ORIENTED_EDGE('',*,*,#13840,.F.);
#19728=ORIENTED_EDGE('',*,*,#13903,.F.);
#19729=ORIENTED_EDGE('',*,*,#13904,.T.);
#19730=ORIENTED_EDGE('',*,*,#13608,.T.);
#19731=ORIENTED_EDGE('',*,*,#13904,.F.);
#19732=ORIENTED_EDGE('',*,*,#13905,.F.);
#19733=ORIENTED_EDGE('',*,*,#13815,.F.);
#19734=ORIENTED_EDGE('',*,*,#13906,.T.);
#19735=ORIENTED_EDGE('',*,*,#13907,.T.);
#19736=ORIENTED_EDGE('',*,*,#13908,.F.);
#19737=ORIENTED_EDGE('',*,*,#13907,.F.);
#19738=ORIENTED_EDGE('',*,*,#13909,.F.);
#19739=ORIENTED_EDGE('',*,*,#13908,.T.);
#19740=ORIENTED_EDGE('',*,*,#13910,.F.);
#19741=ORIENTED_EDGE('',*,*,#13911,.T.);
#19742=ORIENTED_EDGE('',*,*,#13909,.T.);
#19743=ORIENTED_EDGE('',*,*,#13911,.F.);
#19744=ORIENTED_EDGE('',*,*,#13912,.F.);
#19745=ORIENTED_EDGE('',*,*,#13913,.T.);
#19746=ORIENTED_EDGE('',*,*,#13910,.T.);
#19747=ORIENTED_EDGE('',*,*,#13913,.F.);
#19748=ORIENTED_EDGE('',*,*,#13912,.T.);
#19749=ORIENTED_EDGE('',*,*,#13821,.T.);
#19750=ORIENTED_EDGE('',*,*,#13838,.F.);
#19751=ORIENTED_EDGE('',*,*,#13696,.T.);
#19752=ORIENTED_EDGE('',*,*,#13859,.T.);
#19753=ORIENTED_EDGE('',*,*,#13860,.T.);
#19754=ORIENTED_EDGE('',*,*,#13836,.F.);
#19755=ORIENTED_EDGE('',*,*,#13704,.T.);
#19756=ORIENTED_EDGE('',*,*,#13862,.T.);
#19757=ORIENTED_EDGE('',*,*,#13863,.T.);
#19758=ORIENTED_EDGE('',*,*,#13834,.F.);
#19759=ORIENTED_EDGE('',*,*,#13712,.T.);
#19760=ORIENTED_EDGE('',*,*,#13865,.T.);
#19761=ORIENTED_EDGE('',*,*,#13866,.T.);
#19762=ORIENTED_EDGE('',*,*,#13832,.F.);
#19763=ORIENTED_EDGE('',*,*,#13720,.T.);
#19764=ORIENTED_EDGE('',*,*,#13868,.T.);
#19765=ORIENTED_EDGE('',*,*,#13869,.T.);
#19766=ORIENTED_EDGE('',*,*,#13830,.F.);
#19767=ORIENTED_EDGE('',*,*,#13728,.T.);
#19768=ORIENTED_EDGE('',*,*,#13871,.T.);
#19769=ORIENTED_EDGE('',*,*,#13872,.T.);
#19770=ORIENTED_EDGE('',*,*,#13828,.F.);
#19771=ORIENTED_EDGE('',*,*,#13736,.T.);
#19772=ORIENTED_EDGE('',*,*,#13874,.T.);
#19773=ORIENTED_EDGE('',*,*,#13875,.T.);
#19774=ORIENTED_EDGE('',*,*,#13826,.F.);
#19775=ORIENTED_EDGE('',*,*,#13744,.T.);
#19776=ORIENTED_EDGE('',*,*,#13877,.T.);
#19777=ORIENTED_EDGE('',*,*,#13878,.T.);
#19778=ORIENTED_EDGE('',*,*,#13824,.F.);
#19779=ORIENTED_EDGE('',*,*,#13857,.F.);
#19780=ORIENTED_EDGE('',*,*,#13752,.T.);
#19781=ORIENTED_EDGE('',*,*,#13880,.T.);
#19782=ORIENTED_EDGE('',*,*,#13881,.T.);
#19783=ORIENTED_EDGE('',*,*,#13855,.F.);
#19784=ORIENTED_EDGE('',*,*,#13760,.T.);
#19785=ORIENTED_EDGE('',*,*,#13883,.T.);
#19786=ORIENTED_EDGE('',*,*,#13884,.T.);
#19787=ORIENTED_EDGE('',*,*,#13853,.F.);
#19788=ORIENTED_EDGE('',*,*,#13768,.T.);
#19789=ORIENTED_EDGE('',*,*,#13886,.T.);
#19790=ORIENTED_EDGE('',*,*,#13887,.T.);
#19791=ORIENTED_EDGE('',*,*,#13851,.F.);
#19792=ORIENTED_EDGE('',*,*,#13776,.T.);
#19793=ORIENTED_EDGE('',*,*,#13889,.T.);
#19794=ORIENTED_EDGE('',*,*,#13890,.T.);
#19795=ORIENTED_EDGE('',*,*,#13849,.F.);
#19796=ORIENTED_EDGE('',*,*,#13784,.T.);
#19797=ORIENTED_EDGE('',*,*,#13892,.T.);
#19798=ORIENTED_EDGE('',*,*,#13893,.T.);
#19799=ORIENTED_EDGE('',*,*,#13847,.F.);
#19800=ORIENTED_EDGE('',*,*,#13792,.T.);
#19801=ORIENTED_EDGE('',*,*,#13895,.T.);
#19802=ORIENTED_EDGE('',*,*,#13896,.T.);
#19803=ORIENTED_EDGE('',*,*,#13845,.F.);
#19804=ORIENTED_EDGE('',*,*,#13800,.T.);
#19805=ORIENTED_EDGE('',*,*,#13898,.T.);
#19806=ORIENTED_EDGE('',*,*,#13899,.T.);
#19807=ORIENTED_EDGE('',*,*,#13843,.F.);
#19808=ORIENTED_EDGE('',*,*,#13808,.T.);
#19809=ORIENTED_EDGE('',*,*,#13901,.T.);
#19810=ORIENTED_EDGE('',*,*,#13902,.T.);
#19811=ORIENTED_EDGE('',*,*,#13841,.F.);
#19812=ORIENTED_EDGE('',*,*,#13816,.T.);
#19813=ORIENTED_EDGE('',*,*,#13905,.T.);
#19814=ORIENTED_EDGE('',*,*,#13903,.T.);
#19815=ORIENTED_EDGE('',*,*,#13839,.F.);
#19816=ORIENTED_EDGE('',*,*,#13688,.T.);
#19817=ORIENTED_EDGE('',*,*,#13819,.T.);
#19818=ORIENTED_EDGE('',*,*,#13914,.F.);
#19819=ORIENTED_EDGE('',*,*,#13822,.T.);
#19820=ORIENTED_EDGE('',*,*,#13915,.F.);
#19821=ORIENTED_EDGE('',*,*,#13916,.T.);
#19822=ORIENTED_EDGE('',*,*,#13914,.T.);
#19823=ORIENTED_EDGE('',*,*,#13916,.F.);
#19824=ORIENTED_EDGE('',*,*,#13915,.T.);
#19825=ORIENTED_EDGE('',*,*,#13917,.F.);
#19826=ORIENTED_EDGE('',*,*,#13917,.T.);
#19827=ORIENTED_EDGE('',*,*,#13918,.T.);
#19828=ORIENTED_EDGE('',*,*,#13919,.F.);
#19829=ORIENTED_EDGE('',*,*,#13918,.F.);
#19830=ORIENTED_EDGE('',*,*,#13919,.T.);
#19831=ORIENTED_EDGE('',*,*,#13920,.T.);
#19832=ORIENTED_EDGE('',*,*,#13906,.F.);
#19833=ORIENTED_EDGE('',*,*,#13920,.F.);
#19834=ORIENTED_EDGE('',*,*,#13921,.T.);
#19835=ORIENTED_EDGE('',*,*,#13922,.T.);
#19836=ORIENTED_EDGE('',*,*,#13923,.F.);
#19837=ORIENTED_EDGE('',*,*,#13922,.F.);
#19838=ORIENTED_EDGE('',*,*,#13924,.F.);
#19839=ORIENTED_EDGE('',*,*,#13923,.T.);
#19840=ORIENTED_EDGE('',*,*,#13925,.F.);
#19841=ORIENTED_EDGE('',*,*,#13926,.T.);
#19842=ORIENTED_EDGE('',*,*,#13924,.T.);
#19843=ORIENTED_EDGE('',*,*,#13926,.F.);
#19844=ORIENTED_EDGE('',*,*,#13927,.F.);
#19845=ORIENTED_EDGE('',*,*,#13928,.T.);
#19846=ORIENTED_EDGE('',*,*,#13925,.T.);
#19847=ORIENTED_EDGE('',*,*,#13928,.F.);
#19848=ORIENTED_EDGE('',*,*,#13929,.F.);
#19849=ORIENTED_EDGE('',*,*,#13930,.T.);
#19850=ORIENTED_EDGE('',*,*,#13927,.T.);
#19851=ORIENTED_EDGE('',*,*,#13930,.F.);
#19852=ORIENTED_EDGE('',*,*,#13929,.T.);
#19853=ORIENTED_EDGE('',*,*,#13931,.F.);
#19854=ORIENTED_EDGE('',*,*,#13931,.T.);
#19855=ORIENTED_EDGE('',*,*,#13932,.T.);
#19856=ORIENTED_EDGE('',*,*,#13933,.F.);
#19857=ORIENTED_EDGE('',*,*,#13932,.F.);
#19858=ORIENTED_EDGE('',*,*,#13933,.T.);
#19859=ORIENTED_EDGE('',*,*,#13934,.T.);
#19860=ORIENTED_EDGE('',*,*,#13921,.F.);
#19861=ORIENTED_EDGE('',*,*,#13934,.F.);
#19862=ORIENTED_EDGE('',*,*,#13935,.F.);
#19863=ORIENTED_EDGE('',*,*,#13936,.T.);
#19864=ORIENTED_EDGE('',*,*,#13937,.F.);
#19865=ORIENTED_EDGE('',*,*,#13936,.F.);
#19866=ORIENTED_EDGE('',*,*,#13938,.F.);
#19867=ORIENTED_EDGE('',*,*,#13939,.T.);
#19868=ORIENTED_EDGE('',*,*,#13940,.F.);
#19869=ORIENTED_EDGE('',*,*,#13939,.F.);
#19870=ORIENTED_EDGE('',*,*,#13941,.F.);
#19871=ORIENTED_EDGE('',*,*,#13942,.T.);
#19872=ORIENTED_EDGE('',*,*,#13943,.F.);
#19873=ORIENTED_EDGE('',*,*,#13944,.F.);
#19874=ORIENTED_EDGE('',*,*,#13945,.T.);
#19875=ORIENTED_EDGE('',*,*,#13944,.T.);
#19876=ORIENTED_EDGE('',*,*,#13946,.F.);
#19877=ORIENTED_EDGE('',*,*,#13947,.F.);
#19878=ORIENTED_EDGE('',*,*,#13948,.F.);
#19879=ORIENTED_EDGE('',*,*,#13947,.T.);
#19880=ORIENTED_EDGE('',*,*,#13949,.F.);
#19881=ORIENTED_EDGE('',*,*,#13950,.F.);
#19882=ORIENTED_EDGE('',*,*,#13951,.F.);
#19883=ORIENTED_EDGE('',*,*,#13950,.T.);
#19884=ORIENTED_EDGE('',*,*,#13952,.F.);
#19885=ORIENTED_EDGE('',*,*,#13953,.F.);
#19886=ORIENTED_EDGE('',*,*,#13954,.F.);
#19887=ORIENTED_EDGE('',*,*,#13953,.T.);
#19888=ORIENTED_EDGE('',*,*,#13955,.F.);
#19889=ORIENTED_EDGE('',*,*,#13956,.F.);
#19890=ORIENTED_EDGE('',*,*,#13957,.T.);
#19891=ORIENTED_EDGE('',*,*,#13956,.T.);
#19892=ORIENTED_EDGE('',*,*,#13958,.F.);
#19893=ORIENTED_EDGE('',*,*,#13959,.F.);
#19894=ORIENTED_EDGE('',*,*,#13960,.F.);
#19895=ORIENTED_EDGE('',*,*,#13959,.T.);
#19896=ORIENTED_EDGE('',*,*,#13961,.F.);
#19897=ORIENTED_EDGE('',*,*,#13962,.F.);
#19898=ORIENTED_EDGE('',*,*,#13963,.T.);
#19899=ORIENTED_EDGE('',*,*,#13962,.T.);
#19900=ORIENTED_EDGE('',*,*,#13964,.F.);
#19901=ORIENTED_EDGE('',*,*,#13942,.F.);
#19902=ORIENTED_EDGE('',*,*,#13964,.T.);
#19903=ORIENTED_EDGE('',*,*,#13961,.T.);
#19904=ORIENTED_EDGE('',*,*,#13958,.T.);
#19905=ORIENTED_EDGE('',*,*,#13955,.T.);
#19906=ORIENTED_EDGE('',*,*,#13952,.T.);
#19907=ORIENTED_EDGE('',*,*,#13949,.T.);
#19908=ORIENTED_EDGE('',*,*,#13946,.T.);
#19909=ORIENTED_EDGE('',*,*,#13943,.T.);
#19910=ORIENTED_EDGE('',*,*,#13935,.T.);
#19911=ORIENTED_EDGE('',*,*,#13938,.T.);
#19912=ORIENTED_EDGE('',*,*,#13963,.F.);
#19913=ORIENTED_EDGE('',*,*,#13941,.T.);
#19914=ORIENTED_EDGE('',*,*,#13945,.F.);
#19915=ORIENTED_EDGE('',*,*,#13948,.T.);
#19916=ORIENTED_EDGE('',*,*,#13951,.T.);
#19917=ORIENTED_EDGE('',*,*,#13954,.T.);
#19918=ORIENTED_EDGE('',*,*,#13957,.F.);
#19919=ORIENTED_EDGE('',*,*,#13960,.T.);
#19920=ORIENTED_EDGE('',*,*,#13937,.T.);
#19921=ORIENTED_EDGE('',*,*,#13940,.T.);
#19922=ORIENTED_EDGE('',*,*,#13965,.F.);
#19923=ORIENTED_EDGE('',*,*,#13966,.T.);
#19924=ORIENTED_EDGE('',*,*,#13967,.T.);
#19925=ORIENTED_EDGE('',*,*,#13968,.T.);
#19926=ORIENTED_EDGE('',*,*,#13969,.T.);
#19927=ORIENTED_EDGE('',*,*,#13968,.F.);
#19928=ORIENTED_EDGE('',*,*,#13970,.T.);
#19929=ORIENTED_EDGE('',*,*,#13971,.T.);
#19930=ORIENTED_EDGE('',*,*,#13972,.F.);
#19931=ORIENTED_EDGE('',*,*,#13973,.T.);
#19932=ORIENTED_EDGE('',*,*,#13965,.T.);
#19933=ORIENTED_EDGE('',*,*,#13974,.T.);
#19934=ORIENTED_EDGE('',*,*,#13975,.F.);
#19935=ORIENTED_EDGE('',*,*,#13976,.T.);
#19936=ORIENTED_EDGE('',*,*,#13972,.T.);
#19937=ORIENTED_EDGE('',*,*,#13977,.T.);
#19938=ORIENTED_EDGE('',*,*,#13978,.F.);
#19939=ORIENTED_EDGE('',*,*,#13979,.T.);
#19940=ORIENTED_EDGE('',*,*,#13975,.T.);
#19941=ORIENTED_EDGE('',*,*,#13980,.T.);
#19942=ORIENTED_EDGE('',*,*,#13981,.F.);
#19943=ORIENTED_EDGE('',*,*,#13982,.T.);
#19944=ORIENTED_EDGE('',*,*,#13978,.T.);
#19945=ORIENTED_EDGE('',*,*,#13983,.T.);
#19946=ORIENTED_EDGE('',*,*,#13984,.F.);
#19947=ORIENTED_EDGE('',*,*,#13985,.T.);
#19948=ORIENTED_EDGE('',*,*,#13981,.T.);
#19949=ORIENTED_EDGE('',*,*,#13986,.T.);
#19950=ORIENTED_EDGE('',*,*,#13987,.F.);
#19951=ORIENTED_EDGE('',*,*,#13988,.T.);
#19952=ORIENTED_EDGE('',*,*,#13984,.T.);
#19953=ORIENTED_EDGE('',*,*,#13989,.T.);
#19954=ORIENTED_EDGE('',*,*,#13990,.F.);
#19955=ORIENTED_EDGE('',*,*,#13991,.T.);
#19956=ORIENTED_EDGE('',*,*,#13987,.T.);
#19957=ORIENTED_EDGE('',*,*,#13992,.T.);
#19958=ORIENTED_EDGE('',*,*,#13993,.F.);
#19959=ORIENTED_EDGE('',*,*,#13994,.T.);
#19960=ORIENTED_EDGE('',*,*,#13990,.T.);
#19961=ORIENTED_EDGE('',*,*,#13995,.T.);
#19962=ORIENTED_EDGE('',*,*,#13996,.F.);
#19963=ORIENTED_EDGE('',*,*,#13997,.T.);
#19964=ORIENTED_EDGE('',*,*,#13993,.T.);
#19965=ORIENTED_EDGE('',*,*,#13998,.T.);
#19966=ORIENTED_EDGE('',*,*,#13999,.F.);
#19967=ORIENTED_EDGE('',*,*,#14000,.T.);
#19968=ORIENTED_EDGE('',*,*,#13996,.T.);
#19969=ORIENTED_EDGE('',*,*,#14001,.T.);
#19970=ORIENTED_EDGE('',*,*,#14002,.F.);
#19971=ORIENTED_EDGE('',*,*,#14003,.T.);
#19972=ORIENTED_EDGE('',*,*,#13999,.T.);
#19973=ORIENTED_EDGE('',*,*,#14004,.T.);
#19974=ORIENTED_EDGE('',*,*,#14005,.F.);
#19975=ORIENTED_EDGE('',*,*,#14006,.T.);
#19976=ORIENTED_EDGE('',*,*,#14002,.T.);
#19977=ORIENTED_EDGE('',*,*,#14007,.T.);
#19978=ORIENTED_EDGE('',*,*,#14008,.F.);
#19979=ORIENTED_EDGE('',*,*,#14009,.T.);
#19980=ORIENTED_EDGE('',*,*,#14005,.T.);
#19981=ORIENTED_EDGE('',*,*,#14010,.T.);
#19982=ORIENTED_EDGE('',*,*,#14011,.F.);
#19983=ORIENTED_EDGE('',*,*,#14012,.T.);
#19984=ORIENTED_EDGE('',*,*,#14008,.T.);
#19985=ORIENTED_EDGE('',*,*,#14013,.T.);
#19986=ORIENTED_EDGE('',*,*,#14014,.F.);
#19987=ORIENTED_EDGE('',*,*,#14015,.T.);
#19988=ORIENTED_EDGE('',*,*,#14011,.T.);
#19989=ORIENTED_EDGE('',*,*,#14016,.T.);
#19990=ORIENTED_EDGE('',*,*,#14017,.F.);
#19991=ORIENTED_EDGE('',*,*,#14018,.T.);
#19992=ORIENTED_EDGE('',*,*,#14014,.T.);
#19993=ORIENTED_EDGE('',*,*,#14019,.T.);
#19994=ORIENTED_EDGE('',*,*,#14020,.F.);
#19995=ORIENTED_EDGE('',*,*,#14021,.T.);
#19996=ORIENTED_EDGE('',*,*,#14017,.T.);
#19997=ORIENTED_EDGE('',*,*,#14022,.T.);
#19998=ORIENTED_EDGE('',*,*,#14023,.F.);
#19999=ORIENTED_EDGE('',*,*,#14024,.T.);
#20000=ORIENTED_EDGE('',*,*,#14020,.T.);
#20001=ORIENTED_EDGE('',*,*,#14025,.T.);
#20002=ORIENTED_EDGE('',*,*,#14026,.F.);
#20003=ORIENTED_EDGE('',*,*,#14027,.T.);
#20004=ORIENTED_EDGE('',*,*,#14023,.T.);
#20005=ORIENTED_EDGE('',*,*,#14028,.T.);
#20006=ORIENTED_EDGE('',*,*,#14029,.F.);
#20007=ORIENTED_EDGE('',*,*,#14030,.T.);
#20008=ORIENTED_EDGE('',*,*,#14026,.T.);
#20009=ORIENTED_EDGE('',*,*,#14031,.T.);
#20010=ORIENTED_EDGE('',*,*,#14032,.F.);
#20011=ORIENTED_EDGE('',*,*,#14033,.T.);
#20012=ORIENTED_EDGE('',*,*,#14029,.T.);
#20013=ORIENTED_EDGE('',*,*,#14034,.T.);
#20014=ORIENTED_EDGE('',*,*,#14035,.F.);
#20015=ORIENTED_EDGE('',*,*,#14036,.F.);
#20016=ORIENTED_EDGE('',*,*,#14037,.T.);
#20017=ORIENTED_EDGE('',*,*,#14032,.T.);
#20018=ORIENTED_EDGE('',*,*,#14038,.T.);
#20019=ORIENTED_EDGE('',*,*,#14039,.F.);
#20020=ORIENTED_EDGE('',*,*,#14040,.T.);
#20021=ORIENTED_EDGE('',*,*,#14041,.F.);
#20022=ORIENTED_EDGE('',*,*,#14042,.F.);
#20023=ORIENTED_EDGE('',*,*,#14043,.F.);
#20024=ORIENTED_EDGE('',*,*,#14044,.T.);
#20025=ORIENTED_EDGE('',*,*,#14039,.T.);
#20026=ORIENTED_EDGE('',*,*,#14045,.F.);
#20027=ORIENTED_EDGE('',*,*,#14046,.F.);
#20028=ORIENTED_EDGE('',*,*,#14047,.T.);
#20029=ORIENTED_EDGE('',*,*,#14043,.T.);
#20030=ORIENTED_EDGE('',*,*,#14048,.F.);
#20031=ORIENTED_EDGE('',*,*,#14049,.F.);
#20032=ORIENTED_EDGE('',*,*,#14050,.T.);
#20033=ORIENTED_EDGE('',*,*,#14046,.T.);
#20034=ORIENTED_EDGE('',*,*,#14051,.F.);
#20035=ORIENTED_EDGE('',*,*,#14052,.F.);
#20036=ORIENTED_EDGE('',*,*,#14053,.T.);
#20037=ORIENTED_EDGE('',*,*,#14049,.T.);
#20038=ORIENTED_EDGE('',*,*,#14054,.F.);
#20039=ORIENTED_EDGE('',*,*,#14055,.F.);
#20040=ORIENTED_EDGE('',*,*,#14056,.T.);
#20041=ORIENTED_EDGE('',*,*,#14052,.T.);
#20042=ORIENTED_EDGE('',*,*,#14057,.F.);
#20043=ORIENTED_EDGE('',*,*,#14058,.F.);
#20044=ORIENTED_EDGE('',*,*,#14059,.T.);
#20045=ORIENTED_EDGE('',*,*,#14055,.T.);
#20046=ORIENTED_EDGE('',*,*,#14060,.F.);
#20047=ORIENTED_EDGE('',*,*,#14061,.F.);
#20048=ORIENTED_EDGE('',*,*,#14062,.T.);
#20049=ORIENTED_EDGE('',*,*,#14058,.T.);
#20050=ORIENTED_EDGE('',*,*,#14063,.F.);
#20051=ORIENTED_EDGE('',*,*,#14064,.F.);
#20052=ORIENTED_EDGE('',*,*,#14065,.T.);
#20053=ORIENTED_EDGE('',*,*,#14061,.T.);
#20054=ORIENTED_EDGE('',*,*,#14066,.F.);
#20055=ORIENTED_EDGE('',*,*,#14067,.F.);
#20056=ORIENTED_EDGE('',*,*,#14068,.T.);
#20057=ORIENTED_EDGE('',*,*,#14064,.T.);
#20058=ORIENTED_EDGE('',*,*,#14069,.F.);
#20059=ORIENTED_EDGE('',*,*,#14070,.F.);
#20060=ORIENTED_EDGE('',*,*,#14071,.T.);
#20061=ORIENTED_EDGE('',*,*,#14067,.T.);
#20062=ORIENTED_EDGE('',*,*,#14072,.F.);
#20063=ORIENTED_EDGE('',*,*,#14073,.F.);
#20064=ORIENTED_EDGE('',*,*,#14074,.T.);
#20065=ORIENTED_EDGE('',*,*,#14070,.T.);
#20066=ORIENTED_EDGE('',*,*,#14075,.F.);
#20067=ORIENTED_EDGE('',*,*,#14076,.F.);
#20068=ORIENTED_EDGE('',*,*,#14077,.T.);
#20069=ORIENTED_EDGE('',*,*,#14073,.T.);
#20070=ORIENTED_EDGE('',*,*,#14078,.F.);
#20071=ORIENTED_EDGE('',*,*,#14079,.F.);
#20072=ORIENTED_EDGE('',*,*,#14080,.T.);
#20073=ORIENTED_EDGE('',*,*,#14076,.T.);
#20074=ORIENTED_EDGE('',*,*,#14081,.F.);
#20075=ORIENTED_EDGE('',*,*,#14082,.F.);
#20076=ORIENTED_EDGE('',*,*,#14083,.T.);
#20077=ORIENTED_EDGE('',*,*,#14079,.T.);
#20078=ORIENTED_EDGE('',*,*,#14084,.F.);
#20079=ORIENTED_EDGE('',*,*,#14085,.F.);
#20080=ORIENTED_EDGE('',*,*,#14086,.T.);
#20081=ORIENTED_EDGE('',*,*,#14082,.T.);
#20082=ORIENTED_EDGE('',*,*,#14087,.F.);
#20083=ORIENTED_EDGE('',*,*,#14088,.F.);
#20084=ORIENTED_EDGE('',*,*,#14089,.T.);
#20085=ORIENTED_EDGE('',*,*,#14085,.T.);
#20086=ORIENTED_EDGE('',*,*,#14090,.F.);
#20087=ORIENTED_EDGE('',*,*,#14091,.F.);
#20088=ORIENTED_EDGE('',*,*,#14092,.T.);
#20089=ORIENTED_EDGE('',*,*,#14088,.T.);
#20090=ORIENTED_EDGE('',*,*,#14093,.F.);
#20091=ORIENTED_EDGE('',*,*,#14094,.F.);
#20092=ORIENTED_EDGE('',*,*,#14095,.T.);
#20093=ORIENTED_EDGE('',*,*,#14091,.T.);
#20094=ORIENTED_EDGE('',*,*,#14096,.F.);
#20095=ORIENTED_EDGE('',*,*,#14097,.F.);
#20096=ORIENTED_EDGE('',*,*,#14098,.T.);
#20097=ORIENTED_EDGE('',*,*,#14094,.T.);
#20098=ORIENTED_EDGE('',*,*,#14099,.F.);
#20099=ORIENTED_EDGE('',*,*,#14100,.F.);
#20100=ORIENTED_EDGE('',*,*,#14101,.T.);
#20101=ORIENTED_EDGE('',*,*,#14097,.T.);
#20102=ORIENTED_EDGE('',*,*,#14102,.F.);
#20103=ORIENTED_EDGE('',*,*,#14103,.F.);
#20104=ORIENTED_EDGE('',*,*,#14104,.T.);
#20105=ORIENTED_EDGE('',*,*,#14100,.T.);
#20106=ORIENTED_EDGE('',*,*,#14105,.F.);
#20107=ORIENTED_EDGE('',*,*,#14041,.T.);
#20108=ORIENTED_EDGE('',*,*,#14106,.T.);
#20109=ORIENTED_EDGE('',*,*,#14107,.F.);
#20110=ORIENTED_EDGE('',*,*,#14108,.T.);
#20111=ORIENTED_EDGE('',*,*,#14108,.F.);
#20112=ORIENTED_EDGE('',*,*,#14109,.F.);
#20113=ORIENTED_EDGE('',*,*,#14038,.F.);
#20114=ORIENTED_EDGE('',*,*,#14034,.F.);
#20115=ORIENTED_EDGE('',*,*,#14031,.F.);
#20116=ORIENTED_EDGE('',*,*,#14028,.F.);
#20117=ORIENTED_EDGE('',*,*,#14025,.F.);
#20118=ORIENTED_EDGE('',*,*,#14022,.F.);
#20119=ORIENTED_EDGE('',*,*,#14019,.F.);
#20120=ORIENTED_EDGE('',*,*,#14016,.F.);
#20121=ORIENTED_EDGE('',*,*,#14013,.F.);
#20122=ORIENTED_EDGE('',*,*,#14010,.F.);
#20123=ORIENTED_EDGE('',*,*,#14007,.F.);
#20124=ORIENTED_EDGE('',*,*,#14004,.F.);
#20125=ORIENTED_EDGE('',*,*,#14001,.F.);
#20126=ORIENTED_EDGE('',*,*,#13998,.F.);
#20127=ORIENTED_EDGE('',*,*,#13995,.F.);
#20128=ORIENTED_EDGE('',*,*,#13992,.F.);
#20129=ORIENTED_EDGE('',*,*,#13989,.F.);
#20130=ORIENTED_EDGE('',*,*,#13986,.F.);
#20131=ORIENTED_EDGE('',*,*,#13983,.F.);
#20132=ORIENTED_EDGE('',*,*,#13980,.F.);
#20133=ORIENTED_EDGE('',*,*,#13977,.F.);
#20134=ORIENTED_EDGE('',*,*,#13974,.F.);
#20135=ORIENTED_EDGE('',*,*,#13971,.F.);
#20136=ORIENTED_EDGE('',*,*,#14110,.F.);
#20137=ORIENTED_EDGE('',*,*,#14111,.T.);
#20138=ORIENTED_EDGE('',*,*,#14105,.T.);
#20139=ORIENTED_EDGE('',*,*,#14102,.T.);
#20140=ORIENTED_EDGE('',*,*,#14099,.T.);
#20141=ORIENTED_EDGE('',*,*,#14096,.T.);
#20142=ORIENTED_EDGE('',*,*,#14093,.T.);
#20143=ORIENTED_EDGE('',*,*,#14090,.T.);
#20144=ORIENTED_EDGE('',*,*,#14087,.T.);
#20145=ORIENTED_EDGE('',*,*,#14084,.T.);
#20146=ORIENTED_EDGE('',*,*,#14081,.T.);
#20147=ORIENTED_EDGE('',*,*,#14078,.T.);
#20148=ORIENTED_EDGE('',*,*,#14075,.T.);
#20149=ORIENTED_EDGE('',*,*,#14072,.T.);
#20150=ORIENTED_EDGE('',*,*,#14069,.T.);
#20151=ORIENTED_EDGE('',*,*,#14066,.T.);
#20152=ORIENTED_EDGE('',*,*,#14063,.T.);
#20153=ORIENTED_EDGE('',*,*,#14060,.T.);
#20154=ORIENTED_EDGE('',*,*,#14057,.T.);
#20155=ORIENTED_EDGE('',*,*,#14054,.T.);
#20156=ORIENTED_EDGE('',*,*,#14051,.T.);
#20157=ORIENTED_EDGE('',*,*,#14048,.T.);
#20158=ORIENTED_EDGE('',*,*,#14045,.T.);
#20159=ORIENTED_EDGE('',*,*,#14042,.T.);
#20160=ORIENTED_EDGE('',*,*,#13967,.F.);
#20161=ORIENTED_EDGE('',*,*,#14112,.T.);
#20162=ORIENTED_EDGE('',*,*,#14113,.T.);
#20163=ORIENTED_EDGE('',*,*,#14110,.T.);
#20164=ORIENTED_EDGE('',*,*,#13970,.F.);
#20165=ORIENTED_EDGE('',*,*,#14103,.T.);
#20166=ORIENTED_EDGE('',*,*,#14111,.F.);
#20167=ORIENTED_EDGE('',*,*,#14113,.F.);
#20168=ORIENTED_EDGE('',*,*,#14114,.T.);
#20169=ORIENTED_EDGE('',*,*,#14106,.F.);
#20170=ORIENTED_EDGE('',*,*,#14040,.F.);
#20171=ORIENTED_EDGE('',*,*,#14044,.F.);
#20172=ORIENTED_EDGE('',*,*,#14047,.F.);
#20173=ORIENTED_EDGE('',*,*,#14050,.F.);
#20174=ORIENTED_EDGE('',*,*,#14053,.F.);
#20175=ORIENTED_EDGE('',*,*,#14056,.F.);
#20176=ORIENTED_EDGE('',*,*,#14059,.F.);
#20177=ORIENTED_EDGE('',*,*,#14062,.F.);
#20178=ORIENTED_EDGE('',*,*,#14065,.F.);
#20179=ORIENTED_EDGE('',*,*,#14068,.F.);
#20180=ORIENTED_EDGE('',*,*,#14071,.F.);
#20181=ORIENTED_EDGE('',*,*,#14074,.F.);
#20182=ORIENTED_EDGE('',*,*,#14077,.F.);
#20183=ORIENTED_EDGE('',*,*,#14080,.F.);
#20184=ORIENTED_EDGE('',*,*,#14083,.F.);
#20185=ORIENTED_EDGE('',*,*,#14086,.F.);
#20186=ORIENTED_EDGE('',*,*,#14089,.F.);
#20187=ORIENTED_EDGE('',*,*,#14092,.F.);
#20188=ORIENTED_EDGE('',*,*,#14095,.F.);
#20189=ORIENTED_EDGE('',*,*,#14098,.F.);
#20190=ORIENTED_EDGE('',*,*,#14101,.F.);
#20191=ORIENTED_EDGE('',*,*,#14104,.F.);
#20192=ORIENTED_EDGE('',*,*,#14114,.F.);
#20193=ORIENTED_EDGE('',*,*,#14112,.F.);
#20194=ORIENTED_EDGE('',*,*,#13966,.F.);
#20195=ORIENTED_EDGE('',*,*,#13973,.F.);
#20196=ORIENTED_EDGE('',*,*,#13976,.F.);
#20197=ORIENTED_EDGE('',*,*,#13979,.F.);
#20198=ORIENTED_EDGE('',*,*,#13982,.F.);
#20199=ORIENTED_EDGE('',*,*,#13985,.F.);
#20200=ORIENTED_EDGE('',*,*,#13988,.F.);
#20201=ORIENTED_EDGE('',*,*,#13991,.F.);
#20202=ORIENTED_EDGE('',*,*,#13994,.F.);
#20203=ORIENTED_EDGE('',*,*,#13997,.F.);
#20204=ORIENTED_EDGE('',*,*,#14000,.F.);
#20205=ORIENTED_EDGE('',*,*,#14003,.F.);
#20206=ORIENTED_EDGE('',*,*,#14006,.F.);
#20207=ORIENTED_EDGE('',*,*,#14009,.F.);
#20208=ORIENTED_EDGE('',*,*,#14012,.F.);
#20209=ORIENTED_EDGE('',*,*,#14015,.F.);
#20210=ORIENTED_EDGE('',*,*,#14018,.F.);
#20211=ORIENTED_EDGE('',*,*,#14021,.F.);
#20212=ORIENTED_EDGE('',*,*,#14024,.F.);
#20213=ORIENTED_EDGE('',*,*,#14027,.F.);
#20214=ORIENTED_EDGE('',*,*,#14030,.F.);
#20215=ORIENTED_EDGE('',*,*,#14033,.F.);
#20216=ORIENTED_EDGE('',*,*,#14037,.F.);
#20217=ORIENTED_EDGE('',*,*,#14035,.T.);
#20218=ORIENTED_EDGE('',*,*,#14109,.T.);
#20219=ORIENTED_EDGE('',*,*,#14115,.F.);
#20220=ORIENTED_EDGE('',*,*,#14036,.T.);
#20221=ORIENTED_EDGE('',*,*,#14116,.T.);
#20222=ORIENTED_EDGE('',*,*,#14117,.T.);
#20223=ORIENTED_EDGE('',*,*,#14116,.F.);
#20224=ORIENTED_EDGE('',*,*,#14115,.T.);
#20225=ORIENTED_EDGE('',*,*,#14107,.T.);
#20226=ORIENTED_EDGE('',*,*,#14118,.F.);
#20227=ORIENTED_EDGE('',*,*,#14117,.F.);
#20228=ORIENTED_EDGE('',*,*,#14119,.T.);
#20229=ORIENTED_EDGE('',*,*,#14120,.F.);
#20230=ORIENTED_EDGE('',*,*,#14119,.F.);
#20231=ORIENTED_EDGE('',*,*,#14121,.F.);
#20232=ORIENTED_EDGE('',*,*,#14122,.T.);
#20233=ORIENTED_EDGE('',*,*,#14123,.T.);
#20234=ORIENTED_EDGE('',*,*,#14124,.F.);
#20235=ORIENTED_EDGE('',*,*,#14125,.F.);
#20236=ORIENTED_EDGE('',*,*,#14126,.T.);
#20237=ORIENTED_EDGE('',*,*,#14127,.T.);
#20238=ORIENTED_EDGE('',*,*,#14122,.F.);
#20239=ORIENTED_EDGE('',*,*,#14128,.F.);
#20240=ORIENTED_EDGE('',*,*,#14129,.T.);
#20241=ORIENTED_EDGE('',*,*,#14130,.T.);
#20242=ORIENTED_EDGE('',*,*,#14126,.F.);
#20243=ORIENTED_EDGE('',*,*,#14131,.F.);
#20244=ORIENTED_EDGE('',*,*,#14132,.T.);
#20245=ORIENTED_EDGE('',*,*,#14133,.T.);
#20246=ORIENTED_EDGE('',*,*,#14129,.F.);
#20247=ORIENTED_EDGE('',*,*,#14134,.F.);
#20248=ORIENTED_EDGE('',*,*,#14135,.T.);
#20249=ORIENTED_EDGE('',*,*,#14136,.T.);
#20250=ORIENTED_EDGE('',*,*,#14132,.F.);
#20251=ORIENTED_EDGE('',*,*,#14137,.F.);
#20252=ORIENTED_EDGE('',*,*,#14124,.T.);
#20253=ORIENTED_EDGE('',*,*,#14138,.T.);
#20254=ORIENTED_EDGE('',*,*,#14135,.F.);
#20255=ORIENTED_EDGE('',*,*,#14138,.F.);
#20256=ORIENTED_EDGE('',*,*,#14123,.F.);
#20257=ORIENTED_EDGE('',*,*,#14127,.F.);
#20258=ORIENTED_EDGE('',*,*,#14130,.F.);
#20259=ORIENTED_EDGE('',*,*,#14133,.F.);
#20260=ORIENTED_EDGE('',*,*,#14136,.F.);
#20261=ORIENTED_EDGE('',*,*,#14120,.T.);
#20262=ORIENTED_EDGE('',*,*,#14139,.F.);
#20263=ORIENTED_EDGE('',*,*,#14140,.T.);
#20264=ORIENTED_EDGE('',*,*,#14141,.F.);
#20265=ORIENTED_EDGE('',*,*,#14142,.F.);
#20266=ORIENTED_EDGE('',*,*,#14143,.F.);
#20267=ORIENTED_EDGE('',*,*,#14142,.T.);
#20268=ORIENTED_EDGE('',*,*,#14144,.T.);
#20269=ORIENTED_EDGE('',*,*,#14145,.F.);
#20270=ORIENTED_EDGE('',*,*,#14144,.F.);
#20271=ORIENTED_EDGE('',*,*,#14141,.T.);
#20272=ORIENTED_EDGE('',*,*,#14146,.T.);
#20273=ORIENTED_EDGE('',*,*,#14147,.F.);
#20274=ORIENTED_EDGE('',*,*,#14146,.F.);
#20275=ORIENTED_EDGE('',*,*,#14140,.F.);
#20276=ORIENTED_EDGE('',*,*,#14148,.F.);
#20277=ORIENTED_EDGE('',*,*,#14149,.T.);
#20278=ORIENTED_EDGE('',*,*,#14150,.F.);
#20279=ORIENTED_EDGE('',*,*,#14151,.F.);
#20280=ORIENTED_EDGE('',*,*,#14152,.F.);
#20281=ORIENTED_EDGE('',*,*,#14151,.T.);
#20282=ORIENTED_EDGE('',*,*,#14153,.T.);
#20283=ORIENTED_EDGE('',*,*,#14154,.F.);
#20284=ORIENTED_EDGE('',*,*,#14153,.F.);
#20285=ORIENTED_EDGE('',*,*,#14150,.T.);
#20286=ORIENTED_EDGE('',*,*,#14155,.T.);
#20287=ORIENTED_EDGE('',*,*,#14156,.F.);
#20288=ORIENTED_EDGE('',*,*,#14155,.F.);
#20289=ORIENTED_EDGE('',*,*,#14149,.F.);
#20290=ORIENTED_EDGE('',*,*,#14157,.F.);
#20291=ORIENTED_EDGE('',*,*,#14158,.T.);
#20292=ORIENTED_EDGE('',*,*,#14159,.F.);
#20293=ORIENTED_EDGE('',*,*,#14160,.F.);
#20294=ORIENTED_EDGE('',*,*,#14161,.F.);
#20295=ORIENTED_EDGE('',*,*,#14160,.T.);
#20296=ORIENTED_EDGE('',*,*,#14162,.T.);
#20297=ORIENTED_EDGE('',*,*,#14163,.F.);
#20298=ORIENTED_EDGE('',*,*,#14162,.F.);
#20299=ORIENTED_EDGE('',*,*,#14159,.T.);
#20300=ORIENTED_EDGE('',*,*,#14164,.T.);
#20301=ORIENTED_EDGE('',*,*,#14165,.F.);
#20302=ORIENTED_EDGE('',*,*,#14164,.F.);
#20303=ORIENTED_EDGE('',*,*,#14158,.F.);
#20304=ORIENTED_EDGE('',*,*,#14166,.F.);
#20305=ORIENTED_EDGE('',*,*,#14167,.T.);
#20306=ORIENTED_EDGE('',*,*,#14168,.F.);
#20307=ORIENTED_EDGE('',*,*,#14169,.F.);
#20308=ORIENTED_EDGE('',*,*,#14170,.F.);
#20309=ORIENTED_EDGE('',*,*,#14169,.T.);
#20310=ORIENTED_EDGE('',*,*,#14171,.T.);
#20311=ORIENTED_EDGE('',*,*,#14172,.F.);
#20312=ORIENTED_EDGE('',*,*,#14171,.F.);
#20313=ORIENTED_EDGE('',*,*,#14168,.T.);
#20314=ORIENTED_EDGE('',*,*,#14173,.T.);
#20315=ORIENTED_EDGE('',*,*,#14174,.F.);
#20316=ORIENTED_EDGE('',*,*,#14173,.F.);
#20317=ORIENTED_EDGE('',*,*,#14167,.F.);
#20318=ORIENTED_EDGE('',*,*,#14175,.F.);
#20319=ORIENTED_EDGE('',*,*,#14176,.T.);
#20320=ORIENTED_EDGE('',*,*,#14177,.F.);
#20321=ORIENTED_EDGE('',*,*,#14178,.F.);
#20322=ORIENTED_EDGE('',*,*,#14179,.F.);
#20323=ORIENTED_EDGE('',*,*,#14178,.T.);
#20324=ORIENTED_EDGE('',*,*,#14180,.T.);
#20325=ORIENTED_EDGE('',*,*,#14181,.F.);
#20326=ORIENTED_EDGE('',*,*,#14180,.F.);
#20327=ORIENTED_EDGE('',*,*,#14177,.T.);
#20328=ORIENTED_EDGE('',*,*,#14182,.T.);
#20329=ORIENTED_EDGE('',*,*,#14183,.F.);
#20330=ORIENTED_EDGE('',*,*,#14182,.F.);
#20331=ORIENTED_EDGE('',*,*,#14176,.F.);
#20332=ORIENTED_EDGE('',*,*,#14184,.F.);
#20333=ORIENTED_EDGE('',*,*,#14185,.T.);
#20334=ORIENTED_EDGE('',*,*,#14186,.F.);
#20335=ORIENTED_EDGE('',*,*,#14187,.F.);
#20336=ORIENTED_EDGE('',*,*,#14188,.F.);
#20337=ORIENTED_EDGE('',*,*,#14187,.T.);
#20338=ORIENTED_EDGE('',*,*,#14189,.T.);
#20339=ORIENTED_EDGE('',*,*,#14190,.F.);
#20340=ORIENTED_EDGE('',*,*,#14189,.F.);
#20341=ORIENTED_EDGE('',*,*,#14186,.T.);
#20342=ORIENTED_EDGE('',*,*,#14191,.T.);
#20343=ORIENTED_EDGE('',*,*,#14192,.F.);
#20344=ORIENTED_EDGE('',*,*,#14191,.F.);
#20345=ORIENTED_EDGE('',*,*,#14185,.F.);
#20346=ORIENTED_EDGE('',*,*,#14193,.F.);
#20347=ORIENTED_EDGE('',*,*,#14194,.T.);
#20348=ORIENTED_EDGE('',*,*,#14195,.F.);
#20349=ORIENTED_EDGE('',*,*,#14196,.F.);
#20350=ORIENTED_EDGE('',*,*,#14197,.F.);
#20351=ORIENTED_EDGE('',*,*,#14196,.T.);
#20352=ORIENTED_EDGE('',*,*,#14198,.T.);
#20353=ORIENTED_EDGE('',*,*,#14199,.F.);
#20354=ORIENTED_EDGE('',*,*,#14198,.F.);
#20355=ORIENTED_EDGE('',*,*,#14195,.T.);
#20356=ORIENTED_EDGE('',*,*,#14200,.T.);
#20357=ORIENTED_EDGE('',*,*,#14201,.F.);
#20358=ORIENTED_EDGE('',*,*,#14200,.F.);
#20359=ORIENTED_EDGE('',*,*,#14194,.F.);
#20360=ORIENTED_EDGE('',*,*,#14202,.F.);
#20361=ORIENTED_EDGE('',*,*,#14203,.T.);
#20362=ORIENTED_EDGE('',*,*,#14204,.F.);
#20363=ORIENTED_EDGE('',*,*,#14205,.F.);
#20364=ORIENTED_EDGE('',*,*,#14206,.F.);
#20365=ORIENTED_EDGE('',*,*,#14205,.T.);
#20366=ORIENTED_EDGE('',*,*,#14207,.T.);
#20367=ORIENTED_EDGE('',*,*,#14208,.F.);
#20368=ORIENTED_EDGE('',*,*,#14207,.F.);
#20369=ORIENTED_EDGE('',*,*,#14204,.T.);
#20370=ORIENTED_EDGE('',*,*,#14209,.T.);
#20371=ORIENTED_EDGE('',*,*,#14210,.F.);
#20372=ORIENTED_EDGE('',*,*,#14209,.F.);
#20373=ORIENTED_EDGE('',*,*,#14203,.F.);
#20374=ORIENTED_EDGE('',*,*,#14211,.F.);
#20375=ORIENTED_EDGE('',*,*,#14212,.T.);
#20376=ORIENTED_EDGE('',*,*,#14213,.F.);
#20377=ORIENTED_EDGE('',*,*,#14214,.F.);
#20378=ORIENTED_EDGE('',*,*,#14215,.F.);
#20379=ORIENTED_EDGE('',*,*,#14214,.T.);
#20380=ORIENTED_EDGE('',*,*,#14216,.T.);
#20381=ORIENTED_EDGE('',*,*,#14217,.F.);
#20382=ORIENTED_EDGE('',*,*,#14218,.F.);
#20383=ORIENTED_EDGE('',*,*,#14216,.F.);
#20384=ORIENTED_EDGE('',*,*,#14213,.T.);
#20385=ORIENTED_EDGE('',*,*,#14219,.T.);
#20386=ORIENTED_EDGE('',*,*,#14220,.F.);
#20387=ORIENTED_EDGE('',*,*,#14219,.F.);
#20388=ORIENTED_EDGE('',*,*,#14212,.F.);
#20389=ORIENTED_EDGE('',*,*,#14221,.F.);
#20390=ORIENTED_EDGE('',*,*,#14222,.F.);
#20391=ORIENTED_EDGE('',*,*,#14223,.T.);
#20392=ORIENTED_EDGE('',*,*,#14224,.F.);
#20393=ORIENTED_EDGE('',*,*,#14225,.F.);
#20394=ORIENTED_EDGE('',*,*,#14226,.F.);
#20395=ORIENTED_EDGE('',*,*,#14225,.T.);
#20396=ORIENTED_EDGE('',*,*,#14227,.T.);
#20397=ORIENTED_EDGE('',*,*,#14228,.F.);
#20398=ORIENTED_EDGE('',*,*,#14227,.F.);
#20399=ORIENTED_EDGE('',*,*,#14224,.T.);
#20400=ORIENTED_EDGE('',*,*,#14229,.T.);
#20401=ORIENTED_EDGE('',*,*,#14230,.F.);
#20402=ORIENTED_EDGE('',*,*,#14229,.F.);
#20403=ORIENTED_EDGE('',*,*,#14223,.F.);
#20404=ORIENTED_EDGE('',*,*,#14231,.F.);
#20405=ORIENTED_EDGE('',*,*,#14232,.T.);
#20406=ORIENTED_EDGE('',*,*,#14233,.F.);
#20407=ORIENTED_EDGE('',*,*,#14234,.F.);
#20408=ORIENTED_EDGE('',*,*,#14235,.F.);
#20409=ORIENTED_EDGE('',*,*,#14234,.T.);
#20410=ORIENTED_EDGE('',*,*,#14236,.T.);
#20411=ORIENTED_EDGE('',*,*,#14237,.F.);
#20412=ORIENTED_EDGE('',*,*,#14236,.F.);
#20413=ORIENTED_EDGE('',*,*,#14233,.T.);
#20414=ORIENTED_EDGE('',*,*,#14238,.T.);
#20415=ORIENTED_EDGE('',*,*,#14239,.F.);
#20416=ORIENTED_EDGE('',*,*,#14238,.F.);
#20417=ORIENTED_EDGE('',*,*,#14232,.F.);
#20418=ORIENTED_EDGE('',*,*,#14240,.F.);
#20419=ORIENTED_EDGE('',*,*,#14241,.T.);
#20420=ORIENTED_EDGE('',*,*,#14242,.F.);
#20421=ORIENTED_EDGE('',*,*,#14243,.F.);
#20422=ORIENTED_EDGE('',*,*,#14244,.F.);
#20423=ORIENTED_EDGE('',*,*,#14243,.T.);
#20424=ORIENTED_EDGE('',*,*,#14245,.T.);
#20425=ORIENTED_EDGE('',*,*,#14246,.F.);
#20426=ORIENTED_EDGE('',*,*,#14245,.F.);
#20427=ORIENTED_EDGE('',*,*,#14242,.T.);
#20428=ORIENTED_EDGE('',*,*,#14247,.T.);
#20429=ORIENTED_EDGE('',*,*,#14248,.F.);
#20430=ORIENTED_EDGE('',*,*,#14247,.F.);
#20431=ORIENTED_EDGE('',*,*,#14241,.F.);
#20432=ORIENTED_EDGE('',*,*,#14249,.F.);
#20433=ORIENTED_EDGE('',*,*,#14250,.T.);
#20434=ORIENTED_EDGE('',*,*,#14251,.F.);
#20435=ORIENTED_EDGE('',*,*,#14252,.F.);
#20436=ORIENTED_EDGE('',*,*,#14253,.F.);
#20437=ORIENTED_EDGE('',*,*,#14252,.T.);
#20438=ORIENTED_EDGE('',*,*,#14254,.T.);
#20439=ORIENTED_EDGE('',*,*,#14255,.F.);
#20440=ORIENTED_EDGE('',*,*,#14254,.F.);
#20441=ORIENTED_EDGE('',*,*,#14251,.T.);
#20442=ORIENTED_EDGE('',*,*,#14256,.T.);
#20443=ORIENTED_EDGE('',*,*,#14257,.F.);
#20444=ORIENTED_EDGE('',*,*,#14256,.F.);
#20445=ORIENTED_EDGE('',*,*,#14250,.F.);
#20446=ORIENTED_EDGE('',*,*,#14258,.F.);
#20447=ORIENTED_EDGE('',*,*,#14259,.T.);
#20448=ORIENTED_EDGE('',*,*,#14260,.F.);
#20449=ORIENTED_EDGE('',*,*,#14261,.F.);
#20450=ORIENTED_EDGE('',*,*,#14262,.F.);
#20451=ORIENTED_EDGE('',*,*,#14261,.T.);
#20452=ORIENTED_EDGE('',*,*,#14263,.T.);
#20453=ORIENTED_EDGE('',*,*,#14264,.F.);
#20454=ORIENTED_EDGE('',*,*,#14263,.F.);
#20455=ORIENTED_EDGE('',*,*,#14260,.T.);
#20456=ORIENTED_EDGE('',*,*,#14265,.T.);
#20457=ORIENTED_EDGE('',*,*,#14266,.F.);
#20458=ORIENTED_EDGE('',*,*,#14265,.F.);
#20459=ORIENTED_EDGE('',*,*,#14259,.F.);
#20460=ORIENTED_EDGE('',*,*,#14267,.F.);
#20461=ORIENTED_EDGE('',*,*,#14268,.T.);
#20462=ORIENTED_EDGE('',*,*,#14269,.F.);
#20463=ORIENTED_EDGE('',*,*,#14270,.F.);
#20464=ORIENTED_EDGE('',*,*,#14271,.F.);
#20465=ORIENTED_EDGE('',*,*,#14270,.T.);
#20466=ORIENTED_EDGE('',*,*,#14272,.T.);
#20467=ORIENTED_EDGE('',*,*,#14273,.F.);
#20468=ORIENTED_EDGE('',*,*,#14272,.F.);
#20469=ORIENTED_EDGE('',*,*,#14269,.T.);
#20470=ORIENTED_EDGE('',*,*,#14274,.T.);
#20471=ORIENTED_EDGE('',*,*,#14275,.F.);
#20472=ORIENTED_EDGE('',*,*,#14274,.F.);
#20473=ORIENTED_EDGE('',*,*,#14268,.F.);
#20474=ORIENTED_EDGE('',*,*,#14276,.F.);
#20475=ORIENTED_EDGE('',*,*,#14277,.T.);
#20476=ORIENTED_EDGE('',*,*,#14278,.F.);
#20477=ORIENTED_EDGE('',*,*,#14279,.F.);
#20478=ORIENTED_EDGE('',*,*,#14280,.F.);
#20479=ORIENTED_EDGE('',*,*,#14279,.T.);
#20480=ORIENTED_EDGE('',*,*,#14281,.T.);
#20481=ORIENTED_EDGE('',*,*,#14282,.F.);
#20482=ORIENTED_EDGE('',*,*,#14281,.F.);
#20483=ORIENTED_EDGE('',*,*,#14278,.T.);
#20484=ORIENTED_EDGE('',*,*,#14283,.T.);
#20485=ORIENTED_EDGE('',*,*,#14284,.F.);
#20486=ORIENTED_EDGE('',*,*,#14283,.F.);
#20487=ORIENTED_EDGE('',*,*,#14277,.F.);
#20488=ORIENTED_EDGE('',*,*,#14285,.F.);
#20489=ORIENTED_EDGE('',*,*,#14286,.T.);
#20490=ORIENTED_EDGE('',*,*,#14287,.F.);
#20491=ORIENTED_EDGE('',*,*,#14288,.F.);
#20492=ORIENTED_EDGE('',*,*,#14289,.F.);
#20493=ORIENTED_EDGE('',*,*,#14288,.T.);
#20494=ORIENTED_EDGE('',*,*,#14290,.T.);
#20495=ORIENTED_EDGE('',*,*,#14291,.F.);
#20496=ORIENTED_EDGE('',*,*,#14290,.F.);
#20497=ORIENTED_EDGE('',*,*,#14287,.T.);
#20498=ORIENTED_EDGE('',*,*,#14292,.T.);
#20499=ORIENTED_EDGE('',*,*,#14293,.F.);
#20500=ORIENTED_EDGE('',*,*,#14292,.F.);
#20501=ORIENTED_EDGE('',*,*,#14286,.F.);
#20502=ORIENTED_EDGE('',*,*,#14294,.F.);
#20503=ORIENTED_EDGE('',*,*,#14295,.T.);
#20504=ORIENTED_EDGE('',*,*,#14296,.F.);
#20505=ORIENTED_EDGE('',*,*,#14297,.F.);
#20506=ORIENTED_EDGE('',*,*,#14298,.F.);
#20507=ORIENTED_EDGE('',*,*,#14297,.T.);
#20508=ORIENTED_EDGE('',*,*,#14299,.T.);
#20509=ORIENTED_EDGE('',*,*,#14300,.F.);
#20510=ORIENTED_EDGE('',*,*,#14299,.F.);
#20511=ORIENTED_EDGE('',*,*,#14296,.T.);
#20512=ORIENTED_EDGE('',*,*,#14301,.T.);
#20513=ORIENTED_EDGE('',*,*,#14302,.F.);
#20514=ORIENTED_EDGE('',*,*,#14301,.F.);
#20515=ORIENTED_EDGE('',*,*,#14295,.F.);
#20516=ORIENTED_EDGE('',*,*,#14303,.F.);
#20517=ORIENTED_EDGE('',*,*,#14304,.T.);
#20518=ORIENTED_EDGE('',*,*,#14305,.F.);
#20519=ORIENTED_EDGE('',*,*,#14306,.F.);
#20520=ORIENTED_EDGE('',*,*,#14307,.F.);
#20521=ORIENTED_EDGE('',*,*,#14306,.T.);
#20522=ORIENTED_EDGE('',*,*,#14308,.T.);
#20523=ORIENTED_EDGE('',*,*,#14309,.F.);
#20524=ORIENTED_EDGE('',*,*,#14308,.F.);
#20525=ORIENTED_EDGE('',*,*,#14305,.T.);
#20526=ORIENTED_EDGE('',*,*,#14310,.T.);
#20527=ORIENTED_EDGE('',*,*,#14311,.F.);
#20528=ORIENTED_EDGE('',*,*,#14310,.F.);
#20529=ORIENTED_EDGE('',*,*,#14304,.F.);
#20530=ORIENTED_EDGE('',*,*,#14312,.F.);
#20531=ORIENTED_EDGE('',*,*,#14313,.T.);
#20532=ORIENTED_EDGE('',*,*,#14314,.F.);
#20533=ORIENTED_EDGE('',*,*,#14315,.F.);
#20534=ORIENTED_EDGE('',*,*,#14316,.F.);
#20535=ORIENTED_EDGE('',*,*,#14315,.T.);
#20536=ORIENTED_EDGE('',*,*,#14317,.T.);
#20537=ORIENTED_EDGE('',*,*,#14318,.F.);
#20538=ORIENTED_EDGE('',*,*,#14317,.F.);
#20539=ORIENTED_EDGE('',*,*,#14314,.T.);
#20540=ORIENTED_EDGE('',*,*,#14319,.T.);
#20541=ORIENTED_EDGE('',*,*,#14320,.F.);
#20542=ORIENTED_EDGE('',*,*,#14319,.F.);
#20543=ORIENTED_EDGE('',*,*,#14313,.F.);
#20544=ORIENTED_EDGE('',*,*,#14321,.F.);
#20545=ORIENTED_EDGE('',*,*,#14322,.T.);
#20546=ORIENTED_EDGE('',*,*,#14323,.F.);
#20547=ORIENTED_EDGE('',*,*,#14324,.F.);
#20548=ORIENTED_EDGE('',*,*,#14325,.F.);
#20549=ORIENTED_EDGE('',*,*,#14324,.T.);
#20550=ORIENTED_EDGE('',*,*,#14326,.T.);
#20551=ORIENTED_EDGE('',*,*,#14327,.F.);
#20552=ORIENTED_EDGE('',*,*,#14326,.F.);
#20553=ORIENTED_EDGE('',*,*,#14323,.T.);
#20554=ORIENTED_EDGE('',*,*,#14328,.T.);
#20555=ORIENTED_EDGE('',*,*,#14329,.F.);
#20556=ORIENTED_EDGE('',*,*,#14328,.F.);
#20557=ORIENTED_EDGE('',*,*,#14322,.F.);
#20558=ORIENTED_EDGE('',*,*,#14330,.F.);
#20559=ORIENTED_EDGE('',*,*,#14331,.T.);
#20560=ORIENTED_EDGE('',*,*,#14332,.F.);
#20561=ORIENTED_EDGE('',*,*,#14333,.F.);
#20562=ORIENTED_EDGE('',*,*,#14334,.F.);
#20563=ORIENTED_EDGE('',*,*,#14333,.T.);
#20564=ORIENTED_EDGE('',*,*,#14335,.T.);
#20565=ORIENTED_EDGE('',*,*,#14336,.F.);
#20566=ORIENTED_EDGE('',*,*,#14335,.F.);
#20567=ORIENTED_EDGE('',*,*,#14332,.T.);
#20568=ORIENTED_EDGE('',*,*,#14337,.T.);
#20569=ORIENTED_EDGE('',*,*,#14338,.F.);
#20570=ORIENTED_EDGE('',*,*,#14337,.F.);
#20571=ORIENTED_EDGE('',*,*,#14331,.F.);
#20572=ORIENTED_EDGE('',*,*,#14339,.F.);
#20573=ORIENTED_EDGE('',*,*,#14340,.T.);
#20574=ORIENTED_EDGE('',*,*,#14341,.F.);
#20575=ORIENTED_EDGE('',*,*,#14342,.F.);
#20576=ORIENTED_EDGE('',*,*,#14343,.F.);
#20577=ORIENTED_EDGE('',*,*,#14342,.T.);
#20578=ORIENTED_EDGE('',*,*,#14344,.T.);
#20579=ORIENTED_EDGE('',*,*,#14345,.F.);
#20580=ORIENTED_EDGE('',*,*,#14344,.F.);
#20581=ORIENTED_EDGE('',*,*,#14341,.T.);
#20582=ORIENTED_EDGE('',*,*,#14346,.T.);
#20583=ORIENTED_EDGE('',*,*,#14347,.F.);
#20584=ORIENTED_EDGE('',*,*,#14346,.F.);
#20585=ORIENTED_EDGE('',*,*,#14340,.F.);
#20586=ORIENTED_EDGE('',*,*,#14348,.F.);
#20587=ORIENTED_EDGE('',*,*,#14349,.T.);
#20588=ORIENTED_EDGE('',*,*,#14350,.F.);
#20589=ORIENTED_EDGE('',*,*,#14351,.F.);
#20590=ORIENTED_EDGE('',*,*,#14352,.F.);
#20591=ORIENTED_EDGE('',*,*,#14351,.T.);
#20592=ORIENTED_EDGE('',*,*,#14353,.T.);
#20593=ORIENTED_EDGE('',*,*,#14354,.F.);
#20594=ORIENTED_EDGE('',*,*,#14353,.F.);
#20595=ORIENTED_EDGE('',*,*,#14350,.T.);
#20596=ORIENTED_EDGE('',*,*,#14355,.T.);
#20597=ORIENTED_EDGE('',*,*,#14356,.F.);
#20598=ORIENTED_EDGE('',*,*,#14355,.F.);
#20599=ORIENTED_EDGE('',*,*,#14349,.F.);
#20600=ORIENTED_EDGE('',*,*,#14357,.F.);
#20601=ORIENTED_EDGE('',*,*,#14358,.T.);
#20602=ORIENTED_EDGE('',*,*,#14359,.F.);
#20603=ORIENTED_EDGE('',*,*,#14360,.F.);
#20604=ORIENTED_EDGE('',*,*,#14361,.F.);
#20605=ORIENTED_EDGE('',*,*,#14360,.T.);
#20606=ORIENTED_EDGE('',*,*,#14362,.T.);
#20607=ORIENTED_EDGE('',*,*,#14363,.F.);
#20608=ORIENTED_EDGE('',*,*,#14362,.F.);
#20609=ORIENTED_EDGE('',*,*,#14359,.T.);
#20610=ORIENTED_EDGE('',*,*,#14364,.T.);
#20611=ORIENTED_EDGE('',*,*,#14365,.F.);
#20612=ORIENTED_EDGE('',*,*,#14364,.F.);
#20613=ORIENTED_EDGE('',*,*,#14358,.F.);
#20614=ORIENTED_EDGE('',*,*,#14366,.F.);
#20615=ORIENTED_EDGE('',*,*,#14367,.T.);
#20616=ORIENTED_EDGE('',*,*,#14368,.F.);
#20617=ORIENTED_EDGE('',*,*,#14369,.F.);
#20618=ORIENTED_EDGE('',*,*,#14370,.F.);
#20619=ORIENTED_EDGE('',*,*,#14369,.T.);
#20620=ORIENTED_EDGE('',*,*,#14371,.T.);
#20621=ORIENTED_EDGE('',*,*,#14372,.F.);
#20622=ORIENTED_EDGE('',*,*,#14371,.F.);
#20623=ORIENTED_EDGE('',*,*,#14368,.T.);
#20624=ORIENTED_EDGE('',*,*,#14373,.T.);
#20625=ORIENTED_EDGE('',*,*,#14374,.F.);
#20626=ORIENTED_EDGE('',*,*,#14373,.F.);
#20627=ORIENTED_EDGE('',*,*,#14367,.F.);
#20628=ORIENTED_EDGE('',*,*,#14375,.F.);
#20629=ORIENTED_EDGE('',*,*,#14376,.T.);
#20630=ORIENTED_EDGE('',*,*,#14377,.T.);
#20631=ORIENTED_EDGE('',*,*,#14378,.F.);
#20632=ORIENTED_EDGE('',*,*,#14379,.T.);
#20633=ORIENTED_EDGE('',*,*,#14380,.F.);
#20634=ORIENTED_EDGE('',*,*,#14376,.F.);
#20635=ORIENTED_EDGE('',*,*,#14381,.F.);
#20636=ORIENTED_EDGE('',*,*,#14377,.F.);
#20637=ORIENTED_EDGE('',*,*,#14380,.T.);
#20638=ORIENTED_EDGE('',*,*,#14382,.T.);
#20639=ORIENTED_EDGE('',*,*,#14383,.F.);
#20640=ORIENTED_EDGE('',*,*,#14382,.F.);
#20641=ORIENTED_EDGE('',*,*,#14379,.F.);
#20642=ORIENTED_EDGE('',*,*,#14384,.F.);
#20643=ORIENTED_EDGE('',*,*,#14385,.T.);
#20644=ORIENTED_EDGE('',*,*,#14386,.F.);
#20645=ORIENTED_EDGE('',*,*,#14387,.F.);
#20646=ORIENTED_EDGE('',*,*,#14388,.F.);
#20647=ORIENTED_EDGE('',*,*,#14387,.T.);
#20648=ORIENTED_EDGE('',*,*,#14389,.T.);
#20649=ORIENTED_EDGE('',*,*,#14390,.F.);
#20650=ORIENTED_EDGE('',*,*,#14389,.F.);
#20651=ORIENTED_EDGE('',*,*,#14386,.T.);
#20652=ORIENTED_EDGE('',*,*,#14391,.T.);
#20653=ORIENTED_EDGE('',*,*,#14392,.F.);
#20654=ORIENTED_EDGE('',*,*,#14391,.F.);
#20655=ORIENTED_EDGE('',*,*,#14385,.F.);
#20656=ORIENTED_EDGE('',*,*,#14393,.F.);
#20657=ORIENTED_EDGE('',*,*,#14394,.T.);
#20658=ORIENTED_EDGE('',*,*,#14395,.F.);
#20659=ORIENTED_EDGE('',*,*,#14396,.F.);
#20660=ORIENTED_EDGE('',*,*,#14397,.F.);
#20661=ORIENTED_EDGE('',*,*,#14396,.T.);
#20662=ORIENTED_EDGE('',*,*,#14398,.T.);
#20663=ORIENTED_EDGE('',*,*,#14399,.F.);
#20664=ORIENTED_EDGE('',*,*,#14398,.F.);
#20665=ORIENTED_EDGE('',*,*,#14395,.T.);
#20666=ORIENTED_EDGE('',*,*,#14400,.T.);
#20667=ORIENTED_EDGE('',*,*,#14401,.F.);
#20668=ORIENTED_EDGE('',*,*,#14400,.F.);
#20669=ORIENTED_EDGE('',*,*,#14394,.F.);
#20670=ORIENTED_EDGE('',*,*,#14402,.F.);
#20671=ORIENTED_EDGE('',*,*,#14403,.T.);
#20672=ORIENTED_EDGE('',*,*,#14404,.F.);
#20673=ORIENTED_EDGE('',*,*,#14405,.F.);
#20674=ORIENTED_EDGE('',*,*,#14406,.F.);
#20675=ORIENTED_EDGE('',*,*,#14405,.T.);
#20676=ORIENTED_EDGE('',*,*,#14407,.T.);
#20677=ORIENTED_EDGE('',*,*,#14408,.F.);
#20678=ORIENTED_EDGE('',*,*,#14407,.F.);
#20679=ORIENTED_EDGE('',*,*,#14404,.T.);
#20680=ORIENTED_EDGE('',*,*,#14409,.T.);
#20681=ORIENTED_EDGE('',*,*,#14410,.F.);
#20682=ORIENTED_EDGE('',*,*,#14409,.F.);
#20683=ORIENTED_EDGE('',*,*,#14403,.F.);
#20684=ORIENTED_EDGE('',*,*,#14411,.F.);
#20685=ORIENTED_EDGE('',*,*,#14412,.T.);
#20686=ORIENTED_EDGE('',*,*,#14413,.F.);
#20687=ORIENTED_EDGE('',*,*,#14414,.F.);
#20688=ORIENTED_EDGE('',*,*,#14415,.F.);
#20689=ORIENTED_EDGE('',*,*,#14414,.T.);
#20690=ORIENTED_EDGE('',*,*,#14416,.T.);
#20691=ORIENTED_EDGE('',*,*,#14417,.F.);
#20692=ORIENTED_EDGE('',*,*,#14416,.F.);
#20693=ORIENTED_EDGE('',*,*,#14413,.T.);
#20694=ORIENTED_EDGE('',*,*,#14418,.T.);
#20695=ORIENTED_EDGE('',*,*,#14419,.F.);
#20696=ORIENTED_EDGE('',*,*,#14418,.F.);
#20697=ORIENTED_EDGE('',*,*,#14412,.F.);
#20698=ORIENTED_EDGE('',*,*,#14420,.F.);
#20699=ORIENTED_EDGE('',*,*,#14421,.T.);
#20700=ORIENTED_EDGE('',*,*,#14422,.F.);
#20701=ORIENTED_EDGE('',*,*,#14423,.F.);
#20702=ORIENTED_EDGE('',*,*,#14424,.F.);
#20703=ORIENTED_EDGE('',*,*,#14423,.T.);
#20704=ORIENTED_EDGE('',*,*,#14425,.T.);
#20705=ORIENTED_EDGE('',*,*,#14426,.F.);
#20706=ORIENTED_EDGE('',*,*,#14425,.F.);
#20707=ORIENTED_EDGE('',*,*,#14422,.T.);
#20708=ORIENTED_EDGE('',*,*,#14427,.T.);
#20709=ORIENTED_EDGE('',*,*,#14428,.F.);
#20710=ORIENTED_EDGE('',*,*,#14427,.F.);
#20711=ORIENTED_EDGE('',*,*,#14421,.F.);
#20712=ORIENTED_EDGE('',*,*,#14429,.F.);
#20713=ORIENTED_EDGE('',*,*,#14430,.T.);
#20714=ORIENTED_EDGE('',*,*,#14431,.F.);
#20715=ORIENTED_EDGE('',*,*,#14432,.F.);
#20716=ORIENTED_EDGE('',*,*,#14433,.F.);
#20717=ORIENTED_EDGE('',*,*,#14432,.T.);
#20718=ORIENTED_EDGE('',*,*,#14434,.T.);
#20719=ORIENTED_EDGE('',*,*,#14435,.F.);
#20720=ORIENTED_EDGE('',*,*,#14434,.F.);
#20721=ORIENTED_EDGE('',*,*,#14431,.T.);
#20722=ORIENTED_EDGE('',*,*,#14436,.T.);
#20723=ORIENTED_EDGE('',*,*,#14437,.F.);
#20724=ORIENTED_EDGE('',*,*,#14436,.F.);
#20725=ORIENTED_EDGE('',*,*,#14430,.F.);
#20726=ORIENTED_EDGE('',*,*,#14438,.F.);
#20727=ORIENTED_EDGE('',*,*,#14439,.T.);
#20728=ORIENTED_EDGE('',*,*,#14440,.F.);
#20729=ORIENTED_EDGE('',*,*,#14441,.F.);
#20730=ORIENTED_EDGE('',*,*,#14442,.F.);
#20731=ORIENTED_EDGE('',*,*,#14441,.T.);
#20732=ORIENTED_EDGE('',*,*,#14443,.T.);
#20733=ORIENTED_EDGE('',*,*,#14444,.F.);
#20734=ORIENTED_EDGE('',*,*,#14443,.F.);
#20735=ORIENTED_EDGE('',*,*,#14440,.T.);
#20736=ORIENTED_EDGE('',*,*,#14445,.T.);
#20737=ORIENTED_EDGE('',*,*,#14446,.F.);
#20738=ORIENTED_EDGE('',*,*,#14445,.F.);
#20739=ORIENTED_EDGE('',*,*,#14439,.F.);
#20740=ORIENTED_EDGE('',*,*,#14447,.F.);
#20741=ORIENTED_EDGE('',*,*,#14448,.T.);
#20742=ORIENTED_EDGE('',*,*,#14449,.F.);
#20743=ORIENTED_EDGE('',*,*,#14450,.F.);
#20744=ORIENTED_EDGE('',*,*,#14451,.F.);
#20745=ORIENTED_EDGE('',*,*,#14450,.T.);
#20746=ORIENTED_EDGE('',*,*,#14452,.T.);
#20747=ORIENTED_EDGE('',*,*,#14453,.F.);
#20748=ORIENTED_EDGE('',*,*,#14452,.F.);
#20749=ORIENTED_EDGE('',*,*,#14449,.T.);
#20750=ORIENTED_EDGE('',*,*,#14454,.T.);
#20751=ORIENTED_EDGE('',*,*,#14455,.F.);
#20752=ORIENTED_EDGE('',*,*,#14454,.F.);
#20753=ORIENTED_EDGE('',*,*,#14448,.F.);
#20754=ORIENTED_EDGE('',*,*,#14456,.F.);
#20755=ORIENTED_EDGE('',*,*,#14457,.T.);
#20756=ORIENTED_EDGE('',*,*,#14458,.F.);
#20757=ORIENTED_EDGE('',*,*,#14459,.F.);
#20758=ORIENTED_EDGE('',*,*,#14460,.F.);
#20759=ORIENTED_EDGE('',*,*,#14459,.T.);
#20760=ORIENTED_EDGE('',*,*,#14461,.T.);
#20761=ORIENTED_EDGE('',*,*,#14462,.F.);
#20762=ORIENTED_EDGE('',*,*,#14461,.F.);
#20763=ORIENTED_EDGE('',*,*,#14458,.T.);
#20764=ORIENTED_EDGE('',*,*,#14463,.T.);
#20765=ORIENTED_EDGE('',*,*,#14464,.F.);
#20766=ORIENTED_EDGE('',*,*,#14463,.F.);
#20767=ORIENTED_EDGE('',*,*,#14457,.F.);
#20768=ORIENTED_EDGE('',*,*,#14465,.F.);
#20769=ORIENTED_EDGE('',*,*,#13969,.F.);
#20770=ORIENTED_EDGE('',*,*,#14466,.T.);
#20771=ORIENTED_EDGE('',*,*,#14465,.T.);
#20772=ORIENTED_EDGE('',*,*,#14466,.F.);
#20773=ORIENTED_EDGE('',*,*,#14467,.F.);
#20774=ORIENTED_EDGE('',*,*,#14468,.T.);
#20775=ORIENTED_EDGE('',*,*,#14118,.T.);
#20776=ORIENTED_EDGE('',*,*,#14468,.F.);
#20777=ORIENTED_EDGE('',*,*,#14139,.T.);
#20778=ORIENTED_EDGE('',*,*,#14469,.F.);
#20779=ORIENTED_EDGE('',*,*,#14453,.T.);
#20780=ORIENTED_EDGE('',*,*,#14455,.T.);
#20781=ORIENTED_EDGE('',*,*,#14447,.T.);
#20782=ORIENTED_EDGE('',*,*,#14470,.F.);
#20783=ORIENTED_EDGE('',*,*,#14154,.T.);
#20784=ORIENTED_EDGE('',*,*,#14156,.T.);
#20785=ORIENTED_EDGE('',*,*,#14148,.T.);
#20786=ORIENTED_EDGE('',*,*,#14471,.F.);
#20787=ORIENTED_EDGE('',*,*,#14444,.T.);
#20788=ORIENTED_EDGE('',*,*,#14446,.T.);
#20789=ORIENTED_EDGE('',*,*,#14438,.T.);
#20790=ORIENTED_EDGE('',*,*,#14472,.F.);
#20791=ORIENTED_EDGE('',*,*,#14163,.T.);
#20792=ORIENTED_EDGE('',*,*,#14165,.T.);
#20793=ORIENTED_EDGE('',*,*,#14157,.T.);
#20794=ORIENTED_EDGE('',*,*,#14473,.F.);
#20795=ORIENTED_EDGE('',*,*,#14435,.T.);
#20796=ORIENTED_EDGE('',*,*,#14437,.T.);
#20797=ORIENTED_EDGE('',*,*,#14429,.T.);
#20798=ORIENTED_EDGE('',*,*,#14474,.F.);
#20799=ORIENTED_EDGE('',*,*,#14172,.T.);
#20800=ORIENTED_EDGE('',*,*,#14174,.T.);
#20801=ORIENTED_EDGE('',*,*,#14166,.T.);
#20802=ORIENTED_EDGE('',*,*,#14475,.F.);
#20803=ORIENTED_EDGE('',*,*,#14426,.T.);
#20804=ORIENTED_EDGE('',*,*,#14428,.T.);
#20805=ORIENTED_EDGE('',*,*,#14420,.T.);
#20806=ORIENTED_EDGE('',*,*,#14476,.F.);
#20807=ORIENTED_EDGE('',*,*,#14181,.T.);
#20808=ORIENTED_EDGE('',*,*,#14183,.T.);
#20809=ORIENTED_EDGE('',*,*,#14175,.T.);
#20810=ORIENTED_EDGE('',*,*,#14477,.F.);
#20811=ORIENTED_EDGE('',*,*,#14417,.T.);
#20812=ORIENTED_EDGE('',*,*,#14419,.T.);
#20813=ORIENTED_EDGE('',*,*,#14411,.T.);
#20814=ORIENTED_EDGE('',*,*,#14478,.F.);
#20815=ORIENTED_EDGE('',*,*,#14190,.T.);
#20816=ORIENTED_EDGE('',*,*,#14192,.T.);
#20817=ORIENTED_EDGE('',*,*,#14184,.T.);
#20818=ORIENTED_EDGE('',*,*,#14479,.F.);
#20819=ORIENTED_EDGE('',*,*,#14408,.T.);
#20820=ORIENTED_EDGE('',*,*,#14410,.T.);
#20821=ORIENTED_EDGE('',*,*,#14402,.T.);
#20822=ORIENTED_EDGE('',*,*,#14480,.F.);
#20823=ORIENTED_EDGE('',*,*,#14199,.T.);
#20824=ORIENTED_EDGE('',*,*,#14201,.T.);
#20825=ORIENTED_EDGE('',*,*,#14193,.T.);
#20826=ORIENTED_EDGE('',*,*,#14481,.F.);
#20827=ORIENTED_EDGE('',*,*,#14399,.T.);
#20828=ORIENTED_EDGE('',*,*,#14401,.T.);
#20829=ORIENTED_EDGE('',*,*,#14393,.T.);
#20830=ORIENTED_EDGE('',*,*,#14482,.F.);
#20831=ORIENTED_EDGE('',*,*,#14208,.T.);
#20832=ORIENTED_EDGE('',*,*,#14210,.T.);
#20833=ORIENTED_EDGE('',*,*,#14202,.T.);
#20834=ORIENTED_EDGE('',*,*,#14483,.F.);
#20835=ORIENTED_EDGE('',*,*,#14390,.T.);
#20836=ORIENTED_EDGE('',*,*,#14392,.T.);
#20837=ORIENTED_EDGE('',*,*,#14384,.T.);
#20838=ORIENTED_EDGE('',*,*,#14484,.F.);
#20839=ORIENTED_EDGE('',*,*,#14218,.T.);
#20840=ORIENTED_EDGE('',*,*,#14220,.T.);
#20841=ORIENTED_EDGE('',*,*,#14485,.T.);
#20842=ORIENTED_EDGE('',*,*,#14467,.T.);
#20843=ORIENTED_EDGE('',*,*,#14485,.F.);
#20844=ORIENTED_EDGE('',*,*,#14221,.T.);
#20845=ORIENTED_EDGE('',*,*,#14211,.T.);
#20846=ORIENTED_EDGE('',*,*,#14486,.F.);
#20847=ORIENTED_EDGE('',*,*,#14228,.T.);
#20848=ORIENTED_EDGE('',*,*,#14230,.T.);
#20849=ORIENTED_EDGE('',*,*,#14222,.T.);
#20850=ORIENTED_EDGE('',*,*,#14487,.F.);
#20851=ORIENTED_EDGE('',*,*,#14372,.T.);
#20852=ORIENTED_EDGE('',*,*,#14374,.T.);
#20853=ORIENTED_EDGE('',*,*,#14366,.T.);
#20854=ORIENTED_EDGE('',*,*,#14488,.F.);
#20855=ORIENTED_EDGE('',*,*,#14237,.T.);
#20856=ORIENTED_EDGE('',*,*,#14239,.T.);
#20857=ORIENTED_EDGE('',*,*,#14231,.T.);
#20858=ORIENTED_EDGE('',*,*,#14489,.F.);
#20859=ORIENTED_EDGE('',*,*,#14363,.T.);
#20860=ORIENTED_EDGE('',*,*,#14365,.T.);
#20861=ORIENTED_EDGE('',*,*,#14357,.T.);
#20862=ORIENTED_EDGE('',*,*,#14490,.F.);
#20863=ORIENTED_EDGE('',*,*,#14246,.T.);
#20864=ORIENTED_EDGE('',*,*,#14248,.T.);
#20865=ORIENTED_EDGE('',*,*,#14240,.T.);
#20866=ORIENTED_EDGE('',*,*,#14491,.F.);
#20867=ORIENTED_EDGE('',*,*,#14354,.T.);
#20868=ORIENTED_EDGE('',*,*,#14356,.T.);
#20869=ORIENTED_EDGE('',*,*,#14348,.T.);
#20870=ORIENTED_EDGE('',*,*,#14492,.F.);
#20871=ORIENTED_EDGE('',*,*,#14255,.T.);
#20872=ORIENTED_EDGE('',*,*,#14257,.T.);
#20873=ORIENTED_EDGE('',*,*,#14249,.T.);
#20874=ORIENTED_EDGE('',*,*,#14493,.F.);
#20875=ORIENTED_EDGE('',*,*,#14345,.T.);
#20876=ORIENTED_EDGE('',*,*,#14347,.T.);
#20877=ORIENTED_EDGE('',*,*,#14339,.T.);
#20878=ORIENTED_EDGE('',*,*,#14494,.F.);
#20879=ORIENTED_EDGE('',*,*,#14264,.T.);
#20880=ORIENTED_EDGE('',*,*,#14266,.T.);
#20881=ORIENTED_EDGE('',*,*,#14258,.T.);
#20882=ORIENTED_EDGE('',*,*,#14495,.F.);
#20883=ORIENTED_EDGE('',*,*,#14336,.T.);
#20884=ORIENTED_EDGE('',*,*,#14338,.T.);
#20885=ORIENTED_EDGE('',*,*,#14330,.T.);
#20886=ORIENTED_EDGE('',*,*,#14496,.F.);
#20887=ORIENTED_EDGE('',*,*,#14273,.T.);
#20888=ORIENTED_EDGE('',*,*,#14275,.T.);
#20889=ORIENTED_EDGE('',*,*,#14267,.T.);
#20890=ORIENTED_EDGE('',*,*,#14497,.F.);
#20891=ORIENTED_EDGE('',*,*,#14327,.T.);
#20892=ORIENTED_EDGE('',*,*,#14329,.T.);
#20893=ORIENTED_EDGE('',*,*,#14321,.T.);
#20894=ORIENTED_EDGE('',*,*,#14498,.F.);
#20895=ORIENTED_EDGE('',*,*,#14282,.T.);
#20896=ORIENTED_EDGE('',*,*,#14284,.T.);
#20897=ORIENTED_EDGE('',*,*,#14276,.T.);
#20898=ORIENTED_EDGE('',*,*,#14499,.F.);
#20899=ORIENTED_EDGE('',*,*,#14318,.T.);
#20900=ORIENTED_EDGE('',*,*,#14320,.T.);
#20901=ORIENTED_EDGE('',*,*,#14312,.T.);
#20902=ORIENTED_EDGE('',*,*,#14500,.F.);
#20903=ORIENTED_EDGE('',*,*,#14291,.T.);
#20904=ORIENTED_EDGE('',*,*,#14293,.T.);
#20905=ORIENTED_EDGE('',*,*,#14285,.T.);
#20906=ORIENTED_EDGE('',*,*,#14501,.F.);
#20907=ORIENTED_EDGE('',*,*,#14309,.T.);
#20908=ORIENTED_EDGE('',*,*,#14311,.T.);
#20909=ORIENTED_EDGE('',*,*,#14303,.T.);
#20910=ORIENTED_EDGE('',*,*,#14502,.F.);
#20911=ORIENTED_EDGE('',*,*,#14300,.T.);
#20912=ORIENTED_EDGE('',*,*,#14302,.T.);
#20913=ORIENTED_EDGE('',*,*,#14294,.T.);
#20914=ORIENTED_EDGE('',*,*,#14503,.F.);
#20915=ORIENTED_EDGE('',*,*,#14381,.T.);
#20916=ORIENTED_EDGE('',*,*,#14383,.T.);
#20917=ORIENTED_EDGE('',*,*,#14378,.T.);
#20918=ORIENTED_EDGE('',*,*,#14504,.F.);
#20919=ORIENTED_EDGE('',*,*,#14462,.T.);
#20920=ORIENTED_EDGE('',*,*,#14464,.T.);
#20921=ORIENTED_EDGE('',*,*,#14456,.T.);
#20922=ORIENTED_EDGE('',*,*,#14505,.F.);
#20923=ORIENTED_EDGE('',*,*,#14145,.T.);
#20924=ORIENTED_EDGE('',*,*,#14147,.T.);
#20925=ORIENTED_EDGE('',*,*,#14506,.F.);
#20926=ORIENTED_EDGE('',*,*,#14507,.T.);
#20927=ORIENTED_EDGE('',*,*,#14217,.T.);
#20928=ORIENTED_EDGE('',*,*,#14484,.T.);
#20929=ORIENTED_EDGE('',*,*,#14388,.T.);
#20930=ORIENTED_EDGE('',*,*,#14483,.T.);
#20931=ORIENTED_EDGE('',*,*,#14206,.T.);
#20932=ORIENTED_EDGE('',*,*,#14482,.T.);
#20933=ORIENTED_EDGE('',*,*,#14397,.T.);
#20934=ORIENTED_EDGE('',*,*,#14481,.T.);
#20935=ORIENTED_EDGE('',*,*,#14197,.T.);
#20936=ORIENTED_EDGE('',*,*,#14480,.T.);
#20937=ORIENTED_EDGE('',*,*,#14406,.T.);
#20938=ORIENTED_EDGE('',*,*,#14479,.T.);
#20939=ORIENTED_EDGE('',*,*,#14188,.T.);
#20940=ORIENTED_EDGE('',*,*,#14478,.T.);
#20941=ORIENTED_EDGE('',*,*,#14415,.T.);
#20942=ORIENTED_EDGE('',*,*,#14477,.T.);
#20943=ORIENTED_EDGE('',*,*,#14179,.T.);
#20944=ORIENTED_EDGE('',*,*,#14476,.T.);
#20945=ORIENTED_EDGE('',*,*,#14424,.T.);
#20946=ORIENTED_EDGE('',*,*,#14475,.T.);
#20947=ORIENTED_EDGE('',*,*,#14170,.T.);
#20948=ORIENTED_EDGE('',*,*,#14474,.T.);
#20949=ORIENTED_EDGE('',*,*,#14433,.T.);
#20950=ORIENTED_EDGE('',*,*,#14473,.T.);
#20951=ORIENTED_EDGE('',*,*,#14161,.T.);
#20952=ORIENTED_EDGE('',*,*,#14472,.T.);
#20953=ORIENTED_EDGE('',*,*,#14442,.T.);
#20954=ORIENTED_EDGE('',*,*,#14471,.T.);
#20955=ORIENTED_EDGE('',*,*,#14152,.T.);
#20956=ORIENTED_EDGE('',*,*,#14470,.T.);
#20957=ORIENTED_EDGE('',*,*,#14451,.T.);
#20958=ORIENTED_EDGE('',*,*,#14469,.T.);
#20959=ORIENTED_EDGE('',*,*,#14143,.T.);
#20960=ORIENTED_EDGE('',*,*,#14505,.T.);
#20961=ORIENTED_EDGE('',*,*,#14460,.T.);
#20962=ORIENTED_EDGE('',*,*,#14504,.T.);
#20963=ORIENTED_EDGE('',*,*,#14375,.T.);
#20964=ORIENTED_EDGE('',*,*,#14503,.T.);
#20965=ORIENTED_EDGE('',*,*,#14298,.T.);
#20966=ORIENTED_EDGE('',*,*,#14502,.T.);
#20967=ORIENTED_EDGE('',*,*,#14307,.T.);
#20968=ORIENTED_EDGE('',*,*,#14501,.T.);
#20969=ORIENTED_EDGE('',*,*,#14289,.T.);
#20970=ORIENTED_EDGE('',*,*,#14500,.T.);
#20971=ORIENTED_EDGE('',*,*,#14316,.T.);
#20972=ORIENTED_EDGE('',*,*,#14499,.T.);
#20973=ORIENTED_EDGE('',*,*,#14280,.T.);
#20974=ORIENTED_EDGE('',*,*,#14498,.T.);
#20975=ORIENTED_EDGE('',*,*,#14325,.T.);
#20976=ORIENTED_EDGE('',*,*,#14497,.T.);
#20977=ORIENTED_EDGE('',*,*,#14271,.T.);
#20978=ORIENTED_EDGE('',*,*,#14496,.T.);
#20979=ORIENTED_EDGE('',*,*,#14334,.T.);
#20980=ORIENTED_EDGE('',*,*,#14495,.T.);
#20981=ORIENTED_EDGE('',*,*,#14262,.T.);
#20982=ORIENTED_EDGE('',*,*,#14494,.T.);
#20983=ORIENTED_EDGE('',*,*,#14343,.T.);
#20984=ORIENTED_EDGE('',*,*,#14493,.T.);
#20985=ORIENTED_EDGE('',*,*,#14253,.T.);
#20986=ORIENTED_EDGE('',*,*,#14492,.T.);
#20987=ORIENTED_EDGE('',*,*,#14352,.T.);
#20988=ORIENTED_EDGE('',*,*,#14491,.T.);
#20989=ORIENTED_EDGE('',*,*,#14244,.T.);
#20990=ORIENTED_EDGE('',*,*,#14490,.T.);
#20991=ORIENTED_EDGE('',*,*,#14361,.T.);
#20992=ORIENTED_EDGE('',*,*,#14489,.T.);
#20993=ORIENTED_EDGE('',*,*,#14235,.T.);
#20994=ORIENTED_EDGE('',*,*,#14488,.T.);
#20995=ORIENTED_EDGE('',*,*,#14370,.T.);
#20996=ORIENTED_EDGE('',*,*,#14487,.T.);
#20997=ORIENTED_EDGE('',*,*,#14226,.T.);
#20998=ORIENTED_EDGE('',*,*,#14486,.T.);
#20999=ORIENTED_EDGE('',*,*,#14215,.T.);
#21000=ORIENTED_EDGE('',*,*,#14507,.F.);
#21001=ORIENTED_EDGE('',*,*,#14506,.T.);
#21002=ORIENTED_EDGE('',*,*,#14121,.T.);
#21003=ORIENTED_EDGE('',*,*,#14137,.T.);
#21004=ORIENTED_EDGE('',*,*,#14134,.T.);
#21005=ORIENTED_EDGE('',*,*,#14131,.T.);
#21006=ORIENTED_EDGE('',*,*,#14128,.T.);
#21007=ORIENTED_EDGE('',*,*,#14125,.T.);
#21008=ORIENTED_EDGE('',*,*,#14508,.F.);
#21009=ORIENTED_EDGE('',*,*,#14509,.T.);
#21010=ORIENTED_EDGE('',*,*,#14510,.F.);
#21011=ORIENTED_EDGE('',*,*,#14511,.F.);
#21012=ORIENTED_EDGE('',*,*,#14512,.F.);
#21013=ORIENTED_EDGE('',*,*,#14513,.T.);
#21014=ORIENTED_EDGE('',*,*,#14508,.T.);
#21015=ORIENTED_EDGE('',*,*,#14514,.F.);
#21016=ORIENTED_EDGE('',*,*,#14515,.F.);
#21017=ORIENTED_EDGE('',*,*,#14516,.T.);
#21018=ORIENTED_EDGE('',*,*,#14512,.T.);
#21019=ORIENTED_EDGE('',*,*,#14517,.F.);
#21020=ORIENTED_EDGE('',*,*,#14518,.F.);
#21021=ORIENTED_EDGE('',*,*,#14519,.T.);
#21022=ORIENTED_EDGE('',*,*,#14515,.T.);
#21023=ORIENTED_EDGE('',*,*,#14520,.F.);
#21024=ORIENTED_EDGE('',*,*,#14521,.F.);
#21025=ORIENTED_EDGE('',*,*,#14522,.T.);
#21026=ORIENTED_EDGE('',*,*,#14518,.T.);
#21027=ORIENTED_EDGE('',*,*,#14523,.F.);
#21028=ORIENTED_EDGE('',*,*,#14524,.F.);
#21029=ORIENTED_EDGE('',*,*,#14525,.T.);
#21030=ORIENTED_EDGE('',*,*,#14521,.T.);
#21031=ORIENTED_EDGE('',*,*,#14526,.F.);
#21032=ORIENTED_EDGE('',*,*,#14527,.F.);
#21033=ORIENTED_EDGE('',*,*,#14528,.T.);
#21034=ORIENTED_EDGE('',*,*,#14524,.T.);
#21035=ORIENTED_EDGE('',*,*,#14529,.F.);
#21036=ORIENTED_EDGE('',*,*,#14530,.F.);
#21037=ORIENTED_EDGE('',*,*,#14531,.F.);
#21038=ORIENTED_EDGE('',*,*,#14532,.T.);
#21039=ORIENTED_EDGE('',*,*,#14527,.T.);
#21040=ORIENTED_EDGE('',*,*,#14533,.F.);
#21041=ORIENTED_EDGE('',*,*,#14534,.F.);
#21042=ORIENTED_EDGE('',*,*,#14535,.T.);
#21043=ORIENTED_EDGE('',*,*,#14536,.T.);
#21044=ORIENTED_EDGE('',*,*,#14537,.T.);
#21045=ORIENTED_EDGE('',*,*,#14538,.F.);
#21046=ORIENTED_EDGE('',*,*,#14539,.T.);
#21047=ORIENTED_EDGE('',*,*,#14534,.T.);
#21048=ORIENTED_EDGE('',*,*,#14540,.T.);
#21049=ORIENTED_EDGE('',*,*,#14541,.F.);
#21050=ORIENTED_EDGE('',*,*,#14542,.T.);
#21051=ORIENTED_EDGE('',*,*,#14538,.T.);
#21052=ORIENTED_EDGE('',*,*,#14543,.T.);
#21053=ORIENTED_EDGE('',*,*,#14544,.F.);
#21054=ORIENTED_EDGE('',*,*,#14545,.T.);
#21055=ORIENTED_EDGE('',*,*,#14541,.T.);
#21056=ORIENTED_EDGE('',*,*,#14546,.T.);
#21057=ORIENTED_EDGE('',*,*,#14547,.F.);
#21058=ORIENTED_EDGE('',*,*,#14548,.T.);
#21059=ORIENTED_EDGE('',*,*,#14544,.T.);
#21060=ORIENTED_EDGE('',*,*,#14549,.T.);
#21061=ORIENTED_EDGE('',*,*,#14550,.F.);
#21062=ORIENTED_EDGE('',*,*,#14551,.T.);
#21063=ORIENTED_EDGE('',*,*,#14547,.T.);
#21064=ORIENTED_EDGE('',*,*,#14552,.T.);
#21065=ORIENTED_EDGE('',*,*,#14553,.F.);
#21066=ORIENTED_EDGE('',*,*,#14554,.T.);
#21067=ORIENTED_EDGE('',*,*,#14550,.T.);
#21068=ORIENTED_EDGE('',*,*,#14555,.T.);
#21069=ORIENTED_EDGE('',*,*,#14556,.F.);
#21070=ORIENTED_EDGE('',*,*,#14557,.T.);
#21071=ORIENTED_EDGE('',*,*,#14553,.T.);
#21072=ORIENTED_EDGE('',*,*,#14558,.T.);
#21073=ORIENTED_EDGE('',*,*,#14559,.F.);
#21074=ORIENTED_EDGE('',*,*,#14560,.T.);
#21075=ORIENTED_EDGE('',*,*,#14556,.T.);
#21076=ORIENTED_EDGE('',*,*,#14561,.T.);
#21077=ORIENTED_EDGE('',*,*,#14562,.F.);
#21078=ORIENTED_EDGE('',*,*,#14563,.T.);
#21079=ORIENTED_EDGE('',*,*,#14564,.F.);
#21080=ORIENTED_EDGE('',*,*,#14565,.F.);
#21081=ORIENTED_EDGE('',*,*,#14566,.F.);
#21082=ORIENTED_EDGE('',*,*,#14567,.T.);
#21083=ORIENTED_EDGE('',*,*,#14562,.T.);
#21084=ORIENTED_EDGE('',*,*,#14568,.F.);
#21085=ORIENTED_EDGE('',*,*,#14569,.F.);
#21086=ORIENTED_EDGE('',*,*,#14570,.T.);
#21087=ORIENTED_EDGE('',*,*,#14566,.T.);
#21088=ORIENTED_EDGE('',*,*,#14571,.F.);
#21089=ORIENTED_EDGE('',*,*,#14572,.F.);
#21090=ORIENTED_EDGE('',*,*,#14573,.T.);
#21091=ORIENTED_EDGE('',*,*,#14569,.T.);
#21092=ORIENTED_EDGE('',*,*,#14574,.F.);
#21093=ORIENTED_EDGE('',*,*,#14575,.F.);
#21094=ORIENTED_EDGE('',*,*,#14576,.T.);
#21095=ORIENTED_EDGE('',*,*,#14572,.T.);
#21096=ORIENTED_EDGE('',*,*,#14577,.F.);
#21097=ORIENTED_EDGE('',*,*,#14578,.F.);
#21098=ORIENTED_EDGE('',*,*,#14579,.T.);
#21099=ORIENTED_EDGE('',*,*,#14575,.T.);
#21100=ORIENTED_EDGE('',*,*,#14580,.F.);
#21101=ORIENTED_EDGE('',*,*,#14581,.F.);
#21102=ORIENTED_EDGE('',*,*,#14582,.T.);
#21103=ORIENTED_EDGE('',*,*,#14578,.T.);
#21104=ORIENTED_EDGE('',*,*,#14583,.F.);
#21105=ORIENTED_EDGE('',*,*,#14584,.F.);
#21106=ORIENTED_EDGE('',*,*,#14585,.T.);
#21107=ORIENTED_EDGE('',*,*,#14581,.T.);
#21108=ORIENTED_EDGE('',*,*,#14586,.F.);
#21109=ORIENTED_EDGE('',*,*,#14587,.F.);
#21110=ORIENTED_EDGE('',*,*,#14588,.T.);
#21111=ORIENTED_EDGE('',*,*,#14584,.T.);
#21112=ORIENTED_EDGE('',*,*,#14589,.F.);
#21113=ORIENTED_EDGE('',*,*,#14564,.T.);
#21114=ORIENTED_EDGE('',*,*,#14590,.T.);
#21115=ORIENTED_EDGE('',*,*,#14591,.F.);
#21116=ORIENTED_EDGE('',*,*,#14592,.F.);
#21117=ORIENTED_EDGE('',*,*,#14593,.T.);
#21118=ORIENTED_EDGE('',*,*,#14593,.F.);
#21119=ORIENTED_EDGE('',*,*,#14594,.F.);
#21120=ORIENTED_EDGE('',*,*,#14561,.F.);
#21121=ORIENTED_EDGE('',*,*,#14558,.F.);
#21122=ORIENTED_EDGE('',*,*,#14555,.F.);
#21123=ORIENTED_EDGE('',*,*,#14552,.F.);
#21124=ORIENTED_EDGE('',*,*,#14549,.F.);
#21125=ORIENTED_EDGE('',*,*,#14546,.F.);
#21126=ORIENTED_EDGE('',*,*,#14543,.F.);
#21127=ORIENTED_EDGE('',*,*,#14540,.F.);
#21128=ORIENTED_EDGE('',*,*,#14537,.F.);
#21129=ORIENTED_EDGE('',*,*,#14595,.F.);
#21130=ORIENTED_EDGE('',*,*,#14596,.T.);
#21131=ORIENTED_EDGE('',*,*,#14589,.T.);
#21132=ORIENTED_EDGE('',*,*,#14586,.T.);
#21133=ORIENTED_EDGE('',*,*,#14583,.T.);
#21134=ORIENTED_EDGE('',*,*,#14580,.T.);
#21135=ORIENTED_EDGE('',*,*,#14577,.T.);
#21136=ORIENTED_EDGE('',*,*,#14574,.T.);
#21137=ORIENTED_EDGE('',*,*,#14571,.T.);
#21138=ORIENTED_EDGE('',*,*,#14568,.T.);
#21139=ORIENTED_EDGE('',*,*,#14565,.T.);
#21140=ORIENTED_EDGE('',*,*,#14587,.T.);
#21141=ORIENTED_EDGE('',*,*,#14596,.F.);
#21142=ORIENTED_EDGE('',*,*,#14597,.F.);
#21143=ORIENTED_EDGE('',*,*,#14598,.T.);
#21144=ORIENTED_EDGE('',*,*,#14590,.F.);
#21145=ORIENTED_EDGE('',*,*,#14563,.F.);
#21146=ORIENTED_EDGE('',*,*,#14567,.F.);
#21147=ORIENTED_EDGE('',*,*,#14570,.F.);
#21148=ORIENTED_EDGE('',*,*,#14573,.F.);
#21149=ORIENTED_EDGE('',*,*,#14576,.F.);
#21150=ORIENTED_EDGE('',*,*,#14579,.F.);
#21151=ORIENTED_EDGE('',*,*,#14582,.F.);
#21152=ORIENTED_EDGE('',*,*,#14585,.F.);
#21153=ORIENTED_EDGE('',*,*,#14588,.F.);
#21154=ORIENTED_EDGE('',*,*,#14598,.F.);
#21155=ORIENTED_EDGE('',*,*,#14599,.F.);
#21156=ORIENTED_EDGE('',*,*,#14535,.F.);
#21157=ORIENTED_EDGE('',*,*,#14539,.F.);
#21158=ORIENTED_EDGE('',*,*,#14542,.F.);
#21159=ORIENTED_EDGE('',*,*,#14545,.F.);
#21160=ORIENTED_EDGE('',*,*,#14548,.F.);
#21161=ORIENTED_EDGE('',*,*,#14551,.F.);
#21162=ORIENTED_EDGE('',*,*,#14554,.F.);
#21163=ORIENTED_EDGE('',*,*,#14557,.F.);
#21164=ORIENTED_EDGE('',*,*,#14560,.F.);
#21165=ORIENTED_EDGE('',*,*,#14600,.F.);
#21166=ORIENTED_EDGE('',*,*,#14559,.T.);
#21167=ORIENTED_EDGE('',*,*,#14594,.T.);
#21168=ORIENTED_EDGE('',*,*,#14601,.F.);
#21169=ORIENTED_EDGE('',*,*,#14600,.T.);
#21170=ORIENTED_EDGE('',*,*,#14602,.F.);
#21171=ORIENTED_EDGE('',*,*,#14603,.F.);
#21172=ORIENTED_EDGE('',*,*,#14604,.F.);
#21173=ORIENTED_EDGE('',*,*,#14605,.T.);
#21174=ORIENTED_EDGE('',*,*,#14606,.F.);
#21175=ORIENTED_EDGE('',*,*,#14605,.F.);
#21176=ORIENTED_EDGE('',*,*,#14607,.F.);
#21177=ORIENTED_EDGE('',*,*,#14608,.T.);
#21178=ORIENTED_EDGE('',*,*,#14609,.F.);
#21179=ORIENTED_EDGE('',*,*,#14608,.F.);
#21180=ORIENTED_EDGE('',*,*,#14610,.F.);
#21181=ORIENTED_EDGE('',*,*,#14611,.T.);
#21182=ORIENTED_EDGE('',*,*,#14533,.T.);
#21183=ORIENTED_EDGE('',*,*,#14529,.T.);
#21184=ORIENTED_EDGE('',*,*,#14526,.T.);
#21185=ORIENTED_EDGE('',*,*,#14523,.T.);
#21186=ORIENTED_EDGE('',*,*,#14520,.T.);
#21187=ORIENTED_EDGE('',*,*,#14517,.T.);
#21188=ORIENTED_EDGE('',*,*,#14514,.T.);
#21189=ORIENTED_EDGE('',*,*,#14511,.T.);
#21190=ORIENTED_EDGE('',*,*,#14612,.T.);
#21191=ORIENTED_EDGE('',*,*,#14613,.T.);
#21192=ORIENTED_EDGE('',*,*,#14614,.T.);
#21193=ORIENTED_EDGE('',*,*,#14615,.T.);
#21194=ORIENTED_EDGE('',*,*,#14616,.T.);
#21195=ORIENTED_EDGE('',*,*,#14531,.T.);
#21196=ORIENTED_EDGE('',*,*,#14617,.T.);
#21197=ORIENTED_EDGE('',*,*,#14610,.T.);
#21198=ORIENTED_EDGE('',*,*,#14607,.T.);
#21199=ORIENTED_EDGE('',*,*,#14604,.T.);
#21200=ORIENTED_EDGE('',*,*,#14530,.T.);
#21201=ORIENTED_EDGE('',*,*,#14611,.F.);
#21202=ORIENTED_EDGE('',*,*,#14617,.F.);
#21203=ORIENTED_EDGE('',*,*,#14618,.F.);
#21204=ORIENTED_EDGE('',*,*,#14509,.F.);
#21205=ORIENTED_EDGE('',*,*,#14513,.F.);
#21206=ORIENTED_EDGE('',*,*,#14516,.F.);
#21207=ORIENTED_EDGE('',*,*,#14519,.F.);
#21208=ORIENTED_EDGE('',*,*,#14522,.F.);
#21209=ORIENTED_EDGE('',*,*,#14525,.F.);
#21210=ORIENTED_EDGE('',*,*,#14528,.F.);
#21211=ORIENTED_EDGE('',*,*,#14532,.F.);
#21212=ORIENTED_EDGE('',*,*,#14616,.F.);
#21213=ORIENTED_EDGE('',*,*,#14619,.T.);
#21214=ORIENTED_EDGE('',*,*,#14620,.F.);
#21215=ORIENTED_EDGE('',*,*,#14619,.F.);
#21216=ORIENTED_EDGE('',*,*,#14615,.F.);
#21217=ORIENTED_EDGE('',*,*,#14621,.T.);
#21218=ORIENTED_EDGE('',*,*,#14622,.F.);
#21219=ORIENTED_EDGE('',*,*,#14621,.F.);
#21220=ORIENTED_EDGE('',*,*,#14614,.F.);
#21221=ORIENTED_EDGE('',*,*,#14603,.T.);
#21222=ORIENTED_EDGE('',*,*,#14623,.F.);
#21223=ORIENTED_EDGE('',*,*,#14624,.T.);
#21224=ORIENTED_EDGE('',*,*,#14625,.F.);
#21225=ORIENTED_EDGE('',*,*,#14626,.F.);
#21226=ORIENTED_EDGE('',*,*,#14627,.F.);
#21227=ORIENTED_EDGE('',*,*,#14628,.F.);
#21228=ORIENTED_EDGE('',*,*,#14629,.F.);
#21229=ORIENTED_EDGE('',*,*,#14630,.F.);
#21230=ORIENTED_EDGE('',*,*,#14631,.F.);
#21231=ORIENTED_EDGE('',*,*,#14624,.F.);
#21232=ORIENTED_EDGE('',*,*,#14629,.T.);
#21233=ORIENTED_EDGE('',*,*,#14632,.T.);
#21234=ORIENTED_EDGE('',*,*,#14633,.T.);
#21235=ORIENTED_EDGE('',*,*,#14634,.F.);
#21236=ORIENTED_EDGE('',*,*,#14628,.T.);
#21237=ORIENTED_EDGE('',*,*,#14635,.T.);
#21238=ORIENTED_EDGE('',*,*,#14636,.T.);
#21239=ORIENTED_EDGE('',*,*,#14632,.F.);
#21240=ORIENTED_EDGE('',*,*,#14627,.T.);
#21241=ORIENTED_EDGE('',*,*,#14637,.T.);
#21242=ORIENTED_EDGE('',*,*,#14638,.T.);
#21243=ORIENTED_EDGE('',*,*,#14635,.F.);
#21244=ORIENTED_EDGE('',*,*,#14633,.F.);
#21245=ORIENTED_EDGE('',*,*,#14636,.F.);
#21246=ORIENTED_EDGE('',*,*,#14638,.F.);
#21247=ORIENTED_EDGE('',*,*,#14639,.F.);
#21248=ORIENTED_EDGE('',*,*,#14640,.F.);
#21249=ORIENTED_EDGE('',*,*,#14641,.T.);
#21250=ORIENTED_EDGE('',*,*,#14642,.F.);
#21251=ORIENTED_EDGE('',*,*,#14641,.F.);
#21252=ORIENTED_EDGE('',*,*,#14643,.F.);
#21253=ORIENTED_EDGE('',*,*,#14644,.F.);
#21254=ORIENTED_EDGE('',*,*,#14626,.T.);
#21255=ORIENTED_EDGE('',*,*,#14645,.T.);
#21256=ORIENTED_EDGE('',*,*,#14639,.T.);
#21257=ORIENTED_EDGE('',*,*,#14637,.F.);
#21258=ORIENTED_EDGE('',*,*,#14642,.T.);
#21259=ORIENTED_EDGE('',*,*,#14599,.T.);
#21260=ORIENTED_EDGE('',*,*,#14597,.T.);
#21261=ORIENTED_EDGE('',*,*,#14595,.T.);
#21262=ORIENTED_EDGE('',*,*,#14536,.F.);
#21263=ORIENTED_EDGE('',*,*,#14646,.F.);
#21264=ORIENTED_EDGE('',*,*,#14623,.T.);
#21265=ORIENTED_EDGE('',*,*,#14647,.F.);
#21266=ORIENTED_EDGE('',*,*,#14648,.F.);
#21267=ORIENTED_EDGE('',*,*,#14630,.T.);
#21268=ORIENTED_EDGE('',*,*,#14634,.T.);
#21269=ORIENTED_EDGE('',*,*,#14644,.T.);
#21270=ORIENTED_EDGE('',*,*,#14649,.F.);
#21271=ORIENTED_EDGE('',*,*,#14625,.T.);
#21272=ORIENTED_EDGE('',*,*,#14631,.T.);
#21273=ORIENTED_EDGE('',*,*,#14649,.T.);
#21274=ORIENTED_EDGE('',*,*,#14643,.T.);
#21275=ORIENTED_EDGE('',*,*,#14640,.T.);
#21276=ORIENTED_EDGE('',*,*,#14645,.F.);
#21277=ORIENTED_EDGE('',*,*,#14648,.T.);
#21278=ORIENTED_EDGE('',*,*,#14650,.T.);
#21279=ORIENTED_EDGE('',*,*,#14651,.F.);
#21280=ORIENTED_EDGE('',*,*,#14650,.F.);
#21281=ORIENTED_EDGE('',*,*,#14652,.T.);
#21282=ORIENTED_EDGE('',*,*,#14653,.T.);
#21283=ORIENTED_EDGE('',*,*,#14646,.T.);
#21284=ORIENTED_EDGE('',*,*,#14653,.F.);
#21285=ORIENTED_EDGE('',*,*,#14654,.F.);
#21286=ORIENTED_EDGE('',*,*,#14651,.T.);
#21287=ORIENTED_EDGE('',*,*,#14612,.F.);
#21288=ORIENTED_EDGE('',*,*,#14613,.F.);
#21289=ORIENTED_EDGE('',*,*,#14655,.T.);
#21290=ORIENTED_EDGE('',*,*,#14654,.T.);
#21291=ORIENTED_EDGE('',*,*,#14655,.F.);
#21292=ORIENTED_EDGE('',*,*,#14602,.T.);
#21293=ORIENTED_EDGE('',*,*,#14606,.T.);
#21294=ORIENTED_EDGE('',*,*,#14609,.T.);
#21295=ORIENTED_EDGE('',*,*,#14510,.T.);
#21296=ORIENTED_EDGE('',*,*,#14618,.T.);
#21297=ORIENTED_EDGE('',*,*,#14620,.T.);
#21298=ORIENTED_EDGE('',*,*,#14622,.T.);
#21299=ORIENTED_EDGE('',*,*,#14656,.F.);
#21300=ORIENTED_EDGE('',*,*,#14647,.T.);
#21301=ORIENTED_EDGE('',*,*,#14657,.T.);
#21302=ORIENTED_EDGE('',*,*,#14656,.T.);
#21303=ORIENTED_EDGE('',*,*,#14657,.F.);
#21304=ORIENTED_EDGE('',*,*,#14658,.F.);
#21305=ORIENTED_EDGE('',*,*,#14659,.T.);
#21306=ORIENTED_EDGE('',*,*,#14591,.T.);
#21307=ORIENTED_EDGE('',*,*,#14601,.T.);
#21308=ORIENTED_EDGE('',*,*,#14592,.T.);
#21309=ORIENTED_EDGE('',*,*,#14659,.F.);
#21310=ORIENTED_EDGE('',*,*,#14658,.T.);
#21311=ORIENTED_EDGE('',*,*,#14660,.F.);
#21312=ORIENTED_EDGE('',*,*,#14660,.T.);
#21313=ORIENTED_EDGE('',*,*,#14661,.T.);
#21314=ORIENTED_EDGE('',*,*,#14652,.F.);
#21315=ORIENTED_EDGE('',*,*,#14661,.F.);
#21316=CONICAL_SURFACE('',#23047,0.635,0.785398163397444);
#21317=CONICAL_SURFACE('',#23063,0.635,0.785398163397445);
#21318=CONICAL_SURFACE('',#23076,0.635,0.785398163397448);
#21319=CONICAL_SURFACE('',#23080,0.635,0.785398163397448);
#21320=CONICAL_SURFACE('',#23081,0.635,0.785398163397448);
#21321=CONICAL_SURFACE('',#23085,0.635,0.785398163397448);
#21322=CONICAL_SURFACE('',#23086,0.635,0.785398163397444);
#21323=CONICAL_SURFACE('',#23090,0.635,0.785398163397445);
#21324=CONICAL_SURFACE('',#23091,0.635,0.785398163397444);
#21325=CONICAL_SURFACE('',#23095,0.635,0.785398163397445);
#21326=CONICAL_SURFACE('',#23096,0.635,0.785398163397448);
#21327=CONICAL_SURFACE('',#23100,0.635,0.785398163397448);
#21328=CONICAL_SURFACE('',#23101,0.635,0.785398163397448);
#21329=CONICAL_SURFACE('',#23105,0.635,0.785398163397448);
#21330=CONICAL_SURFACE('',#23106,0.635,0.785398163397448);
#21331=CONICAL_SURFACE('',#23110,0.635,0.785398163397448);
#21332=CONICAL_SURFACE('',#23111,0.635,0.785398163397448);
#21333=CONICAL_SURFACE('',#23115,0.635,0.785398163397448);
#21334=CONICAL_SURFACE('',#23118,3.425,0.785398163397451);
#21335=CONICAL_SURFACE('',#23122,3.425,0.785398163397451);
#21336=CONICAL_SURFACE('',#23129,1.63,0.785398163397446);
#21337=CONICAL_SURFACE('',#23135,1.275,0.785398163397448);
#21338=CONICAL_SURFACE('',#23139,1.275,0.785398163397437);
#21339=CONICAL_SURFACE('',#23152,3.96,0.785398163397457);
#21340=CONICAL_SURFACE('',#23154,1.825,0.785398163397442);
#21341=CONICAL_SURFACE('',#23163,3.97,0.785398163397445);
#21342=CONICAL_SURFACE('',#23176,0.385,0.785398163397448);
#21343=CONICAL_SURFACE('',#23180,0.385,0.785398163397448);
#21344=CONICAL_SURFACE('',#23201,1.98,0.785398163397448);
#21345=CONICAL_SURFACE('',#23209,1.98,0.785398163397448);
#21346=CONICAL_SURFACE('',#23217,1.475,1.13416916698136);
#21347=CONICAL_SURFACE('',#23221,1.4,1.24904577239825);
#21348=CONICAL_SURFACE('',#23225,1.4,1.13416916698136);
#21349=CONICAL_SURFACE('',#23433,1.18258529610859,1.0471975511966);
#21350=CONICAL_SURFACE('',#23438,1.18258529610859,1.0471975511966);
#21351=CONICAL_SURFACE('',#23450,0.3,0.982793723247329);
#21352=CONICAL_SURFACE('',#23453,0.7931,0.785398163397448);
#21353=CONICAL_SURFACE('',#23488,0.87,0.785398163397447);
#21354=CONICAL_SURFACE('',#23527,1.02473275573014,1.0471975511966);
#21355=CONICAL_SURFACE('',#23532,1.02473275573014,1.0471975511966);
#21356=CONICAL_SURFACE('',#23550,0.61785,0.785398163397448);
#21357=CONICAL_SURFACE('',#23554,0.67,0.785398163397446);
#21358=CONICAL_SURFACE('',#23558,0.39,0.20943951023932);
#21359=CONICAL_SURFACE('',#23560,0.1875,0.536910742740044);
#21360=CONICAL_SURFACE('',#23563,0.125,1.03037682652432);
#21361=CONICAL_SURFACE('',#23580,1.05,0.785398163397442);
#21362=CONICAL_SURFACE('',#23586,1.225,0.785398163397442);
#21363=CONICAL_SURFACE('',#23606,1.2,0.785398163397446);
#21364=CONICAL_SURFACE('',#23711,1.73,0.785398163397447);
#21365=CONICAL_SURFACE('',#23712,3.45,0.785398163397448);
#21366=CONICAL_SURFACE('',#23715,3.66,0.785398163397449);
#21367=CONICAL_SURFACE('',#23733,0.4625,0.785398163397455);
#21368=CONICAL_SURFACE('',#23741,0.4625,0.785398163397446);
#21369=CONICAL_SURFACE('',#23749,0.4625,0.785398163397446);
#21370=CONICAL_SURFACE('',#23757,0.4625,0.785398163397455);
#21371=CONICAL_SURFACE('',#23765,0.4625,0.785398163397446);
#21372=CONICAL_SURFACE('',#23773,0.4625,0.785398163397446);
#21373=CONICAL_SURFACE('',#23809,0.70285,0.785398163397448);
#21374=CONICAL_SURFACE('',#23815,1.25,0.785398163397448);
#21375=CONICAL_SURFACE('',#23818,4.325,0.785398163397448);
#21376=CONICAL_SURFACE('',#23826,2.05,0.785398163397451);
#21377=CONICAL_SURFACE('',#23839,4.1,0.963808662748489);
#21378=CONICAL_SURFACE('',#23841,3.15,0.785398163397451);
#21379=CONICAL_SURFACE('',#23844,6.95,0.785398163397447);
#21380=CONICAL_SURFACE('',#23848,6.975,0.463647609000805);
#21381=CONICAL_SURFACE('',#23867,0.465,0.785398163397456);
#21382=CONICAL_SURFACE('',#23882,0.465,0.785398163397452);
#21383=CONICAL_SURFACE('',#23901,0.465,0.785398163397448);
#21384=CONICAL_SURFACE('',#23905,0.465,0.785398163397444);
#21385=CONICAL_SURFACE('',#23906,0.465,0.785398163397448);
#21386=CONICAL_SURFACE('',#23910,0.465,0.785398163397444);
#21387=CONICAL_SURFACE('',#23911,0.465,0.785398163397456);
#21388=CONICAL_SURFACE('',#23915,0.465,0.785398163397452);
#21389=CONICAL_SURFACE('',#23916,0.465,0.785398163397448);
#21390=CONICAL_SURFACE('',#23920,0.465,0.785398163397444);
#21391=CONICAL_SURFACE('',#23921,0.465,0.785398163397448);
#21392=CONICAL_SURFACE('',#23925,0.465,0.785398163397444);
#21393=CONICAL_SURFACE('',#23927,0.8781,0.785398163397448);
#21394=CONICAL_SURFACE('',#23933,0.8781,0.785398163397448);
#21395=CONICAL_SURFACE('',#23946,0.6,1.02974425867665);
#21396=CONICAL_SURFACE('',#23953,6.95,0.785398163397447);
#21397=CONICAL_SURFACE('',#23957,6.95,0.785398163397446);
#21398=CONICAL_SURFACE('',#23964,0.3,1.02974425867665);
#21399=CONICAL_SURFACE('',#23984,1.525,0.785398163397448);
#21400=CONICAL_SURFACE('',#23990,1.525,0.785398163397451);
#21401=CONICAL_SURFACE('',#23991,6.95,0.785398163397447);
#21402=CONICAL_SURFACE('',#23995,6.95,0.785398163397446);
#21403=CONICAL_SURFACE('',#24088,0.8781,0.785398163397448);
#21404=CONICAL_SURFACE('',#24094,0.25,1.02974425867665);
#21405=CONICAL_SURFACE('',#24108,0.429999999999999,0.785398163397448);
#21406=CONICAL_SURFACE('',#24121,0.429999999999999,0.785398163397448);
#21407=CONICAL_SURFACE('',#24125,0.43,0.785398163397448);
#21408=CONICAL_SURFACE('',#24129,0.429999999999999,0.785398163397448);
#21409=CONICAL_SURFACE('',#24133,0.43,0.785398163397448);
#21410=CONICAL_SURFACE('',#24137,0.429999999999999,0.785398163397448);
#21411=CONICAL_SURFACE('',#24141,0.404999999999999,1.02974425867665);
#21412=CONICAL_SURFACE('',#24142,0.405,1.02974425867665);
#21413=CONICAL_SURFACE('',#24143,0.404999999999999,1.02974425867665);
#21414=CONICAL_SURFACE('',#24144,0.405,1.02974425867666);
#21415=CONICAL_SURFACE('',#24145,0.404999999999999,1.02974425867665);
#21416=CONICAL_SURFACE('',#24146,0.404999999999999,1.02974425867665);
#21417=CONICAL_SURFACE('',#24147,2.63,0.785398163397448);
#21418=CONICAL_SURFACE('',#24153,6.975,0.785398163397444);
#21419=CONICAL_SURFACE('',#24180,0.42,1.36540093760513);
#21420=CONICAL_SURFACE('',#24182,0.57,0.785398163397448);
#21421=CONICAL_SURFACE('',#24185,0.57,0.785398163397451);
#21422=CONICAL_SURFACE('',#24191,0.1625,1.29249666778979);
#21423=CONICAL_SURFACE('',#24218,0.78,0.785398163397448);
#21424=CONICAL_SURFACE('',#24222,0.78,0.785398163397449);
#21425=CONICAL_SURFACE('',#24228,0.53,0.785398163397449);
#21426=CONICAL_SURFACE('',#24232,1.88899277133291,0.209439510239319);
#21427=CONICAL_SURFACE('',#24269,1.96724457939162,0.20943951023932);
#21428=CONICAL_SURFACE('',#24306,2.06222171593972,1.36135681655558);
#21429=CONICAL_SURFACE('',#24307,1.79401563478481,1.36135681655558);
#21430=CONICAL_SURFACE('',#24314,0.32,0.0347685918560824);
#21431=CONICAL_SURFACE('',#24316,0.32,0.0347685918560824);
#21432=CONICAL_SURFACE('',#24326,0.32,0.0347685918560824);
#21433=CONICAL_SURFACE('',#24328,0.32,0.0347685918560824);
#21434=CONICAL_SURFACE('',#24338,0.32,0.0347685918560824);
#21435=CONICAL_SURFACE('',#24340,0.32,0.0347685918560824);
#21436=CONICAL_SURFACE('',#24350,0.32,0.0347685918560824);
#21437=CONICAL_SURFACE('',#24352,0.32,0.0347685918560824);
#21438=CONICAL_SURFACE('',#24362,0.32,0.0347685918560824);
#21439=CONICAL_SURFACE('',#24364,0.32,0.0347685918560824);
#21440=CONICAL_SURFACE('',#24374,0.32,0.0347685918560824);
#21441=CONICAL_SURFACE('',#24376,0.32,0.0347685918560824);
#21442=CONICAL_SURFACE('',#24386,0.32,0.0347685918560824);
#21443=CONICAL_SURFACE('',#24388,0.32,0.0347685918560824);
#21444=CONICAL_SURFACE('',#24398,0.32,0.0347685918560824);
#21445=CONICAL_SURFACE('',#24400,0.32,0.0347685918560824);
#21446=CONICAL_SURFACE('',#24410,0.32,0.0347685918560824);
#21447=CONICAL_SURFACE('',#24412,0.32,0.0347685918560824);
#21448=CONICAL_SURFACE('',#24422,0.32,0.0347685918560824);
#21449=CONICAL_SURFACE('',#24424,0.32,0.0347685918560824);
#21450=CONICAL_SURFACE('',#24434,0.32,0.0347685918560824);
#21451=CONICAL_SURFACE('',#24436,0.32,0.0347685918560824);
#21452=CONICAL_SURFACE('',#24446,0.32,0.0347685918560824);
#21453=CONICAL_SURFACE('',#24448,0.32,0.0347685918560824);
#21454=CONICAL_SURFACE('',#24458,0.32,0.0347685918560824);
#21455=CONICAL_SURFACE('',#24460,0.32,0.0347685918560824);
#21456=CONICAL_SURFACE('',#24470,0.32,0.0347685918560824);
#21457=CONICAL_SURFACE('',#24472,0.32,0.0347685918560824);
#21458=CONICAL_SURFACE('',#24482,0.32,0.0347685918560824);
#21459=CONICAL_SURFACE('',#24484,0.32,0.0347685918560824);
#21460=CONICAL_SURFACE('',#24494,0.32,0.0347685918560824);
#21461=CONICAL_SURFACE('',#24496,0.32,0.0347685918560824);
#21462=CONICAL_SURFACE('',#24508,0.32,0.0347685918560824);
#21463=CONICAL_SURFACE('',#24509,0.32,0.0347685918560824);
#21464=CONICAL_SURFACE('',#24514,0.32,0.0347685918560824);
#21465=CONICAL_SURFACE('',#24516,1.61107777577792,0.174532925199433);
#21466=CONICAL_SURFACE('',#24538,0.32,0.0347685918560824);
#21467=CONICAL_SURFACE('',#24542,0.32,0.0347685918560824);
#21468=CONICAL_SURFACE('',#24546,0.32,0.0347685918560824);
#21469=CONICAL_SURFACE('',#24550,0.32,0.0347685918560824);
#21470=CONICAL_SURFACE('',#24554,0.32,0.0347685918560824);
#21471=CONICAL_SURFACE('',#24558,0.32,0.0347685918560824);
#21472=CONICAL_SURFACE('',#24562,0.32,0.0347685918560824);
#21473=CONICAL_SURFACE('',#24566,0.32,0.0347685918560824);
#21474=CONICAL_SURFACE('',#24570,0.32,0.0347685918560824);
#21475=CONICAL_SURFACE('',#24574,0.32,0.0347685918560824);
#21476=CONICAL_SURFACE('',#24578,0.32,0.0347685918560824);
#21477=CONICAL_SURFACE('',#24582,0.32,0.0347685918560824);
#21478=CONICAL_SURFACE('',#24586,0.32,0.0347685918560824);
#21479=CONICAL_SURFACE('',#24590,0.32,0.0347685918560824);
#21480=CONICAL_SURFACE('',#24594,0.32,0.0347685918560824);
#21481=CONICAL_SURFACE('',#24596,0.32,0.0347685918560824);
#21482=CONICAL_SURFACE('',#24600,1.28,0.785398163397449);
#21483=CONICAL_SURFACE('',#24605,1.87,0.785398163397449);
#21484=CONICAL_SURFACE('',#24616,1.28,0.785398163397448);
#21485=CONICAL_SURFACE('',#24620,2.40256617975257,0.895793055792162);
#21486=CONICAL_SURFACE('',#24625,2.57,0.785398163397449);
#21487=CONICAL_SURFACE('',#24629,2.57,0.785398163397448);
#21488=CONICAL_SURFACE('',#24633,2.09090617619859,0.643931048266465);
#21489=CONICAL_SURFACE('',#24635,2.22173617797558,0.244346095279207);
#21490=CONICAL_SURFACE('',#24724,0.149995599935465,1.0303638848789);
#21491=CONICAL_SURFACE('',#24953,0.37,0.785398163397445);
#21492=CONICAL_SURFACE('',#24954,0.63,0.785398163397449);
#21493=CONICAL_SURFACE('',#24993,0.62,0.785398163397447);
#21494=CONICAL_SURFACE('',#25039,1.18258529610859,1.0471975511966);
#21495=CONICAL_SURFACE('',#25044,1.18258529610859,1.0471975511966);
#21496=CONICAL_SURFACE('',#25062,0.7931,0.785398163397448);
#21497=CONICAL_SURFACE('',#25066,0.77,0.785398163397445);
#21498=CONICAL_SURFACE('',#25070,0.49,0.209439510239319);
#21499=ADVANCED_FACE('',(#2669),#21316,.F.);
#21500=ADVANCED_FACE('',(#2670),#2409,.F.);
#21501=ADVANCED_FACE('',(#2671,#1599,#1600,#1601,#1602,#1603,#1604,#1605,
#1606,#1607,#1608),#1810,.T.);
#21502=ADVANCED_FACE('',(#2672),#21317,.F.);
#21503=ADVANCED_FACE('',(#2673,#1609,#1610,#1611,#1612,#1613,#1614,#1615,
#1616,#1617,#1618),#1811,.T.);
#21504=ADVANCED_FACE('',(#2674),#21318,.F.);
#21505=ADVANCED_FACE('',(#2675),#2410,.F.);
#21506=ADVANCED_FACE('',(#2676),#21319,.F.);
#21507=ADVANCED_FACE('',(#2677),#21320,.F.);
#21508=ADVANCED_FACE('',(#2678),#2411,.F.);
#21509=ADVANCED_FACE('',(#2679),#21321,.F.);
#21510=ADVANCED_FACE('',(#2680),#21322,.F.);
#21511=ADVANCED_FACE('',(#2681),#2412,.F.);
#21512=ADVANCED_FACE('',(#2682),#21323,.F.);
#21513=ADVANCED_FACE('',(#2683),#21324,.F.);
#21514=ADVANCED_FACE('',(#2684),#2413,.F.);
#21515=ADVANCED_FACE('',(#2685),#21325,.F.);
#21516=ADVANCED_FACE('',(#2686),#21326,.F.);
#21517=ADVANCED_FACE('',(#2687),#2414,.F.);
#21518=ADVANCED_FACE('',(#2688),#21327,.F.);
#21519=ADVANCED_FACE('',(#2689),#21328,.F.);
#21520=ADVANCED_FACE('',(#2690),#2415,.F.);
#21521=ADVANCED_FACE('',(#2691),#21329,.F.);
#21522=ADVANCED_FACE('',(#2692),#21330,.F.);
#21523=ADVANCED_FACE('',(#2693),#2416,.F.);
#21524=ADVANCED_FACE('',(#2694),#21331,.F.);
#21525=ADVANCED_FACE('',(#2695),#21332,.F.);
#21526=ADVANCED_FACE('',(#2696),#2417,.F.);
#21527=ADVANCED_FACE('',(#2697),#21333,.F.);
#21528=ADVANCED_FACE('',(#2698),#1595,.F.);
#21529=ADVANCED_FACE('',(#2699),#21334,.T.);
#21530=ADVANCED_FACE('',(#2700),#2418,.T.);
#21531=ADVANCED_FACE('',(#2701),#21335,.T.);
#21532=ADVANCED_FACE('',(#2702),#2419,.T.);
#21533=ADVANCED_FACE('',(#2703,#1619),#1812,.T.);
#21534=ADVANCED_FACE('',(#2704),#21336,.T.);
#21535=ADVANCED_FACE('',(#2705),#2420,.T.);
#21536=ADVANCED_FACE('',(#2706,#1620),#1813,.T.);
#21537=ADVANCED_FACE('',(#2707),#21337,.F.);
#21538=ADVANCED_FACE('',(#2708),#2421,.F.);
#21539=ADVANCED_FACE('',(#2709),#21338,.F.);
#21540=ADVANCED_FACE('',(#2710,#1621),#1814,.T.);
#21541=ADVANCED_FACE('',(#2711),#1596,.T.);
#21542=ADVANCED_FACE('',(#2712),#1815,.F.);
#21543=ADVANCED_FACE('',(#2713),#1816,.F.);
#21544=ADVANCED_FACE('',(#2714),#1817,.F.);
#21545=ADVANCED_FACE('',(#2715,#1622),#1818,.T.);
#21546=ADVANCED_FACE('',(#2716),#21339,.T.);
#21547=ADVANCED_FACE('',(#2717),#314,.T.);
#21548=ADVANCED_FACE('',(#2718),#21340,.F.);
#21549=ADVANCED_FACE('',(#2719),#2422,.F.);
#21550=ADVANCED_FACE('',(#2720),#315,.T.);
#21551=ADVANCED_FACE('',(#2721,#1623),#1819,.F.);
#21552=ADVANCED_FACE('',(#2722),#2423,.T.);
#21553=ADVANCED_FACE('',(#2723),#316,.T.);
#21554=ADVANCED_FACE('',(#2724),#2424,.T.);
#21555=ADVANCED_FACE('',(#2725),#21341,.T.);
#21556=ADVANCED_FACE('',(#2726),#1820,.T.);
#21557=ADVANCED_FACE('',(#2727),#1821,.T.);
#21558=ADVANCED_FACE('',(#2728),#1822,.T.);
#21559=ADVANCED_FACE('',(#2729),#1823,.F.);
#21560=ADVANCED_FACE('',(#2730),#1824,.F.);
#21561=ADVANCED_FACE('',(#2731),#317,.T.);
#21562=ADVANCED_FACE('',(#2732),#1825,.T.);
#21563=ADVANCED_FACE('',(#2733),#21342,.T.);
#21564=ADVANCED_FACE('',(#2734),#1826,.T.);
#21565=ADVANCED_FACE('',(#2735),#21343,.T.);
#21566=ADVANCED_FACE('',(#2736),#2425,.T.);
#21567=ADVANCED_FACE('',(#2737),#1827,.T.);
#21568=ADVANCED_FACE('',(#2738),#1828,.T.);
#21569=ADVANCED_FACE('',(#2739),#2426,.T.);
#21570=ADVANCED_FACE('',(#2740),#1829,.T.);
#21571=ADVANCED_FACE('',(#2741),#1830,.F.);
#21572=ADVANCED_FACE('',(#2742),#2427,.F.);
#21573=ADVANCED_FACE('',(#2743),#2428,.T.);
#21574=ADVANCED_FACE('',(#2744,#1624),#1831,.F.);
#21575=ADVANCED_FACE('',(#2745,#1625),#1832,.T.);
#21576=ADVANCED_FACE('',(#2746),#21344,.T.);
#21577=ADVANCED_FACE('',(#2747),#2429,.T.);
#21578=ADVANCED_FACE('',(#2748,#1626),#1833,.T.);
#21579=ADVANCED_FACE('',(#2749),#21345,.T.);
#21580=ADVANCED_FACE('',(#2750,#1627),#1834,.T.);
#21581=ADVANCED_FACE('',(#2751),#2430,.F.);
#21582=ADVANCED_FACE('',(#2752),#2431,.F.);
#21583=ADVANCED_FACE('',(#2753),#21346,.F.);
#21584=ADVANCED_FACE('',(#2754),#2432,.F.);
#21585=ADVANCED_FACE('',(#2755),#21347,.F.);
#21586=ADVANCED_FACE('',(#2756),#2433,.F.);
#21587=ADVANCED_FACE('',(#2757),#21348,.F.);
#21588=ADVANCED_FACE('',(#2758,#1628),#1835,.T.);
#21589=ADVANCED_FACE('',(#2759),#2434,.T.);
#21590=ADVANCED_FACE('',(#2760),#2435,.T.);
#21591=ADVANCED_FACE('',(#2761),#2436,.T.);
#21592=ADVANCED_FACE('',(#2762),#2437,.T.);
#21593=ADVANCED_FACE('',(#2763),#2438,.T.);
#21594=ADVANCED_FACE('',(#2764),#2439,.T.);
#21595=ADVANCED_FACE('',(#2765),#2440,.T.);
#21596=ADVANCED_FACE('',(#2766),#2441,.T.);
#21597=ADVANCED_FACE('',(#2767),#318,.T.);
#21598=ADVANCED_FACE('',(#2768),#319,.F.);
#21599=ADVANCED_FACE('',(#2769),#320,.F.);
#21600=ADVANCED_FACE('',(#2770),#1836,.T.);
#21601=ADVANCED_FACE('',(#2771),#2442,.T.);
#21602=ADVANCED_FACE('',(#2772),#321,.F.);
#21603=ADVANCED_FACE('',(#2773),#322,.F.);
#21604=ADVANCED_FACE('',(#2774),#323,.T.);
#21605=ADVANCED_FACE('',(#2775),#1837,.F.);
#21606=ADVANCED_FACE('',(#2776),#1838,.F.);
#21607=ADVANCED_FACE('',(#2777),#1839,.F.);
#21608=ADVANCED_FACE('',(#2778),#1840,.F.);
#21609=ADVANCED_FACE('',(#2779),#1841,.F.);
#21610=ADVANCED_FACE('',(#2780),#1842,.F.);
#21611=ADVANCED_FACE('',(#2781),#1843,.F.);
#21612=ADVANCED_FACE('',(#2782),#1844,.F.);
#21613=ADVANCED_FACE('',(#2783),#1845,.F.);
#21614=ADVANCED_FACE('',(#2784),#1846,.F.);
#21615=ADVANCED_FACE('',(#2785),#1847,.F.);
#21616=ADVANCED_FACE('',(#2786),#1848,.F.);
#21617=ADVANCED_FACE('',(#2787),#1849,.F.);
#21618=ADVANCED_FACE('',(#2788),#1850,.F.);
#21619=ADVANCED_FACE('',(#2789),#1851,.F.);
#21620=ADVANCED_FACE('',(#2790),#1852,.F.);
#21621=ADVANCED_FACE('',(#2791),#1853,.F.);
#21622=ADVANCED_FACE('',(#2792),#1854,.F.);
#21623=ADVANCED_FACE('',(#2793),#1855,.F.);
#21624=ADVANCED_FACE('',(#2794),#1856,.F.);
#21625=ADVANCED_FACE('',(#2795),#1857,.F.);
#21626=ADVANCED_FACE('',(#2796),#1858,.F.);
#21627=ADVANCED_FACE('',(#2797),#1859,.F.);
#21628=ADVANCED_FACE('',(#2798),#1860,.F.);
#21629=ADVANCED_FACE('',(#2799),#1861,.F.);
#21630=ADVANCED_FACE('',(#2800),#1862,.F.);
#21631=ADVANCED_FACE('',(#2801),#1863,.F.);
#21632=ADVANCED_FACE('',(#2802),#1864,.F.);
#21633=ADVANCED_FACE('',(#2803),#1865,.F.);
#21634=ADVANCED_FACE('',(#2804),#1866,.F.);
#21635=ADVANCED_FACE('',(#2805),#1867,.F.);
#21636=ADVANCED_FACE('',(#2806),#1868,.F.);
#21637=ADVANCED_FACE('',(#2807),#1869,.F.);
#21638=ADVANCED_FACE('',(#2808),#1870,.F.);
#21639=ADVANCED_FACE('',(#2809),#1871,.F.);
#21640=ADVANCED_FACE('',(#2810),#1872,.F.);
#21641=ADVANCED_FACE('',(#2811),#1873,.F.);
#21642=ADVANCED_FACE('',(#2812),#1874,.F.);
#21643=ADVANCED_FACE('',(#2813),#1875,.F.);
#21644=ADVANCED_FACE('',(#2814),#1876,.F.);
#21645=ADVANCED_FACE('',(#2815),#1877,.F.);
#21646=ADVANCED_FACE('',(#2816),#1878,.F.);
#21647=ADVANCED_FACE('',(#2817),#1879,.F.);
#21648=ADVANCED_FACE('',(#2818),#1880,.F.);
#21649=ADVANCED_FACE('',(#2819),#1881,.F.);
#21650=ADVANCED_FACE('',(#2820),#1882,.F.);
#21651=ADVANCED_FACE('',(#2821),#1883,.F.);
#21652=ADVANCED_FACE('',(#2822),#1884,.F.);
#21653=ADVANCED_FACE('',(#2823),#1885,.F.);
#21654=ADVANCED_FACE('',(#2824),#1886,.F.);
#21655=ADVANCED_FACE('',(#2825),#1887,.F.);
#21656=ADVANCED_FACE('',(#2826),#1888,.F.);
#21657=ADVANCED_FACE('',(#2827),#1889,.F.);
#21658=ADVANCED_FACE('',(#2828),#1890,.F.);
#21659=ADVANCED_FACE('',(#2829),#1891,.F.);
#21660=ADVANCED_FACE('',(#2830),#1892,.F.);
#21661=ADVANCED_FACE('',(#2831),#1893,.F.);
#21662=ADVANCED_FACE('',(#2832),#1894,.F.);
#21663=ADVANCED_FACE('',(#2833),#1895,.F.);
#21664=ADVANCED_FACE('',(#2834),#1896,.F.);
#21665=ADVANCED_FACE('',(#2835),#1897,.F.);
#21666=ADVANCED_FACE('',(#2836),#1898,.F.);
#21667=ADVANCED_FACE('',(#2837),#1899,.F.);
#21668=ADVANCED_FACE('',(#2838),#1900,.F.);
#21669=ADVANCED_FACE('',(#2839),#1901,.F.);
#21670=ADVANCED_FACE('',(#2840),#1902,.F.);
#21671=ADVANCED_FACE('',(#2841),#1903,.F.);
#21672=ADVANCED_FACE('',(#2842),#1904,.F.);
#21673=ADVANCED_FACE('',(#2843),#1905,.F.);
#21674=ADVANCED_FACE('',(#2844),#1906,.F.);
#21675=ADVANCED_FACE('',(#2845),#1907,.F.);
#21676=ADVANCED_FACE('',(#2846),#1908,.F.);
#21677=ADVANCED_FACE('',(#2847),#1909,.F.);
#21678=ADVANCED_FACE('',(#2848),#1910,.F.);
#21679=ADVANCED_FACE('',(#2849),#1911,.F.);
#21680=ADVANCED_FACE('',(#2850),#1912,.F.);
#21681=ADVANCED_FACE('',(#2851),#1913,.F.);
#21682=ADVANCED_FACE('',(#2852),#1914,.F.);
#21683=ADVANCED_FACE('',(#2853),#1915,.F.);
#21684=ADVANCED_FACE('',(#2854),#1916,.F.);
#21685=ADVANCED_FACE('',(#2855),#1917,.F.);
#21686=ADVANCED_FACE('',(#2856),#1918,.F.);
#21687=ADVANCED_FACE('',(#2857),#1919,.F.);
#21688=ADVANCED_FACE('',(#2858),#1920,.F.);
#21689=ADVANCED_FACE('',(#2859),#1921,.F.);
#21690=ADVANCED_FACE('',(#2860),#1922,.F.);
#21691=ADVANCED_FACE('',(#2861),#1923,.F.);
#21692=ADVANCED_FACE('',(#2862),#1924,.F.);
#21693=ADVANCED_FACE('',(#2863),#1925,.F.);
#21694=ADVANCED_FACE('',(#2864),#1926,.F.);
#21695=ADVANCED_FACE('',(#2865),#1927,.F.);
#21696=ADVANCED_FACE('',(#2866),#1928,.F.);
#21697=ADVANCED_FACE('',(#2867),#1929,.F.);
#21698=ADVANCED_FACE('',(#2868),#1930,.F.);
#21699=ADVANCED_FACE('',(#2869),#1931,.F.);
#21700=ADVANCED_FACE('',(#2870),#1932,.F.);
#21701=ADVANCED_FACE('',(#2871),#1933,.F.);
#21702=ADVANCED_FACE('',(#2872),#1934,.F.);
#21703=ADVANCED_FACE('',(#2873),#1935,.F.);
#21704=ADVANCED_FACE('',(#2874),#1936,.F.);
#21705=ADVANCED_FACE('',(#2875),#1937,.F.);
#21706=ADVANCED_FACE('',(#2876),#1938,.F.);
#21707=ADVANCED_FACE('',(#2877),#1939,.F.);
#21708=ADVANCED_FACE('',(#2878),#1940,.F.);
#21709=ADVANCED_FACE('',(#2879),#1941,.F.);
#21710=ADVANCED_FACE('',(#2880),#1942,.F.);
#21711=ADVANCED_FACE('',(#2881),#1943,.F.);
#21712=ADVANCED_FACE('',(#2882),#1944,.F.);
#21713=ADVANCED_FACE('',(#2883),#1945,.F.);
#21714=ADVANCED_FACE('',(#2884),#1946,.F.);
#21715=ADVANCED_FACE('',(#2885),#1947,.F.);
#21716=ADVANCED_FACE('',(#2886),#1948,.F.);
#21717=ADVANCED_FACE('',(#2887),#1949,.F.);
#21718=ADVANCED_FACE('',(#2888),#1950,.F.);
#21719=ADVANCED_FACE('',(#2889),#1951,.F.);
#21720=ADVANCED_FACE('',(#2890),#1952,.F.);
#21721=ADVANCED_FACE('',(#2891),#1953,.F.);
#21722=ADVANCED_FACE('',(#2892),#1954,.F.);
#21723=ADVANCED_FACE('',(#2893),#1955,.F.);
#21724=ADVANCED_FACE('',(#2894),#1956,.F.);
#21725=ADVANCED_FACE('',(#2895),#1957,.F.);
#21726=ADVANCED_FACE('',(#2896),#1958,.F.);
#21727=ADVANCED_FACE('',(#2897),#1959,.F.);
#21728=ADVANCED_FACE('',(#2898),#1960,.F.);
#21729=ADVANCED_FACE('',(#2899),#1961,.F.);
#21730=ADVANCED_FACE('',(#2900),#1962,.F.);
#21731=ADVANCED_FACE('',(#2901),#1963,.F.);
#21732=ADVANCED_FACE('',(#2902),#21349,.T.);
#21733=ADVANCED_FACE('',(#2903),#1964,.T.);
#21734=ADVANCED_FACE('',(#2904),#1965,.T.);
#21735=ADVANCED_FACE('',(#2905),#1966,.T.);
#21736=ADVANCED_FACE('',(#2906),#21350,.T.);
#21737=ADVANCED_FACE('',(#2907),#1967,.T.);
#21738=ADVANCED_FACE('',(#2908,#1629),#1968,.T.);
#21739=ADVANCED_FACE('',(#2909,#1630),#1969,.F.);
#21740=ADVANCED_FACE('',(#2910),#1970,.T.);
#21741=ADVANCED_FACE('',(#2911),#1971,.T.);
#21742=ADVANCED_FACE('',(#2912),#2443,.F.);
#21743=ADVANCED_FACE('',(#2913),#21351,.F.);
#21744=ADVANCED_FACE('',(#2914,#1631),#1972,.T.);
#21745=ADVANCED_FACE('',(#2915),#21352,.T.);
#21746=ADVANCED_FACE('',(#2916,#1632),#1973,.T.);
#21747=ADVANCED_FACE('',(#2917),#2444,.T.);
#21748=ADVANCED_FACE('',(#2918),#2445,.T.);
#21749=ADVANCED_FACE('',(#2919),#21353,.T.);
#21750=ADVANCED_FACE('',(#2920,#1633),#1974,.T.);
#21751=ADVANCED_FACE('',(#2921),#2446,.T.);
#21752=ADVANCED_FACE('',(#2922),#2447,.T.);
#21753=ADVANCED_FACE('',(#2923),#2448,.T.);
#21754=ADVANCED_FACE('',(#2924),#2449,.T.);
#21755=ADVANCED_FACE('',(#2925),#2450,.T.);
#21756=ADVANCED_FACE('',(#2926),#2451,.T.);
#21757=ADVANCED_FACE('',(#2927),#2452,.T.);
#21758=ADVANCED_FACE('',(#2928),#2453,.T.);
#21759=ADVANCED_FACE('',(#2929),#2454,.T.);
#21760=ADVANCED_FACE('',(#2930),#2455,.T.);
#21761=ADVANCED_FACE('',(#2931),#2456,.T.);
#21762=ADVANCED_FACE('',(#2932),#2457,.T.);
#21763=ADVANCED_FACE('',(#2933),#2458,.T.);
#21764=ADVANCED_FACE('',(#2934),#2459,.T.);
#21765=ADVANCED_FACE('',(#2935),#2460,.T.);
#21766=ADVANCED_FACE('',(#2936),#2461,.T.);
#21767=ADVANCED_FACE('',(#2937),#2462,.T.);
#21768=ADVANCED_FACE('',(#2938),#2463,.T.);
#21769=ADVANCED_FACE('',(#2939),#2464,.T.);
#21770=ADVANCED_FACE('',(#2940),#1975,.F.);
#21771=ADVANCED_FACE('',(#2941),#324,.F.);
#21772=ADVANCED_FACE('',(#2942),#2465,.T.);
#21773=ADVANCED_FACE('',(#2943),#325,.F.);
#21774=ADVANCED_FACE('',(#2944),#2466,.T.);
#21775=ADVANCED_FACE('',(#2945),#326,.T.);
#21776=ADVANCED_FACE('',(#2946),#327,.F.);
#21777=ADVANCED_FACE('',(#2947),#328,.F.);
#21778=ADVANCED_FACE('',(#2948),#1976,.T.);
#21779=ADVANCED_FACE('',(#2949),#2467,.T.);
#21780=ADVANCED_FACE('',(#2950),#329,.F.);
#21781=ADVANCED_FACE('',(#2951),#330,.F.);
#21782=ADVANCED_FACE('',(#2952),#331,.T.);
#21783=ADVANCED_FACE('',(#2953),#21354,.T.);
#21784=ADVANCED_FACE('',(#2954),#1977,.T.);
#21785=ADVANCED_FACE('',(#2955),#1978,.T.);
#21786=ADVANCED_FACE('',(#2956),#1979,.T.);
#21787=ADVANCED_FACE('',(#2957),#21355,.T.);
#21788=ADVANCED_FACE('',(#2958),#1980,.T.);
#21789=ADVANCED_FACE('',(#2959,#1634),#1981,.T.);
#21790=ADVANCED_FACE('',(#2960),#1982,.T.);
#21791=ADVANCED_FACE('',(#2961,#1635),#1983,.F.);
#21792=ADVANCED_FACE('',(#2962),#1984,.F.);
#21793=ADVANCED_FACE('',(#2963),#1985,.T.);
#21794=ADVANCED_FACE('',(#2964),#1986,.T.);
#21795=ADVANCED_FACE('',(#2965),#2468,.F.);
#21796=ADVANCED_FACE('',(#2966),#2469,.F.);
#21797=ADVANCED_FACE('',(#2967,#1636),#1987,.T.);
#21798=ADVANCED_FACE('',(#2968),#21356,.T.);
#21799=ADVANCED_FACE('',(#2969,#1637),#1988,.T.);
#21800=ADVANCED_FACE('',(#2970),#2470,.T.);
#21801=ADVANCED_FACE('',(#2971),#21357,.T.);
#21802=ADVANCED_FACE('',(#2972,#1638),#1989,.T.);
#21803=ADVANCED_FACE('',(#2973),#21358,.F.);
#21804=ADVANCED_FACE('',(#2974),#21359,.F.);
#21805=ADVANCED_FACE('',(#2975),#21360,.F.);
#21806=ADVANCED_FACE('',(#2976),#1990,.F.);
#21807=ADVANCED_FACE('',(#2977),#2471,.F.);
#21808=ADVANCED_FACE('',(#2978),#1991,.F.);
#21809=ADVANCED_FACE('',(#2979),#2472,.F.);
#21810=ADVANCED_FACE('',(#2980),#1992,.T.);
#21811=ADVANCED_FACE('',(#2981),#1993,.F.);
#21812=ADVANCED_FACE('',(#2982),#2473,.F.);
#21813=ADVANCED_FACE('',(#2983),#1994,.F.);
#21814=ADVANCED_FACE('',(#2984),#2474,.F.);
#21815=ADVANCED_FACE('',(#2985),#1995,.T.);
#21816=ADVANCED_FACE('',(#2986,#1639),#1996,.T.);
#21817=ADVANCED_FACE('',(#2987),#21361,.T.);
#21818=ADVANCED_FACE('',(#2988,#1640),#2475,.T.);
#21819=ADVANCED_FACE('',(#2989,#1641),#1997,.T.);
#21820=ADVANCED_FACE('',(#2990),#21362,.T.);
#21821=ADVANCED_FACE('',(#2991),#2476,.T.);
#21822=ADVANCED_FACE('',(#2992,#1642),#1998,.T.);
#21823=ADVANCED_FACE('',(#2993),#2477,.T.);
#21824=ADVANCED_FACE('',(#2994,#1643),#1999,.T.);
#21825=ADVANCED_FACE('',(#2995,#1644),#2478,.T.);
#21826=ADVANCED_FACE('',(#2996,#1645),#2000,.T.);
#21827=ADVANCED_FACE('',(#2997),#2479,.T.);
#21828=ADVANCED_FACE('',(#2998,#1646),#2001,.T.);
#21829=ADVANCED_FACE('',(#2999),#2480,.T.);
#21830=ADVANCED_FACE('',(#3000),#21363,.T.);
#21831=ADVANCED_FACE('',(#3001),#2002,.T.);
#21832=ADVANCED_FACE('',(#3002,#1647),#2003,.F.);
#21833=ADVANCED_FACE('',(#3003),#2481,.T.);
#21834=ADVANCED_FACE('',(#3004,#1648),#2004,.F.);
#21835=ADVANCED_FACE('',(#3005),#2482,.T.);
#21836=ADVANCED_FACE('',(#3006),#2005,.F.);
#21837=ADVANCED_FACE('',(#3007),#2006,.F.);
#21838=ADVANCED_FACE('',(#3008),#2007,.F.);
#21839=ADVANCED_FACE('',(#3009,#1649),#2008,.T.);
#21840=ADVANCED_FACE('',(#3010),#2483,.F.);
#21841=ADVANCED_FACE('',(#3011),#2484,.F.);
#21842=ADVANCED_FACE('',(#3012),#2485,.F.);
#21843=ADVANCED_FACE('',(#3013),#2486,.F.);
#21844=ADVANCED_FACE('',(#3014),#2487,.F.);
#21845=ADVANCED_FACE('',(#3015),#2488,.F.);
#21846=ADVANCED_FACE('',(#3016),#2489,.F.);
#21847=ADVANCED_FACE('',(#3017),#2490,.F.);
#21848=ADVANCED_FACE('',(#3018),#2491,.F.);
#21849=ADVANCED_FACE('',(#3019),#2492,.F.);
#21850=ADVANCED_FACE('',(#3020,#1650),#2009,.F.);
#21851=ADVANCED_FACE('',(#3021),#2493,.F.);
#21852=ADVANCED_FACE('',(#3022,#1651),#2010,.F.);
#21853=ADVANCED_FACE('',(#3023),#2494,.F.);
#21854=ADVANCED_FACE('',(#3024,#1652),#2011,.F.);
#21855=ADVANCED_FACE('',(#3025),#2495,.F.);
#21856=ADVANCED_FACE('',(#3026,#1653),#2012,.F.);
#21857=ADVANCED_FACE('',(#3027),#2496,.F.);
#21858=ADVANCED_FACE('',(#3028,#1654),#2013,.F.);
#21859=ADVANCED_FACE('',(#3029),#2497,.F.);
#21860=ADVANCED_FACE('',(#3030,#1655),#2014,.F.);
#21861=ADVANCED_FACE('',(#3031),#2498,.F.);
#21862=ADVANCED_FACE('',(#3032,#1656),#2015,.F.);
#21863=ADVANCED_FACE('',(#3033),#2499,.F.);
#21864=ADVANCED_FACE('',(#3034,#1657),#2016,.F.);
#21865=ADVANCED_FACE('',(#3035),#2500,.F.);
#21866=ADVANCED_FACE('',(#3036,#1658),#2017,.F.);
#21867=ADVANCED_FACE('',(#3037,#1659),#2018,.T.);
#21868=ADVANCED_FACE('',(#3038),#2501,.F.);
#21869=ADVANCED_FACE('',(#3039),#21364,.F.);
#21870=ADVANCED_FACE('',(#3040),#21365,.T.);
#21871=ADVANCED_FACE('',(#3041),#2502,.T.);
#21872=ADVANCED_FACE('',(#3042),#21366,.T.);
#21873=ADVANCED_FACE('',(#3043,#1660,#1661,#1662,#1663,#1664,#1665,#1666,
#1667,#1668,#1669),#2019,.T.);
#21874=ADVANCED_FACE('',(#3044),#2503,.F.);
#21875=ADVANCED_FACE('',(#3045),#2020,.F.);
#21876=ADVANCED_FACE('',(#3046),#2021,.F.);
#21877=ADVANCED_FACE('',(#3047),#2022,.F.);
#21878=ADVANCED_FACE('',(#3048),#2023,.F.);
#21879=ADVANCED_FACE('',(#3049),#2504,.T.);
#21880=ADVANCED_FACE('',(#3050),#2024,.F.);
#21881=ADVANCED_FACE('',(#3051),#2505,.F.);
#21882=ADVANCED_FACE('',(#3052),#2025,.F.);
#21883=ADVANCED_FACE('',(#3053),#21367,.F.);
#21884=ADVANCED_FACE('',(#3054,#1670),#2026,.F.);
#21885=ADVANCED_FACE('',(#3055),#2506,.F.);
#21886=ADVANCED_FACE('',(#3056),#21368,.F.);
#21887=ADVANCED_FACE('',(#3057,#1671),#2027,.F.);
#21888=ADVANCED_FACE('',(#3058),#2507,.F.);
#21889=ADVANCED_FACE('',(#3059),#21369,.F.);
#21890=ADVANCED_FACE('',(#3060,#1672),#2028,.F.);
#21891=ADVANCED_FACE('',(#3061),#2508,.F.);
#21892=ADVANCED_FACE('',(#3062),#21370,.F.);
#21893=ADVANCED_FACE('',(#3063,#1673),#2029,.F.);
#21894=ADVANCED_FACE('',(#3064),#2509,.F.);
#21895=ADVANCED_FACE('',(#3065),#21371,.F.);
#21896=ADVANCED_FACE('',(#3066,#1674),#2030,.F.);
#21897=ADVANCED_FACE('',(#3067),#2510,.F.);
#21898=ADVANCED_FACE('',(#3068),#21372,.F.);
#21899=ADVANCED_FACE('',(#3069,#1675),#2031,.F.);
#21900=ADVANCED_FACE('',(#3070),#2511,.F.);
#21901=ADVANCED_FACE('',(#3071),#2512,.F.);
#21902=ADVANCED_FACE('',(#3072),#310,.F.);
#21903=ADVANCED_FACE('',(#3073),#2513,.F.);
#21904=ADVANCED_FACE('',(#3074,#1676),#2032,.T.);
#21905=ADVANCED_FACE('',(#3075),#2514,.F.);
#21906=ADVANCED_FACE('',(#3076),#2515,.F.);
#21907=ADVANCED_FACE('',(#3077),#2516,.F.);
#21908=ADVANCED_FACE('',(#3078),#2517,.F.);
#21909=ADVANCED_FACE('',(#3079),#21373,.F.);
#21910=ADVANCED_FACE('',(#3080),#2518,.F.);
#21911=ADVANCED_FACE('',(#3081,#1677),#2033,.T.);
#21912=ADVANCED_FACE('',(#3082),#21374,.T.);
#21913=ADVANCED_FACE('',(#3083),#2519,.T.);
#21914=ADVANCED_FACE('',(#3084),#21375,.F.);
#21915=ADVANCED_FACE('',(#3085,#1678,#1679,#1680,#1681,#1682,#1683,#1684),
#2034,.T.);
#21916=ADVANCED_FACE('',(#3086,#1685),#2520,.F.);
#21917=ADVANCED_FACE('',(#3087),#21376,.F.);
#21918=ADVANCED_FACE('',(#3088),#2521,.F.);
#21919=ADVANCED_FACE('',(#3089,#1686,#1687),#2035,.T.);
#21920=ADVANCED_FACE('',(#3090),#311,.T.);
#21921=ADVANCED_FACE('',(#3091,#1688),#2522,.T.);
#21922=ADVANCED_FACE('',(#3092),#21377,.T.);
#21923=ADVANCED_FACE('',(#3093),#21378,.T.);
#21924=ADVANCED_FACE('',(#3094),#2523,.T.);
#21925=ADVANCED_FACE('',(#3095),#21379,.T.);
#21926=ADVANCED_FACE('',(#3096),#2524,.T.);
#21927=ADVANCED_FACE('',(#3097),#21380,.T.);
#21928=ADVANCED_FACE('',(#3098,#1689),#2036,.T.);
#21929=ADVANCED_FACE('',(#3099),#2525,.F.);
#21930=ADVANCED_FACE('',(#3100,#1690),#2037,.T.);
#21931=ADVANCED_FACE('',(#3101),#2526,.F.);
#21932=ADVANCED_FACE('',(#3102,#1691),#2038,.T.);
#21933=ADVANCED_FACE('',(#3103),#2527,.F.);
#21934=ADVANCED_FACE('',(#3104,#1692),#2039,.T.);
#21935=ADVANCED_FACE('',(#3105),#2528,.F.);
#21936=ADVANCED_FACE('',(#3106,#1693),#2040,.T.);
#21937=ADVANCED_FACE('',(#3107),#21381,.F.);
#21938=ADVANCED_FACE('',(#3108),#2529,.F.);
#21939=ADVANCED_FACE('',(#3109,#1694,#1695,#1696,#1697,#1698,#1699,#1700,
#1701),#2041,.T.);
#21940=ADVANCED_FACE('',(#3110),#21382,.F.);
#21941=ADVANCED_FACE('',(#3111,#1702,#1703,#1704,#1705,#1706,#1707,#1708,
#1709,#1710),#2042,.T.);
#21942=ADVANCED_FACE('',(#3112),#21383,.F.);
#21943=ADVANCED_FACE('',(#3113),#2530,.F.);
#21944=ADVANCED_FACE('',(#3114),#21384,.F.);
#21945=ADVANCED_FACE('',(#3115),#21385,.F.);
#21946=ADVANCED_FACE('',(#3116),#2531,.F.);
#21947=ADVANCED_FACE('',(#3117),#21386,.F.);
#21948=ADVANCED_FACE('',(#3118),#21387,.F.);
#21949=ADVANCED_FACE('',(#3119),#2532,.F.);
#21950=ADVANCED_FACE('',(#3120),#21388,.F.);
#21951=ADVANCED_FACE('',(#3121),#21389,.F.);
#21952=ADVANCED_FACE('',(#3122),#2533,.F.);
#21953=ADVANCED_FACE('',(#3123),#21390,.F.);
#21954=ADVANCED_FACE('',(#3124),#21391,.F.);
#21955=ADVANCED_FACE('',(#3125),#2534,.F.);
#21956=ADVANCED_FACE('',(#3126),#21392,.F.);
#21957=ADVANCED_FACE('',(#3127),#2535,.F.);
#21958=ADVANCED_FACE('',(#3128),#21393,.F.);
#21959=ADVANCED_FACE('',(#3129),#2536,.F.);
#21960=ADVANCED_FACE('',(#3130,#1711),#2043,.T.);
#21961=ADVANCED_FACE('',(#3131),#21394,.F.);
#21962=ADVANCED_FACE('',(#3132),#2537,.F.);
#21963=ADVANCED_FACE('',(#3133,#1712),#2044,.F.);
#21964=ADVANCED_FACE('',(#3134),#2538,.F.);
#21965=ADVANCED_FACE('',(#3135),#2539,.F.);
#21966=ADVANCED_FACE('',(#3136,#1713),#2045,.F.);
#21967=ADVANCED_FACE('',(#3137),#21395,.F.);
#21968=ADVANCED_FACE('',(#3138),#2540,.T.);
#21969=ADVANCED_FACE('',(#3139),#2046,.F.);
#21970=ADVANCED_FACE('',(#3140),#21396,.T.);
#21971=ADVANCED_FACE('',(#3141),#2541,.T.);
#21972=ADVANCED_FACE('',(#3142),#21397,.T.);
#21973=ADVANCED_FACE('',(#3143,#1714),#2542,.F.);
#21974=ADVANCED_FACE('',(#3144),#2543,.F.);
#21975=ADVANCED_FACE('',(#3145),#21398,.F.);
#21976=ADVANCED_FACE('',(#3146,#1715),#2047,.F.);
#21977=ADVANCED_FACE('',(#3147),#2544,.T.);
#21978=ADVANCED_FACE('',(#3148),#2048,.F.);
#21979=ADVANCED_FACE('',(#3149),#2545,.F.);
#21980=ADVANCED_FACE('',(#3150),#2546,.F.);
#21981=ADVANCED_FACE('',(#3151),#2547,.F.);
#21982=ADVANCED_FACE('',(#3152),#2049,.F.);
#21983=ADVANCED_FACE('',(#3153),#2548,.F.);
#21984=ADVANCED_FACE('',(#3154),#2549,.F.);
#21985=ADVANCED_FACE('',(#3155),#2550,.F.);
#21986=ADVANCED_FACE('',(#3156),#2050,.F.);
#21987=ADVANCED_FACE('',(#3157),#21399,.F.);
#21988=ADVANCED_FACE('',(#3158),#2551,.F.);
#21989=ADVANCED_FACE('',(#3159),#21400,.F.);
#21990=ADVANCED_FACE('',(#3160),#21401,.T.);
#21991=ADVANCED_FACE('',(#3161),#2552,.T.);
#21992=ADVANCED_FACE('',(#3162),#21402,.T.);
#21993=ADVANCED_FACE('',(#3163),#332,.F.);
#21994=ADVANCED_FACE('',(#3164),#333,.F.);
#21995=ADVANCED_FACE('',(#3165),#334,.F.);
#21996=ADVANCED_FACE('',(#3166),#335,.F.);
#21997=ADVANCED_FACE('',(#3167),#336,.F.);
#21998=ADVANCED_FACE('',(#3168),#337,.F.);
#21999=ADVANCED_FACE('',(#3169),#338,.F.);
#22000=ADVANCED_FACE('',(#3170),#339,.F.);
#22001=ADVANCED_FACE('',(#3171),#340,.F.);
#22002=ADVANCED_FACE('',(#3172),#2051,.F.);
#22003=ADVANCED_FACE('',(#3173),#341,.F.);
#22004=ADVANCED_FACE('',(#3174),#342,.F.);
#22005=ADVANCED_FACE('',(#3175),#2052,.F.);
#22006=ADVANCED_FACE('',(#3176),#343,.F.);
#22007=ADVANCED_FACE('',(#3177),#344,.F.);
#22008=ADVANCED_FACE('',(#3178),#345,.F.);
#22009=ADVANCED_FACE('',(#3179),#346,.F.);
#22010=ADVANCED_FACE('',(#3180),#347,.F.);
#22011=ADVANCED_FACE('',(#3181),#348,.F.);
#22012=ADVANCED_FACE('',(#3182),#349,.F.);
#22013=ADVANCED_FACE('',(#3183),#2053,.F.);
#22014=ADVANCED_FACE('',(#3184),#350,.F.);
#22015=ADVANCED_FACE('',(#3185),#351,.F.);
#22016=ADVANCED_FACE('',(#3186),#352,.F.);
#22017=ADVANCED_FACE('',(#3187),#353,.F.);
#22018=ADVANCED_FACE('',(#3188),#354,.F.);
#22019=ADVANCED_FACE('',(#3189),#355,.F.);
#22020=ADVANCED_FACE('',(#3190),#356,.F.);
#22021=ADVANCED_FACE('',(#3191),#357,.F.);
#22022=ADVANCED_FACE('',(#3192),#358,.F.);
#22023=ADVANCED_FACE('',(#3193),#359,.F.);
#22024=ADVANCED_FACE('',(#3194),#360,.F.);
#22025=ADVANCED_FACE('',(#3195),#361,.F.);
#22026=ADVANCED_FACE('',(#3196),#362,.F.);
#22027=ADVANCED_FACE('',(#3197),#363,.F.);
#22028=ADVANCED_FACE('',(#3198),#364,.F.);
#22029=ADVANCED_FACE('',(#3199),#2054,.F.);
#22030=ADVANCED_FACE('',(#3200,#1716),#2055,.T.);
#22031=ADVANCED_FACE('',(#3201),#365,.F.);
#22032=ADVANCED_FACE('',(#3202),#366,.F.);
#22033=ADVANCED_FACE('',(#3203),#367,.F.);
#22034=ADVANCED_FACE('',(#3204),#368,.F.);
#22035=ADVANCED_FACE('',(#3205),#369,.F.);
#22036=ADVANCED_FACE('',(#3206),#370,.F.);
#22037=ADVANCED_FACE('',(#3207),#371,.F.);
#22038=ADVANCED_FACE('',(#3208),#372,.F.);
#22039=ADVANCED_FACE('',(#3209),#373,.F.);
#22040=ADVANCED_FACE('',(#3210),#374,.F.);
#22041=ADVANCED_FACE('',(#3211),#375,.F.);
#22042=ADVANCED_FACE('',(#3212),#376,.F.);
#22043=ADVANCED_FACE('',(#3213),#377,.F.);
#22044=ADVANCED_FACE('',(#3214),#378,.F.);
#22045=ADVANCED_FACE('',(#3215),#379,.F.);
#22046=ADVANCED_FACE('',(#3216),#380,.F.);
#22047=ADVANCED_FACE('',(#3217),#381,.F.);
#22048=ADVANCED_FACE('',(#3218),#382,.F.);
#22049=ADVANCED_FACE('',(#3219),#383,.F.);
#22050=ADVANCED_FACE('',(#3220),#384,.F.);
#22051=ADVANCED_FACE('',(#3221,#1717),#2056,.T.);
#22052=ADVANCED_FACE('',(#3222),#385,.F.);
#22053=ADVANCED_FACE('',(#3223),#386,.F.);
#22054=ADVANCED_FACE('',(#3224),#2057,.F.);
#22055=ADVANCED_FACE('',(#3225),#387,.F.);
#22056=ADVANCED_FACE('',(#3226),#388,.F.);
#22057=ADVANCED_FACE('',(#3227),#2058,.F.);
#22058=ADVANCED_FACE('',(#3228),#2059,.F.);
#22059=ADVANCED_FACE('',(#3229),#2060,.F.);
#22060=ADVANCED_FACE('',(#3230),#2061,.F.);
#22061=ADVANCED_FACE('',(#3231),#2062,.T.);
#22062=ADVANCED_FACE('',(#3232),#2063,.F.);
#22063=ADVANCED_FACE('',(#3233),#2064,.F.);
#22064=ADVANCED_FACE('',(#3234),#2065,.F.);
#22065=ADVANCED_FACE('',(#3235),#2066,.F.);
#22066=ADVANCED_FACE('',(#3236),#2067,.F.);
#22067=ADVANCED_FACE('',(#3237),#2068,.F.);
#22068=ADVANCED_FACE('',(#3238),#2069,.F.);
#22069=ADVANCED_FACE('',(#3239),#2070,.F.);
#22070=ADVANCED_FACE('',(#3240),#389,.F.);
#22071=ADVANCED_FACE('',(#3241),#390,.F.);
#22072=ADVANCED_FACE('',(#3242),#2071,.F.);
#22073=ADVANCED_FACE('',(#3243),#2072,.F.);
#22074=ADVANCED_FACE('',(#3244),#2073,.F.);
#22075=ADVANCED_FACE('',(#3245),#2074,.F.);
#22076=ADVANCED_FACE('',(#3246),#2075,.F.);
#22077=ADVANCED_FACE('',(#3247),#2076,.T.);
#22078=ADVANCED_FACE('',(#3248),#391,.F.);
#22079=ADVANCED_FACE('',(#3249),#392,.F.);
#22080=ADVANCED_FACE('',(#3250),#393,.F.);
#22081=ADVANCED_FACE('',(#3251),#394,.F.);
#22082=ADVANCED_FACE('',(#3252),#395,.F.);
#22083=ADVANCED_FACE('',(#3253),#396,.F.);
#22084=ADVANCED_FACE('',(#3254),#397,.F.);
#22085=ADVANCED_FACE('',(#3255),#398,.F.);
#22086=ADVANCED_FACE('',(#3256),#399,.F.);
#22087=ADVANCED_FACE('',(#3257),#400,.F.);
#22088=ADVANCED_FACE('',(#3258),#401,.F.);
#22089=ADVANCED_FACE('',(#3259),#2077,.F.);
#22090=ADVANCED_FACE('',(#3260),#402,.F.);
#22091=ADVANCED_FACE('',(#3261),#403,.F.);
#22092=ADVANCED_FACE('',(#3262),#404,.F.);
#22093=ADVANCED_FACE('',(#3263),#405,.F.);
#22094=ADVANCED_FACE('',(#3264),#406,.F.);
#22095=ADVANCED_FACE('',(#3265),#407,.F.);
#22096=ADVANCED_FACE('',(#3266),#408,.F.);
#22097=ADVANCED_FACE('',(#3267),#2078,.F.);
#22098=ADVANCED_FACE('',(#3268),#409,.F.);
#22099=ADVANCED_FACE('',(#3269),#410,.F.);
#22100=ADVANCED_FACE('',(#3270),#411,.F.);
#22101=ADVANCED_FACE('',(#3271),#412,.F.);
#22102=ADVANCED_FACE('',(#3272),#413,.F.);
#22103=ADVANCED_FACE('',(#3273),#414,.F.);
#22104=ADVANCED_FACE('',(#3274),#415,.F.);
#22105=ADVANCED_FACE('',(#3275),#2079,.F.);
#22106=ADVANCED_FACE('',(#3276),#416,.F.);
#22107=ADVANCED_FACE('',(#3277),#417,.F.);
#22108=ADVANCED_FACE('',(#3278),#2080,.T.);
#22109=ADVANCED_FACE('',(#3279),#2081,.F.);
#22110=ADVANCED_FACE('',(#3280),#2082,.F.);
#22111=ADVANCED_FACE('',(#3281),#2083,.F.);
#22112=ADVANCED_FACE('',(#3282),#2084,.F.);
#22113=ADVANCED_FACE('',(#3283),#2085,.F.);
#22114=ADVANCED_FACE('',(#3284),#418,.F.);
#22115=ADVANCED_FACE('',(#3285),#419,.F.);
#22116=ADVANCED_FACE('',(#3286),#2086,.F.);
#22117=ADVANCED_FACE('',(#3287),#2087,.F.);
#22118=ADVANCED_FACE('',(#3288),#2088,.F.);
#22119=ADVANCED_FACE('',(#3289),#2089,.F.);
#22120=ADVANCED_FACE('',(#3290),#2090,.F.);
#22121=ADVANCED_FACE('',(#3291),#2091,.F.);
#22122=ADVANCED_FACE('',(#3292),#2092,.F.);
#22123=ADVANCED_FACE('',(#3293),#2093,.F.);
#22124=ADVANCED_FACE('',(#3294),#2094,.F.);
#22125=ADVANCED_FACE('',(#3295),#2095,.F.);
#22126=ADVANCED_FACE('',(#3296),#2096,.F.);
#22127=ADVANCED_FACE('',(#3297,#1718),#2097,.T.);
#22128=ADVANCED_FACE('',(#3298),#420,.F.);
#22129=ADVANCED_FACE('',(#3299),#421,.F.);
#22130=ADVANCED_FACE('',(#3300),#422,.F.);
#22131=ADVANCED_FACE('',(#3301),#423,.F.);
#22132=ADVANCED_FACE('',(#3302),#424,.F.);
#22133=ADVANCED_FACE('',(#3303),#425,.F.);
#22134=ADVANCED_FACE('',(#3304),#426,.F.);
#22135=ADVANCED_FACE('',(#3305),#427,.F.);
#22136=ADVANCED_FACE('',(#3306),#428,.F.);
#22137=ADVANCED_FACE('',(#3307),#429,.F.);
#22138=ADVANCED_FACE('',(#3308),#430,.F.);
#22139=ADVANCED_FACE('',(#3309),#431,.F.);
#22140=ADVANCED_FACE('',(#3310),#432,.F.);
#22141=ADVANCED_FACE('',(#3311),#2098,.F.);
#22142=ADVANCED_FACE('',(#3312),#433,.F.);
#22143=ADVANCED_FACE('',(#3313),#434,.F.);
#22144=ADVANCED_FACE('',(#3314),#435,.F.);
#22145=ADVANCED_FACE('',(#3315),#436,.F.);
#22146=ADVANCED_FACE('',(#3316),#437,.F.);
#22147=ADVANCED_FACE('',(#3317),#438,.F.);
#22148=ADVANCED_FACE('',(#3318),#439,.F.);
#22149=ADVANCED_FACE('',(#3319),#440,.F.);
#22150=ADVANCED_FACE('',(#3320),#441,.F.);
#22151=ADVANCED_FACE('',(#3321),#442,.F.);
#22152=ADVANCED_FACE('',(#3322),#443,.F.);
#22153=ADVANCED_FACE('',(#3323),#444,.F.);
#22154=ADVANCED_FACE('',(#3324),#445,.F.);
#22155=ADVANCED_FACE('',(#3325),#446,.F.);
#22156=ADVANCED_FACE('',(#3326),#447,.F.);
#22157=ADVANCED_FACE('',(#3327),#448,.F.);
#22158=ADVANCED_FACE('',(#3328),#449,.F.);
#22159=ADVANCED_FACE('',(#3329),#450,.F.);
#22160=ADVANCED_FACE('',(#3330),#2099,.F.);
#22161=ADVANCED_FACE('',(#3331),#451,.F.);
#22162=ADVANCED_FACE('',(#3332),#452,.F.);
#22163=ADVANCED_FACE('',(#3333),#2100,.T.);
#22164=ADVANCED_FACE('',(#3334),#453,.F.);
#22165=ADVANCED_FACE('',(#3335),#454,.F.);
#22166=ADVANCED_FACE('',(#3336),#455,.F.);
#22167=ADVANCED_FACE('',(#3337),#456,.F.);
#22168=ADVANCED_FACE('',(#3338),#457,.F.);
#22169=ADVANCED_FACE('',(#3339),#458,.F.);
#22170=ADVANCED_FACE('',(#3340),#459,.F.);
#22171=ADVANCED_FACE('',(#3341),#460,.F.);
#22172=ADVANCED_FACE('',(#3342),#461,.F.);
#22173=ADVANCED_FACE('',(#3343),#462,.F.);
#22174=ADVANCED_FACE('',(#3344),#463,.F.);
#22175=ADVANCED_FACE('',(#3345),#2101,.F.);
#22176=ADVANCED_FACE('',(#3346),#464,.F.);
#22177=ADVANCED_FACE('',(#3347),#465,.F.);
#22178=ADVANCED_FACE('',(#3348),#466,.F.);
#22179=ADVANCED_FACE('',(#3349),#467,.F.);
#22180=ADVANCED_FACE('',(#3350),#468,.F.);
#22181=ADVANCED_FACE('',(#3351),#469,.F.);
#22182=ADVANCED_FACE('',(#3352),#470,.F.);
#22183=ADVANCED_FACE('',(#3353),#2102,.F.);
#22184=ADVANCED_FACE('',(#3354),#471,.F.);
#22185=ADVANCED_FACE('',(#3355),#472,.F.);
#22186=ADVANCED_FACE('',(#3356),#473,.F.);
#22187=ADVANCED_FACE('',(#3357),#474,.F.);
#22188=ADVANCED_FACE('',(#3358),#475,.F.);
#22189=ADVANCED_FACE('',(#3359),#476,.F.);
#22190=ADVANCED_FACE('',(#3360),#477,.F.);
#22191=ADVANCED_FACE('',(#3361),#2103,.F.);
#22192=ADVANCED_FACE('',(#3362),#478,.F.);
#22193=ADVANCED_FACE('',(#3363),#479,.F.);
#22194=ADVANCED_FACE('',(#3364),#2104,.T.);
#22195=ADVANCED_FACE('',(#3365),#480,.F.);
#22196=ADVANCED_FACE('',(#3366),#481,.F.);
#22197=ADVANCED_FACE('',(#3367),#482,.F.);
#22198=ADVANCED_FACE('',(#3368),#483,.F.);
#22199=ADVANCED_FACE('',(#3369),#484,.F.);
#22200=ADVANCED_FACE('',(#3370),#485,.F.);
#22201=ADVANCED_FACE('',(#3371),#486,.F.);
#22202=ADVANCED_FACE('',(#3372),#487,.F.);
#22203=ADVANCED_FACE('',(#3373),#2105,.F.);
#22204=ADVANCED_FACE('',(#3374),#488,.F.);
#22205=ADVANCED_FACE('',(#3375),#489,.F.);
#22206=ADVANCED_FACE('',(#3376),#490,.F.);
#22207=ADVANCED_FACE('',(#3377),#491,.F.);
#22208=ADVANCED_FACE('',(#3378),#492,.F.);
#22209=ADVANCED_FACE('',(#3379),#493,.F.);
#22210=ADVANCED_FACE('',(#3380),#494,.F.);
#22211=ADVANCED_FACE('',(#3381),#495,.F.);
#22212=ADVANCED_FACE('',(#3382),#496,.F.);
#22213=ADVANCED_FACE('',(#3383),#2106,.F.);
#22214=ADVANCED_FACE('',(#3384),#2107,.F.);
#22215=ADVANCED_FACE('',(#3385),#2108,.F.);
#22216=ADVANCED_FACE('',(#3386),#497,.F.);
#22217=ADVANCED_FACE('',(#3387),#2109,.T.);
#22218=ADVANCED_FACE('',(#3388),#2110,.F.);
#22219=ADVANCED_FACE('',(#3389),#498,.F.);
#22220=ADVANCED_FACE('',(#3390),#499,.F.);
#22221=ADVANCED_FACE('',(#3391),#500,.F.);
#22222=ADVANCED_FACE('',(#3392),#501,.F.);
#22223=ADVANCED_FACE('',(#3393),#502,.F.);
#22224=ADVANCED_FACE('',(#3394),#2111,.F.);
#22225=ADVANCED_FACE('',(#3395),#2112,.F.);
#22226=ADVANCED_FACE('',(#3396),#2113,.F.);
#22227=ADVANCED_FACE('',(#3397),#503,.F.);
#22228=ADVANCED_FACE('',(#3398),#504,.F.);
#22229=ADVANCED_FACE('',(#3399),#505,.F.);
#22230=ADVANCED_FACE('',(#3400),#506,.F.);
#22231=ADVANCED_FACE('',(#3401),#507,.F.);
#22232=ADVANCED_FACE('',(#3402),#508,.F.);
#22233=ADVANCED_FACE('',(#3403),#2114,.F.);
#22234=ADVANCED_FACE('',(#3404),#2115,.F.);
#22235=ADVANCED_FACE('',(#3405),#2116,.F.);
#22236=ADVANCED_FACE('',(#3406),#2117,.F.);
#22237=ADVANCED_FACE('',(#3407,#1719),#2118,.T.);
#22238=ADVANCED_FACE('',(#3408),#509,.F.);
#22239=ADVANCED_FACE('',(#3409),#510,.F.);
#22240=ADVANCED_FACE('',(#3410),#511,.F.);
#22241=ADVANCED_FACE('',(#3411),#512,.F.);
#22242=ADVANCED_FACE('',(#3412),#513,.F.);
#22243=ADVANCED_FACE('',(#3413),#514,.F.);
#22244=ADVANCED_FACE('',(#3414),#515,.F.);
#22245=ADVANCED_FACE('',(#3415),#516,.F.);
#22246=ADVANCED_FACE('',(#3416),#517,.F.);
#22247=ADVANCED_FACE('',(#3417),#518,.F.);
#22248=ADVANCED_FACE('',(#3418),#519,.F.);
#22249=ADVANCED_FACE('',(#3419),#520,.F.);
#22250=ADVANCED_FACE('',(#3420),#521,.F.);
#22251=ADVANCED_FACE('',(#3421),#522,.F.);
#22252=ADVANCED_FACE('',(#3422),#523,.F.);
#22253=ADVANCED_FACE('',(#3423),#524,.F.);
#22254=ADVANCED_FACE('',(#3424),#525,.F.);
#22255=ADVANCED_FACE('',(#3425),#526,.F.);
#22256=ADVANCED_FACE('',(#3426),#527,.F.);
#22257=ADVANCED_FACE('',(#3427),#528,.F.);
#22258=ADVANCED_FACE('',(#3428),#529,.F.);
#22259=ADVANCED_FACE('',(#3429),#530,.F.);
#22260=ADVANCED_FACE('',(#3430),#531,.F.);
#22261=ADVANCED_FACE('',(#3431),#532,.F.);
#22262=ADVANCED_FACE('',(#3432),#533,.F.);
#22263=ADVANCED_FACE('',(#3433),#2119,.F.);
#22264=ADVANCED_FACE('',(#3434),#534,.F.);
#22265=ADVANCED_FACE('',(#3435),#535,.F.);
#22266=ADVANCED_FACE('',(#3436,#1720),#2120,.T.);
#22267=ADVANCED_FACE('',(#3437),#536,.F.);
#22268=ADVANCED_FACE('',(#3438),#537,.F.);
#22269=ADVANCED_FACE('',(#3439),#538,.F.);
#22270=ADVANCED_FACE('',(#3440),#539,.F.);
#22271=ADVANCED_FACE('',(#3441),#540,.F.);
#22272=ADVANCED_FACE('',(#3442),#541,.F.);
#22273=ADVANCED_FACE('',(#3443),#542,.F.);
#22274=ADVANCED_FACE('',(#3444),#543,.F.);
#22275=ADVANCED_FACE('',(#3445),#544,.F.);
#22276=ADVANCED_FACE('',(#3446),#545,.F.);
#22277=ADVANCED_FACE('',(#3447),#546,.F.);
#22278=ADVANCED_FACE('',(#3448),#547,.F.);
#22279=ADVANCED_FACE('',(#3449),#548,.F.);
#22280=ADVANCED_FACE('',(#3450),#549,.F.);
#22281=ADVANCED_FACE('',(#3451),#550,.F.);
#22282=ADVANCED_FACE('',(#3452),#2121,.F.);
#22283=ADVANCED_FACE('',(#3453),#2122,.F.);
#22284=ADVANCED_FACE('',(#3454),#2123,.F.);
#22285=ADVANCED_FACE('',(#3455),#2124,.F.);
#22286=ADVANCED_FACE('',(#3456),#2125,.F.);
#22287=ADVANCED_FACE('',(#3457),#551,.F.);
#22288=ADVANCED_FACE('',(#3458,#1721),#2126,.T.);
#22289=ADVANCED_FACE('',(#3459),#552,.F.);
#22290=ADVANCED_FACE('',(#3460),#553,.F.);
#22291=ADVANCED_FACE('',(#3461),#554,.F.);
#22292=ADVANCED_FACE('',(#3462),#555,.F.);
#22293=ADVANCED_FACE('',(#3463),#2127,.F.);
#22294=ADVANCED_FACE('',(#3464),#556,.F.);
#22295=ADVANCED_FACE('',(#3465),#557,.F.);
#22296=ADVANCED_FACE('',(#3466),#558,.F.);
#22297=ADVANCED_FACE('',(#3467),#2128,.F.);
#22298=ADVANCED_FACE('',(#3468),#2129,.F.);
#22299=ADVANCED_FACE('',(#3469),#2130,.F.);
#22300=ADVANCED_FACE('',(#3470),#2131,.F.);
#22301=ADVANCED_FACE('',(#3471),#2132,.F.);
#22302=ADVANCED_FACE('',(#3472),#2133,.T.);
#22303=ADVANCED_FACE('',(#3473),#2134,.T.);
#22304=ADVANCED_FACE('',(#3474),#2135,.T.);
#22305=ADVANCED_FACE('',(#3475),#2136,.T.);
#22306=ADVANCED_FACE('',(#3476),#2137,.T.);
#22307=ADVANCED_FACE('',(#3477),#2138,.T.);
#22308=ADVANCED_FACE('',(#3478),#2139,.T.);
#22309=ADVANCED_FACE('',(#3479),#2553,.F.);
#22310=ADVANCED_FACE('',(#3480),#21403,.F.);
#22311=ADVANCED_FACE('',(#3481),#2554,.F.);
#22312=ADVANCED_FACE('',(#3482,#1722),#2140,.T.);
#22313=ADVANCED_FACE('',(#3483),#21404,.F.);
#22314=ADVANCED_FACE('',(#3484),#2555,.F.);
#22315=ADVANCED_FACE('',(#3485,#1723),#2141,.F.);
#22316=ADVANCED_FACE('',(#3486),#2142,.F.);
#22317=ADVANCED_FACE('',(#3487),#2556,.T.);
#22318=ADVANCED_FACE('',(#3488),#312,.T.);
#22319=ADVANCED_FACE('',(#3489),#21405,.F.);
#22320=ADVANCED_FACE('',(#3490,#1724,#1725,#1726,#1727,#1728,#1729,#1730,
#1731),#2143,.T.);
#22321=ADVANCED_FACE('',(#3491),#2557,.F.);
#22322=ADVANCED_FACE('',(#3492),#21406,.F.);
#22323=ADVANCED_FACE('',(#3493),#2558,.F.);
#22324=ADVANCED_FACE('',(#3494),#21407,.F.);
#22325=ADVANCED_FACE('',(#3495),#2559,.F.);
#22326=ADVANCED_FACE('',(#3496),#21408,.F.);
#22327=ADVANCED_FACE('',(#3497),#2560,.F.);
#22328=ADVANCED_FACE('',(#3498),#21409,.F.);
#22329=ADVANCED_FACE('',(#3499),#2561,.F.);
#22330=ADVANCED_FACE('',(#3500),#21410,.F.);
#22331=ADVANCED_FACE('',(#3501),#2562,.F.);
#22332=ADVANCED_FACE('',(#3502),#21411,.F.);
#22333=ADVANCED_FACE('',(#3503),#21412,.F.);
#22334=ADVANCED_FACE('',(#3504),#21413,.F.);
#22335=ADVANCED_FACE('',(#3505),#21414,.F.);
#22336=ADVANCED_FACE('',(#3506),#21415,.F.);
#22337=ADVANCED_FACE('',(#3507),#21416,.F.);
#22338=ADVANCED_FACE('',(#3508),#21417,.F.);
#22339=ADVANCED_FACE('',(#3509),#2563,.F.);
#22340=ADVANCED_FACE('',(#3510,#1732,#1733,#1734,#1735,#1736,#1737,#1738,
#1739,#1740,#1741,#1742,#1743,#1744,#1745),#2144,.T.);
#22341=ADVANCED_FACE('',(#3511),#21418,.T.);
#22342=ADVANCED_FACE('',(#3512),#2145,.T.);
#22343=ADVANCED_FACE('',(#3513),#2564,.F.);
#22344=ADVANCED_FACE('',(#3514,#1746),#2146,.T.);
#22345=ADVANCED_FACE('',(#3515,#1747),#2147,.F.);
#22346=ADVANCED_FACE('',(#3516),#2565,.T.);
#22347=ADVANCED_FACE('',(#3517,#1748),#2148,.F.);
#22348=ADVANCED_FACE('',(#3518),#2566,.T.);
#22349=ADVANCED_FACE('',(#3519,#1749),#2149,.F.);
#22350=ADVANCED_FACE('',(#3520),#2567,.T.);
#22351=ADVANCED_FACE('',(#3521,#1750),#2150,.F.);
#22352=ADVANCED_FACE('',(#3522),#2568,.T.);
#22353=ADVANCED_FACE('',(#3523),#2569,.T.);
#22354=ADVANCED_FACE('',(#3524),#21419,.T.);
#22355=ADVANCED_FACE('',(#3525),#21420,.T.);
#22356=ADVANCED_FACE('',(#3526),#2570,.T.);
#22357=ADVANCED_FACE('',(#3527),#21421,.T.);
#22358=ADVANCED_FACE('',(#3528,#1751),#2151,.T.);
#22359=ADVANCED_FACE('',(#3529),#2571,.F.);
#22360=ADVANCED_FACE('',(#3530),#21422,.F.);
#22361=ADVANCED_FACE('',(#3531),#2572,.F.);
#22362=ADVANCED_FACE('',(#3532),#1597,.T.);
#22363=ADVANCED_FACE('',(#3533),#2573,.T.);
#22364=ADVANCED_FACE('',(#3534),#2574,.F.);
#22365=ADVANCED_FACE('',(#3535,#1752),#2152,.F.);
#22366=ADVANCED_FACE('',(#3536,#1753),#2153,.T.);
#22367=ADVANCED_FACE('',(#3537),#1598,.F.);
#22368=ADVANCED_FACE('',(#3538),#2575,.F.);
#22369=ADVANCED_FACE('',(#3539,#1754),#2154,.T.);
#22370=ADVANCED_FACE('',(#3540),#2576,.F.);
#22371=ADVANCED_FACE('',(#3541,#1755),#2155,.T.);
#22372=ADVANCED_FACE('',(#3542),#21423,.T.);
#22373=ADVANCED_FACE('',(#3543),#2577,.T.);
#22374=ADVANCED_FACE('',(#3544),#21424,.T.);
#22375=ADVANCED_FACE('',(#3545,#1756),#2156,.T.);
#22376=ADVANCED_FACE('',(#3546),#2578,.T.);
#22377=ADVANCED_FACE('',(#3547),#21425,.T.);
#22378=ADVANCED_FACE('',(#3548,#1757),#2157,.T.);
#22379=ADVANCED_FACE('',(#3549,#1758,#1759,#1760,#1761,#1762,#1763,#1764,
#1765,#1766,#1767,#1768,#1769,#1770,#1771,#1772,#1773,#1774),#21426,.F.);
#22380=ADVANCED_FACE('',(#3550,#1775,#1776,#1777,#1778,#1779,#1780,#1781,
#1782,#1783,#1784,#1785,#1786,#1787,#1788,#1789,#1790,#1791),#21427,.T.);
#22381=ADVANCED_FACE('',(#3551),#21428,.T.);
#22382=ADVANCED_FACE('',(#3552),#21429,.F.);
#22383=ADVANCED_FACE('',(#3553),#2158,.T.);
#22384=ADVANCED_FACE('',(#3554),#2159,.T.);
#22385=ADVANCED_FACE('',(#3555),#21430,.T.);
#22386=ADVANCED_FACE('',(#3556),#21431,.T.);
#22387=ADVANCED_FACE('',(#3557),#2160,.T.);
#22388=ADVANCED_FACE('',(#3558),#2161,.T.);
#22389=ADVANCED_FACE('',(#3559),#2162,.T.);
#22390=ADVANCED_FACE('',(#3560),#21432,.T.);
#22391=ADVANCED_FACE('',(#3561),#21433,.T.);
#22392=ADVANCED_FACE('',(#3562),#2163,.T.);
#22393=ADVANCED_FACE('',(#3563),#2164,.T.);
#22394=ADVANCED_FACE('',(#3564),#2165,.T.);
#22395=ADVANCED_FACE('',(#3565),#21434,.T.);
#22396=ADVANCED_FACE('',(#3566),#21435,.T.);
#22397=ADVANCED_FACE('',(#3567),#2166,.T.);
#22398=ADVANCED_FACE('',(#3568),#2167,.T.);
#22399=ADVANCED_FACE('',(#3569),#2168,.T.);
#22400=ADVANCED_FACE('',(#3570),#21436,.T.);
#22401=ADVANCED_FACE('',(#3571),#21437,.T.);
#22402=ADVANCED_FACE('',(#3572),#2169,.T.);
#22403=ADVANCED_FACE('',(#3573),#2170,.T.);
#22404=ADVANCED_FACE('',(#3574),#2171,.T.);
#22405=ADVANCED_FACE('',(#3575),#21438,.T.);
#22406=ADVANCED_FACE('',(#3576),#21439,.T.);
#22407=ADVANCED_FACE('',(#3577),#2172,.T.);
#22408=ADVANCED_FACE('',(#3578),#2173,.T.);
#22409=ADVANCED_FACE('',(#3579),#2174,.T.);
#22410=ADVANCED_FACE('',(#3580),#21440,.T.);
#22411=ADVANCED_FACE('',(#3581),#21441,.T.);
#22412=ADVANCED_FACE('',(#3582),#2175,.T.);
#22413=ADVANCED_FACE('',(#3583),#2176,.T.);
#22414=ADVANCED_FACE('',(#3584),#2177,.T.);
#22415=ADVANCED_FACE('',(#3585),#21442,.T.);
#22416=ADVANCED_FACE('',(#3586),#21443,.T.);
#22417=ADVANCED_FACE('',(#3587),#2178,.T.);
#22418=ADVANCED_FACE('',(#3588),#2179,.T.);
#22419=ADVANCED_FACE('',(#3589),#2180,.T.);
#22420=ADVANCED_FACE('',(#3590),#21444,.T.);
#22421=ADVANCED_FACE('',(#3591),#21445,.T.);
#22422=ADVANCED_FACE('',(#3592),#2181,.T.);
#22423=ADVANCED_FACE('',(#3593),#2182,.T.);
#22424=ADVANCED_FACE('',(#3594),#2183,.T.);
#22425=ADVANCED_FACE('',(#3595),#21446,.T.);
#22426=ADVANCED_FACE('',(#3596),#21447,.T.);
#22427=ADVANCED_FACE('',(#3597),#2184,.T.);
#22428=ADVANCED_FACE('',(#3598),#2185,.T.);
#22429=ADVANCED_FACE('',(#3599),#2186,.T.);
#22430=ADVANCED_FACE('',(#3600),#21448,.T.);
#22431=ADVANCED_FACE('',(#3601),#21449,.T.);
#22432=ADVANCED_FACE('',(#3602),#2187,.T.);
#22433=ADVANCED_FACE('',(#3603),#2188,.T.);
#22434=ADVANCED_FACE('',(#3604),#2189,.T.);
#22435=ADVANCED_FACE('',(#3605),#21450,.T.);
#22436=ADVANCED_FACE('',(#3606),#21451,.T.);
#22437=ADVANCED_FACE('',(#3607),#2190,.T.);
#22438=ADVANCED_FACE('',(#3608),#2191,.T.);
#22439=ADVANCED_FACE('',(#3609),#2192,.T.);
#22440=ADVANCED_FACE('',(#3610),#21452,.T.);
#22441=ADVANCED_FACE('',(#3611),#21453,.T.);
#22442=ADVANCED_FACE('',(#3612),#2193,.T.);
#22443=ADVANCED_FACE('',(#3613),#2194,.T.);
#22444=ADVANCED_FACE('',(#3614),#2195,.T.);
#22445=ADVANCED_FACE('',(#3615),#21454,.T.);
#22446=ADVANCED_FACE('',(#3616),#21455,.T.);
#22447=ADVANCED_FACE('',(#3617),#2196,.T.);
#22448=ADVANCED_FACE('',(#3618),#2197,.T.);
#22449=ADVANCED_FACE('',(#3619),#2198,.T.);
#22450=ADVANCED_FACE('',(#3620),#21456,.T.);
#22451=ADVANCED_FACE('',(#3621),#21457,.T.);
#22452=ADVANCED_FACE('',(#3622),#2199,.T.);
#22453=ADVANCED_FACE('',(#3623),#2200,.T.);
#22454=ADVANCED_FACE('',(#3624),#2201,.T.);
#22455=ADVANCED_FACE('',(#3625),#21458,.T.);
#22456=ADVANCED_FACE('',(#3626),#21459,.T.);
#22457=ADVANCED_FACE('',(#3627),#2202,.T.);
#22458=ADVANCED_FACE('',(#3628),#2203,.T.);
#22459=ADVANCED_FACE('',(#3629),#2204,.T.);
#22460=ADVANCED_FACE('',(#3630),#21460,.T.);
#22461=ADVANCED_FACE('',(#3631),#21461,.T.);
#22462=ADVANCED_FACE('',(#3632),#2205,.T.);
#22463=ADVANCED_FACE('',(#3633),#2206,.T.);
#22464=ADVANCED_FACE('',(#3634),#2207,.T.);
#22465=ADVANCED_FACE('',(#3635),#2208,.T.);
#22466=ADVANCED_FACE('',(#3636),#21462,.T.);
#22467=ADVANCED_FACE('',(#3637),#21463,.T.);
#22468=ADVANCED_FACE('',(#3638),#2209,.T.);
#22469=ADVANCED_FACE('',(#3639),#21464,.T.);
#22470=ADVANCED_FACE('',(#3640),#21465,.T.);
#22471=ADVANCED_FACE('',(#3641),#2210,.T.);
#22472=ADVANCED_FACE('',(#3642),#21466,.T.);
#22473=ADVANCED_FACE('',(#3643),#2211,.T.);
#22474=ADVANCED_FACE('',(#3644),#21467,.T.);
#22475=ADVANCED_FACE('',(#3645),#2212,.T.);
#22476=ADVANCED_FACE('',(#3646),#21468,.T.);
#22477=ADVANCED_FACE('',(#3647),#2213,.T.);
#22478=ADVANCED_FACE('',(#3648),#21469,.T.);
#22479=ADVANCED_FACE('',(#3649),#2214,.T.);
#22480=ADVANCED_FACE('',(#3650),#21470,.T.);
#22481=ADVANCED_FACE('',(#3651),#2215,.T.);
#22482=ADVANCED_FACE('',(#3652),#21471,.T.);
#22483=ADVANCED_FACE('',(#3653),#2216,.T.);
#22484=ADVANCED_FACE('',(#3654),#21472,.T.);
#22485=ADVANCED_FACE('',(#3655),#2217,.T.);
#22486=ADVANCED_FACE('',(#3656),#21473,.T.);
#22487=ADVANCED_FACE('',(#3657),#2218,.T.);
#22488=ADVANCED_FACE('',(#3658),#21474,.T.);
#22489=ADVANCED_FACE('',(#3659),#2219,.T.);
#22490=ADVANCED_FACE('',(#3660),#21475,.T.);
#22491=ADVANCED_FACE('',(#3661),#2220,.T.);
#22492=ADVANCED_FACE('',(#3662),#21476,.T.);
#22493=ADVANCED_FACE('',(#3663),#2221,.T.);
#22494=ADVANCED_FACE('',(#3664),#21477,.T.);
#22495=ADVANCED_FACE('',(#3665),#2222,.T.);
#22496=ADVANCED_FACE('',(#3666),#21478,.T.);
#22497=ADVANCED_FACE('',(#3667),#2223,.T.);
#22498=ADVANCED_FACE('',(#3668),#21479,.T.);
#22499=ADVANCED_FACE('',(#3669),#2224,.T.);
#22500=ADVANCED_FACE('',(#3670),#21480,.T.);
#22501=ADVANCED_FACE('',(#3671),#21481,.T.);
#22502=ADVANCED_FACE('',(#3672),#2225,.T.);
#22503=ADVANCED_FACE('',(#3673),#21482,.F.);
#22504=ADVANCED_FACE('',(#3674,#1792),#2226,.T.);
#22505=ADVANCED_FACE('',(#3675),#21483,.T.);
#22506=ADVANCED_FACE('',(#3676),#2579,.T.);
#22507=ADVANCED_FACE('',(#3677,#1793),#2227,.T.);
#22508=ADVANCED_FACE('',(#3678,#1794),#2228,.T.);
#22509=ADVANCED_FACE('',(#3679),#2580,.T.);
#22510=ADVANCED_FACE('',(#3680,#1795),#2229,.T.);
#22511=ADVANCED_FACE('',(#3681),#21484,.F.);
#22512=ADVANCED_FACE('',(#3682),#2581,.F.);
#22513=ADVANCED_FACE('',(#3683),#21485,.F.);
#22514=ADVANCED_FACE('',(#3684,#1796),#2230,.T.);
#22515=ADVANCED_FACE('',(#3685),#21486,.T.);
#22516=ADVANCED_FACE('',(#3686),#2582,.T.);
#22517=ADVANCED_FACE('',(#3687),#21487,.T.);
#22518=ADVANCED_FACE('',(#3688,#1797),#2231,.T.);
#22519=ADVANCED_FACE('',(#3689),#21488,.F.);
#22520=ADVANCED_FACE('',(#3690),#21489,.F.);
#22521=ADVANCED_FACE('',(#3691),#2583,.F.);
#22522=ADVANCED_FACE('',(#3692),#2584,.F.);
#22523=ADVANCED_FACE('',(#3693),#2232,.T.);
#22524=ADVANCED_FACE('',(#3694),#2585,.T.);
#22525=ADVANCED_FACE('',(#3695),#2233,.T.);
#22526=ADVANCED_FACE('',(#3696),#2586,.F.);
#22527=ADVANCED_FACE('',(#3697),#2234,.T.);
#22528=ADVANCED_FACE('',(#3698),#2587,.T.);
#22529=ADVANCED_FACE('',(#3699),#2235,.T.);
#22530=ADVANCED_FACE('',(#3700),#2588,.T.);
#22531=ADVANCED_FACE('',(#3701,#1798,#1799),#2236,.T.);
#22532=ADVANCED_FACE('',(#3702,#1800,#1801),#2237,.F.);
#22533=ADVANCED_FACE('',(#3703),#2589,.T.);
#22534=ADVANCED_FACE('',(#3704),#2590,.T.);
#22535=ADVANCED_FACE('',(#3705),#2591,.T.);
#22536=ADVANCED_FACE('',(#3706),#2592,.T.);
#22537=ADVANCED_FACE('',(#3707),#2593,.T.);
#22538=ADVANCED_FACE('',(#3708),#2594,.T.);
#22539=ADVANCED_FACE('',(#3709),#2595,.T.);
#22540=ADVANCED_FACE('',(#3710),#2596,.T.);
#22541=ADVANCED_FACE('',(#3711),#2597,.T.);
#22542=ADVANCED_FACE('',(#3712),#2598,.T.);
#22543=ADVANCED_FACE('',(#3713),#2599,.T.);
#22544=ADVANCED_FACE('',(#3714),#2600,.T.);
#22545=ADVANCED_FACE('',(#3715),#2601,.T.);
#22546=ADVANCED_FACE('',(#3716),#2602,.T.);
#22547=ADVANCED_FACE('',(#3717),#2603,.T.);
#22548=ADVANCED_FACE('',(#3718),#2604,.T.);
#22549=ADVANCED_FACE('',(#3719),#2605,.T.);
#22550=ADVANCED_FACE('',(#3720),#2606,.T.);
#22551=ADVANCED_FACE('',(#3721),#2607,.T.);
#22552=ADVANCED_FACE('',(#3722),#2608,.T.);
#22553=ADVANCED_FACE('',(#3723),#2609,.T.);
#22554=ADVANCED_FACE('',(#3724),#2610,.T.);
#22555=ADVANCED_FACE('',(#3725),#2611,.T.);
#22556=ADVANCED_FACE('',(#3726),#2612,.T.);
#22557=ADVANCED_FACE('',(#3727),#2613,.T.);
#22558=ADVANCED_FACE('',(#3728),#2614,.T.);
#22559=ADVANCED_FACE('',(#3729),#2615,.T.);
#22560=ADVANCED_FACE('',(#3730),#2616,.T.);
#22561=ADVANCED_FACE('',(#3731),#2617,.T.);
#22562=ADVANCED_FACE('',(#3732),#2618,.T.);
#22563=ADVANCED_FACE('',(#3733),#2619,.T.);
#22564=ADVANCED_FACE('',(#3734),#2620,.T.);
#22565=ADVANCED_FACE('',(#3735),#2621,.T.);
#22566=ADVANCED_FACE('',(#3736),#2622,.T.);
#22567=ADVANCED_FACE('',(#3737),#2623,.T.);
#22568=ADVANCED_FACE('',(#3738),#2624,.T.);
#22569=ADVANCED_FACE('',(#3739),#2625,.T.);
#22570=ADVANCED_FACE('',(#3740),#2626,.T.);
#22571=ADVANCED_FACE('',(#3741),#2627,.T.);
#22572=ADVANCED_FACE('',(#3742),#2628,.T.);
#22573=ADVANCED_FACE('',(#3743),#2629,.T.);
#22574=ADVANCED_FACE('',(#3744),#2630,.T.);
#22575=ADVANCED_FACE('',(#3745),#2631,.T.);
#22576=ADVANCED_FACE('',(#3746),#2632,.T.);
#22577=ADVANCED_FACE('',(#3747),#2633,.T.);
#22578=ADVANCED_FACE('',(#3748),#2238,.F.);
#22579=ADVANCED_FACE('',(#3749),#559,.F.);
#22580=ADVANCED_FACE('',(#3750),#2239,.T.);
#22581=ADVANCED_FACE('',(#3751),#2634,.T.);
#22582=ADVANCED_FACE('',(#3752),#560,.F.);
#22583=ADVANCED_FACE('',(#3753),#2635,.T.);
#22584=ADVANCED_FACE('',(#3754),#313,.F.);
#22585=ADVANCED_FACE('',(#3755,#1802),#2240,.T.);
#22586=ADVANCED_FACE('',(#3756),#21490,.F.);
#22587=ADVANCED_FACE('',(#3757),#2241,.F.);
#22588=ADVANCED_FACE('',(#3758),#2242,.F.);
#22589=ADVANCED_FACE('',(#3759),#2243,.F.);
#22590=ADVANCED_FACE('',(#3760),#2244,.F.);
#22591=ADVANCED_FACE('',(#3761),#2245,.F.);
#22592=ADVANCED_FACE('',(#3762),#2246,.F.);
#22593=ADVANCED_FACE('',(#3763,#1803),#2247,.F.);
#22594=ADVANCED_FACE('',(#3764),#2248,.F.);
#22595=ADVANCED_FACE('',(#3765),#2249,.F.);
#22596=ADVANCED_FACE('',(#3766),#2250,.F.);
#22597=ADVANCED_FACE('',(#3767),#2251,.F.);
#22598=ADVANCED_FACE('',(#3768),#2252,.F.);
#22599=ADVANCED_FACE('',(#3769),#2253,.F.);
#22600=ADVANCED_FACE('',(#3770),#2254,.F.);
#22601=ADVANCED_FACE('',(#3771),#2255,.F.);
#22602=ADVANCED_FACE('',(#3772),#2256,.F.);
#22603=ADVANCED_FACE('',(#3773),#2257,.F.);
#22604=ADVANCED_FACE('',(#3774),#2258,.F.);
#22605=ADVANCED_FACE('',(#3775),#2259,.F.);
#22606=ADVANCED_FACE('',(#3776),#2260,.F.);
#22607=ADVANCED_FACE('',(#3777),#2261,.F.);
#22608=ADVANCED_FACE('',(#3778),#2262,.F.);
#22609=ADVANCED_FACE('',(#3779),#2263,.F.);
#22610=ADVANCED_FACE('',(#3780),#2264,.F.);
#22611=ADVANCED_FACE('',(#3781),#2265,.F.);
#22612=ADVANCED_FACE('',(#3782),#2266,.F.);
#22613=ADVANCED_FACE('',(#3783),#2267,.F.);
#22614=ADVANCED_FACE('',(#3784),#2268,.F.);
#22615=ADVANCED_FACE('',(#3785),#2269,.F.);
#22616=ADVANCED_FACE('',(#3786),#2270,.F.);
#22617=ADVANCED_FACE('',(#3787),#2271,.F.);
#22618=ADVANCED_FACE('',(#3788),#2272,.F.);
#22619=ADVANCED_FACE('',(#3789),#2273,.F.);
#22620=ADVANCED_FACE('',(#3790),#2274,.F.);
#22621=ADVANCED_FACE('',(#3791),#2275,.F.);
#22622=ADVANCED_FACE('',(#3792),#2276,.F.);
#22623=ADVANCED_FACE('',(#3793),#2277,.F.);
#22624=ADVANCED_FACE('',(#3794),#2278,.F.);
#22625=ADVANCED_FACE('',(#3795),#2279,.F.);
#22626=ADVANCED_FACE('',(#3796),#2280,.F.);
#22627=ADVANCED_FACE('',(#3797),#2281,.F.);
#22628=ADVANCED_FACE('',(#3798),#2282,.F.);
#22629=ADVANCED_FACE('',(#3799),#2283,.F.);
#22630=ADVANCED_FACE('',(#3800),#2284,.F.);
#22631=ADVANCED_FACE('',(#3801),#2285,.F.);
#22632=ADVANCED_FACE('',(#3802),#2286,.F.);
#22633=ADVANCED_FACE('',(#3803),#2287,.F.);
#22634=ADVANCED_FACE('',(#3804),#2288,.F.);
#22635=ADVANCED_FACE('',(#3805),#2289,.F.);
#22636=ADVANCED_FACE('',(#3806),#2290,.F.);
#22637=ADVANCED_FACE('',(#3807),#2291,.F.);
#22638=ADVANCED_FACE('',(#3808),#2292,.F.);
#22639=ADVANCED_FACE('',(#3809),#2293,.F.);
#22640=ADVANCED_FACE('',(#3810),#2294,.F.);
#22641=ADVANCED_FACE('',(#3811),#2295,.F.);
#22642=ADVANCED_FACE('',(#3812),#2296,.F.);
#22643=ADVANCED_FACE('',(#3813),#2297,.F.);
#22644=ADVANCED_FACE('',(#3814),#2298,.F.);
#22645=ADVANCED_FACE('',(#3815),#2299,.F.);
#22646=ADVANCED_FACE('',(#3816),#2300,.F.);
#22647=ADVANCED_FACE('',(#3817),#2301,.F.);
#22648=ADVANCED_FACE('',(#3818),#2302,.F.);
#22649=ADVANCED_FACE('',(#3819),#2303,.F.);
#22650=ADVANCED_FACE('',(#3820),#2304,.F.);
#22651=ADVANCED_FACE('',(#3821),#2305,.F.);
#22652=ADVANCED_FACE('',(#3822),#2306,.F.);
#22653=ADVANCED_FACE('',(#3823),#2307,.F.);
#22654=ADVANCED_FACE('',(#3824),#2308,.F.);
#22655=ADVANCED_FACE('',(#3825),#2309,.F.);
#22656=ADVANCED_FACE('',(#3826),#2310,.F.);
#22657=ADVANCED_FACE('',(#3827),#2311,.F.);
#22658=ADVANCED_FACE('',(#3828),#2312,.F.);
#22659=ADVANCED_FACE('',(#3829),#2313,.F.);
#22660=ADVANCED_FACE('',(#3830),#2314,.F.);
#22661=ADVANCED_FACE('',(#3831),#2315,.F.);
#22662=ADVANCED_FACE('',(#3832),#2316,.F.);
#22663=ADVANCED_FACE('',(#3833),#2317,.F.);
#22664=ADVANCED_FACE('',(#3834),#2318,.F.);
#22665=ADVANCED_FACE('',(#3835),#2319,.F.);
#22666=ADVANCED_FACE('',(#3836),#2320,.F.);
#22667=ADVANCED_FACE('',(#3837),#2321,.F.);
#22668=ADVANCED_FACE('',(#3838),#2322,.F.);
#22669=ADVANCED_FACE('',(#3839),#2323,.F.);
#22670=ADVANCED_FACE('',(#3840),#2324,.F.);
#22671=ADVANCED_FACE('',(#3841),#2325,.F.);
#22672=ADVANCED_FACE('',(#3842),#2326,.F.);
#22673=ADVANCED_FACE('',(#3843),#2327,.F.);
#22674=ADVANCED_FACE('',(#3844),#2328,.F.);
#22675=ADVANCED_FACE('',(#3845),#2329,.F.);
#22676=ADVANCED_FACE('',(#3846),#2330,.F.);
#22677=ADVANCED_FACE('',(#3847),#2331,.F.);
#22678=ADVANCED_FACE('',(#3848),#2332,.F.);
#22679=ADVANCED_FACE('',(#3849),#2333,.F.);
#22680=ADVANCED_FACE('',(#3850),#2334,.F.);
#22681=ADVANCED_FACE('',(#3851),#2335,.F.);
#22682=ADVANCED_FACE('',(#3852),#2336,.F.);
#22683=ADVANCED_FACE('',(#3853),#2337,.F.);
#22684=ADVANCED_FACE('',(#3854),#2338,.F.);
#22685=ADVANCED_FACE('',(#3855),#2339,.F.);
#22686=ADVANCED_FACE('',(#3856),#2340,.F.);
#22687=ADVANCED_FACE('',(#3857),#2341,.F.);
#22688=ADVANCED_FACE('',(#3858),#2342,.F.);
#22689=ADVANCED_FACE('',(#3859),#2343,.F.);
#22690=ADVANCED_FACE('',(#3860),#2344,.F.);
#22691=ADVANCED_FACE('',(#3861),#2345,.F.);
#22692=ADVANCED_FACE('',(#3862),#2346,.F.);
#22693=ADVANCED_FACE('',(#3863),#2347,.F.);
#22694=ADVANCED_FACE('',(#3864),#2348,.F.);
#22695=ADVANCED_FACE('',(#3865),#2349,.F.);
#22696=ADVANCED_FACE('',(#3866),#2350,.F.);
#22697=ADVANCED_FACE('',(#3867),#2351,.F.);
#22698=ADVANCED_FACE('',(#3868),#2352,.F.);
#22699=ADVANCED_FACE('',(#3869),#2353,.F.);
#22700=ADVANCED_FACE('',(#3870),#2354,.F.);
#22701=ADVANCED_FACE('',(#3871),#2355,.F.);
#22702=ADVANCED_FACE('',(#3872),#2356,.F.);
#22703=ADVANCED_FACE('',(#3873),#2357,.F.);
#22704=ADVANCED_FACE('',(#3874),#2358,.F.);
#22705=ADVANCED_FACE('',(#3875),#2359,.F.);
#22706=ADVANCED_FACE('',(#3876),#2360,.F.);
#22707=ADVANCED_FACE('',(#3877),#2361,.F.);
#22708=ADVANCED_FACE('',(#3878),#2362,.F.);
#22709=ADVANCED_FACE('',(#3879),#2363,.F.);
#22710=ADVANCED_FACE('',(#3880),#2364,.F.);
#22711=ADVANCED_FACE('',(#3881),#2365,.F.);
#22712=ADVANCED_FACE('',(#3882),#2366,.F.);
#22713=ADVANCED_FACE('',(#3883),#2367,.F.);
#22714=ADVANCED_FACE('',(#3884),#2368,.F.);
#22715=ADVANCED_FACE('',(#3885),#2369,.F.);
#22716=ADVANCED_FACE('',(#3886),#2370,.F.);
#22717=ADVANCED_FACE('',(#3887),#2371,.F.);
#22718=ADVANCED_FACE('',(#3888),#2372,.F.);
#22719=ADVANCED_FACE('',(#3889),#2373,.F.);
#22720=ADVANCED_FACE('',(#3890),#2374,.F.);
#22721=ADVANCED_FACE('',(#3891),#2375,.F.);
#22722=ADVANCED_FACE('',(#3892),#2376,.F.);
#22723=ADVANCED_FACE('',(#3893),#2377,.F.);
#22724=ADVANCED_FACE('',(#3894),#2378,.F.);
#22725=ADVANCED_FACE('',(#3895),#2379,.F.);
#22726=ADVANCED_FACE('',(#3896),#2380,.F.);
#22727=ADVANCED_FACE('',(#3897),#2381,.F.);
#22728=ADVANCED_FACE('',(#3898),#2382,.F.);
#22729=ADVANCED_FACE('',(#3899),#2383,.F.);
#22730=ADVANCED_FACE('',(#3900),#2384,.F.);
#22731=ADVANCED_FACE('',(#3901),#2385,.F.);
#22732=ADVANCED_FACE('',(#3902),#2386,.F.);
#22733=ADVANCED_FACE('',(#3903),#2387,.F.);
#22734=ADVANCED_FACE('',(#3904),#2388,.F.);
#22735=ADVANCED_FACE('',(#3905),#2389,.F.);
#22736=ADVANCED_FACE('',(#3906),#2390,.F.);
#22737=ADVANCED_FACE('',(#3907),#2391,.F.);
#22738=ADVANCED_FACE('',(#3908),#2392,.T.);
#22739=ADVANCED_FACE('',(#3909),#21491,.T.);
#22740=ADVANCED_FACE('',(#3910),#21492,.T.);
#22741=ADVANCED_FACE('',(#3911),#2636,.T.);
#22742=ADVANCED_FACE('',(#3912),#21493,.T.);
#22743=ADVANCED_FACE('',(#3913,#1804),#2393,.T.);
#22744=ADVANCED_FACE('',(#3914),#2637,.T.);
#22745=ADVANCED_FACE('',(#3915),#2638,.T.);
#22746=ADVANCED_FACE('',(#3916),#2639,.T.);
#22747=ADVANCED_FACE('',(#3917),#2640,.T.);
#22748=ADVANCED_FACE('',(#3918),#2641,.T.);
#22749=ADVANCED_FACE('',(#3919),#2642,.T.);
#22750=ADVANCED_FACE('',(#3920),#2643,.T.);
#22751=ADVANCED_FACE('',(#3921),#2644,.T.);
#22752=ADVANCED_FACE('',(#3922),#2645,.T.);
#22753=ADVANCED_FACE('',(#3923),#2646,.T.);
#22754=ADVANCED_FACE('',(#3924),#2647,.T.);
#22755=ADVANCED_FACE('',(#3925),#2648,.T.);
#22756=ADVANCED_FACE('',(#3926),#2649,.T.);
#22757=ADVANCED_FACE('',(#3927),#2650,.T.);
#22758=ADVANCED_FACE('',(#3928),#2651,.T.);
#22759=ADVANCED_FACE('',(#3929),#2652,.T.);
#22760=ADVANCED_FACE('',(#3930),#2653,.T.);
#22761=ADVANCED_FACE('',(#3931),#2654,.T.);
#22762=ADVANCED_FACE('',(#3932),#2655,.T.);
#22763=ADVANCED_FACE('',(#3933),#2656,.T.);
#22764=ADVANCED_FACE('',(#3934),#2657,.T.);
#22765=ADVANCED_FACE('',(#3935),#2658,.T.);
#22766=ADVANCED_FACE('',(#3936),#2659,.T.);
#22767=ADVANCED_FACE('',(#3937),#2660,.T.);
#22768=ADVANCED_FACE('',(#3938),#2661,.T.);
#22769=ADVANCED_FACE('',(#3939),#2662,.T.);
#22770=ADVANCED_FACE('',(#3940),#2394,.F.);
#22771=ADVANCED_FACE('',(#3941),#561,.F.);
#22772=ADVANCED_FACE('',(#3942),#2663,.T.);
#22773=ADVANCED_FACE('',(#3943),#562,.F.);
#22774=ADVANCED_FACE('',(#3944),#2664,.T.);
#22775=ADVANCED_FACE('',(#3945),#563,.T.);
#22776=ADVANCED_FACE('',(#3946),#564,.F.);
#22777=ADVANCED_FACE('',(#3947),#565,.F.);
#22778=ADVANCED_FACE('',(#3948),#2395,.T.);
#22779=ADVANCED_FACE('',(#3949),#2665,.T.);
#22780=ADVANCED_FACE('',(#3950),#566,.F.);
#22781=ADVANCED_FACE('',(#3951),#567,.F.);
#22782=ADVANCED_FACE('',(#3952),#568,.T.);
#22783=ADVANCED_FACE('',(#3953),#21494,.T.);
#22784=ADVANCED_FACE('',(#3954),#2396,.T.);
#22785=ADVANCED_FACE('',(#3955),#2397,.T.);
#22786=ADVANCED_FACE('',(#3956),#2398,.T.);
#22787=ADVANCED_FACE('',(#3957),#21495,.T.);
#22788=ADVANCED_FACE('',(#3958),#2399,.T.);
#22789=ADVANCED_FACE('',(#3959,#1805),#2400,.T.);
#22790=ADVANCED_FACE('',(#3960),#2401,.T.);
#22791=ADVANCED_FACE('',(#3961,#1806),#2402,.F.);
#22792=ADVANCED_FACE('',(#3962),#2403,.F.);
#22793=ADVANCED_FACE('',(#3963),#2404,.T.);
#22794=ADVANCED_FACE('',(#3964),#2405,.T.);
#22795=ADVANCED_FACE('',(#3965),#2666,.F.);
#22796=ADVANCED_FACE('',(#3966),#2667,.F.);
#22797=ADVANCED_FACE('',(#3967,#1807),#2406,.T.);
#22798=ADVANCED_FACE('',(#3968),#21496,.T.);
#22799=ADVANCED_FACE('',(#3969,#1808),#2407,.T.);
#22800=ADVANCED_FACE('',(#3970),#2668,.T.);
#22801=ADVANCED_FACE('',(#3971),#21497,.T.);
#22802=ADVANCED_FACE('',(#3972,#1809),#2408,.T.);
#22803=ADVANCED_FACE('',(#3973),#21498,.F.);
#22804=CLOSED_SHELL('',(#21499,#21500,#21501,#21502,#21503,#21504,#21505,
#21506,#21507,#21508,#21509,#21510,#21511,#21512,#21513,#21514,#21515,#21516,
#21517,#21518,#21519,#21520,#21521,#21522,#21523,#21524,#21525,#21526,#21527,
#21528,#21529,#21530,#21531));
#22805=CLOSED_SHELL('',(#21532,#21533,#21534,#21535,#21536,#21537,#21538,
#21539,#21540,#21541));
#22806=CLOSED_SHELL('',(#21542,#21543,#21544,#21545,#21546,#21547,#21548,
#21549,#21550,#21551,#21552,#21553,#21554,#21555,#21556));
#22807=CLOSED_SHELL('',(#21557,#21558,#21559,#21560,#21561));
#22808=CLOSED_SHELL('',(#21562,#21563,#21564,#21565,#21566,#21567,#21568,
#21569,#21570,#21571));
#22809=CLOSED_SHELL('',(#21572,#21573,#21574,#21575,#21576,#21577,#21578,
#21579,#21580,#21581,#21582,#21583,#21584,#21585,#21586,#21587,#21588));
#22810=CLOSED_SHELL('',(#21589,#21590,#21591,#21592,#21593,#21594,#21595,
#21596,#21597,#21598,#21599,#21600,#21601,#21602,#21603,#21604,#21605,#21606,
#21607,#21608,#21609,#21610,#21611,#21612,#21613,#21614,#21615,#21616,#21617,
#21618,#21619,#21620,#21621,#21622,#21623,#21624,#21625,#21626,#21627,#21628,
#21629,#21630,#21631,#21632,#21633,#21634,#21635,#21636,#21637,#21638,#21639,
#21640,#21641,#21642,#21643,#21644,#21645,#21646,#21647,#21648,#21649,#21650,
#21651,#21652,#21653,#21654,#21655,#21656,#21657,#21658,#21659,#21660,#21661,
#21662,#21663,#21664,#21665,#21666,#21667,#21668,#21669,#21670,#21671,#21672,
#21673,#21674,#21675,#21676,#21677,#21678,#21679,#21680,#21681,#21682,#21683,
#21684,#21685,#21686,#21687,#21688,#21689,#21690,#21691,#21692,#21693,#21694,
#21695,#21696,#21697,#21698,#21699,#21700,#21701,#21702,#21703,#21704,#21705,
#21706,#21707,#21708,#21709,#21710,#21711,#21712,#21713,#21714,#21715,#21716,
#21717,#21718,#21719,#21720,#21721,#21722,#21723,#21724,#21725,#21726,#21727,
#21728,#21729,#21730,#21731,#21732,#21733,#21734,#21735,#21736,#21737,#21738,
#21739,#21740,#21741,#21742,#21743,#21744,#21745,#21746,#21747,#21748,#21749,
#21750));
#22811=CLOSED_SHELL('',(#21751,#21752,#21753,#21754,#21755,#21756,#21757,
#21758,#21759,#21760,#21761,#21762,#21763,#21764,#21765,#21766,#21767,#21768,
#21769,#21770,#21771,#21772,#21773,#21774,#21775,#21776,#21777,#21778,#21779,
#21780,#21781,#21782,#21783,#21784,#21785,#21786,#21787,#21788,#21789,#21790,
#21791,#21792,#21793,#21794,#21795,#21796,#21797,#21798,#21799,#21800,#21801,
#21802,#21803));
#22812=CLOSED_SHELL('',(#21804,#21805,#21806,#21807,#21808,#21809,#21810,
#21811,#21812,#21813,#21814,#21815,#21816,#21817,#21818,#21819,#21820,#21821,
#21822,#21823,#21824,#21825,#21826,#21827,#21828,#21829,#21830,#21831));
#22813=CLOSED_SHELL('',(#21832,#21833,#21834,#21835,#21836,#21837,#21838,
#21839,#21840,#21841,#21842,#21843,#21844,#21845,#21846,#21847,#21848,#21849,
#21850,#21851,#21852,#21853,#21854,#21855,#21856,#21857,#21858,#21859,#21860,
#21861,#21862,#21863,#21864,#21865,#21866,#21867,#21868,#21869,#21870,#21871,
#21872,#21873,#21874));
#22814=CLOSED_SHELL('',(#21875,#21876,#21877,#21878,#21879,#21880,#21881,
#21882,#21883,#21884,#21885,#21886,#21887,#21888,#21889,#21890,#21891,#21892,
#21893,#21894,#21895,#21896,#21897,#21898,#21899,#21900,#21901,#21902,#21903,
#21904,#21905,#21906,#21907,#21908,#21909,#21910,#21911,#21912,#21913,#21914,
#21915,#21916,#21917,#21918,#21919,#21920,#21921,#21922,#21923,#21924,#21925,
#21926,#21927,#21928,#21929,#21930,#21931,#21932,#21933,#21934,#21935,#21936));
#22815=CLOSED_SHELL('',(#21937,#21938,#21939,#21940,#21941,#21942,#21943,
#21944,#21945,#21946,#21947,#21948,#21949,#21950,#21951,#21952,#21953,#21954,
#21955,#21956,#21957,#21958,#21959,#21960,#21961,#21962,#21963,#21964,#21965,
#21966,#21967,#21968,#21969,#21970,#21971,#21972,#21973,#21974,#21975,#21976,
#21977,#21978,#21979,#21980,#21981,#21982,#21983,#21984,#21985,#21986,#21987,
#21988,#21989,#21990,#21991,#21992));
#22816=CLOSED_SHELL('',(#21993,#21994,#21995,#21996,#21997,#21998,#21999,
#22000,#22001,#22002,#22003,#22004,#22005,#22006,#22007,#22008,#22009,#22010,
#22011,#22012,#22013,#22014,#22015,#22016,#22017,#22018,#22019,#22020,#22021,
#22022,#22023,#22024,#22025,#22026,#22027,#22028,#22029,#22030,#22031,#22032,
#22033,#22034,#22035,#22036,#22037,#22038,#22039,#22040,#22041,#22042,#22043,
#22044,#22045,#22046,#22047,#22048,#22049,#22050,#22051,#22052,#22053,#22054,
#22055,#22056,#22057,#22058,#22059,#22060,#22061,#22062,#22063,#22064,#22065,
#22066,#22067,#22068,#22069,#22070,#22071,#22072,#22073,#22074,#22075,#22076,
#22077,#22078,#22079,#22080,#22081,#22082,#22083,#22084,#22085,#22086,#22087,
#22088,#22089,#22090,#22091,#22092,#22093,#22094,#22095,#22096,#22097,#22098,
#22099,#22100,#22101,#22102,#22103,#22104,#22105,#22106,#22107,#22108,#22109,
#22110,#22111,#22112,#22113,#22114,#22115,#22116,#22117,#22118,#22119,#22120,
#22121,#22122,#22123,#22124,#22125,#22126,#22127,#22128,#22129,#22130,#22131,
#22132,#22133,#22134,#22135,#22136,#22137,#22138,#22139,#22140,#22141,#22142,
#22143,#22144,#22145,#22146,#22147,#22148,#22149,#22150,#22151,#22152,#22153,
#22154,#22155,#22156,#22157,#22158,#22159,#22160,#22161,#22162,#22163,#22164,
#22165,#22166,#22167,#22168,#22169,#22170,#22171,#22172,#22173,#22174,#22175,
#22176,#22177,#22178,#22179,#22180,#22181,#22182,#22183,#22184,#22185,#22186,
#22187,#22188,#22189,#22190,#22191,#22192,#22193,#22194,#22195,#22196,#22197,
#22198,#22199,#22200,#22201,#22202,#22203,#22204,#22205,#22206,#22207,#22208,
#22209,#22210,#22211,#22212,#22213,#22214,#22215,#22216,#22217,#22218,#22219,
#22220,#22221,#22222,#22223,#22224,#22225,#22226,#22227,#22228,#22229,#22230,
#22231,#22232,#22233,#22234,#22235,#22236,#22237,#22238,#22239,#22240,#22241,
#22242,#22243,#22244,#22245,#22246,#22247,#22248,#22249,#22250,#22251,#22252,
#22253,#22254,#22255,#22256,#22257,#22258,#22259,#22260,#22261,#22262,#22263,
#22264,#22265,#22266,#22267,#22268,#22269,#22270,#22271,#22272,#22273,#22274,
#22275,#22276,#22277,#22278,#22279,#22280,#22281,#22282,#22283,#22284,#22285,
#22286,#22287,#22288,#22289,#22290,#22291,#22292,#22293,#22294,#22295,#22296,
#22297,#22298,#22299,#22300,#22301,#22302,#22303,#22304,#22305,#22306,#22307,
#22308,#22309,#22310,#22311,#22312,#22313,#22314,#22315,#22316,#22317,#22318,
#22319,#22320,#22321,#22322,#22323,#22324,#22325,#22326,#22327,#22328,#22329,
#22330,#22331,#22332,#22333,#22334,#22335,#22336,#22337,#22338,#22339,#22340,
#22341,#22342,#22343,#22344));
#22817=CLOSED_SHELL('',(#22345,#22346,#22347,#22348,#22349,#22350,#22351,
#22352,#22353,#22354,#22355,#22356,#22357,#22358,#22359,#22360,#22361,#22362));
#22818=CLOSED_SHELL('',(#22363,#22364,#22365,#22366,#22367,#22368,#22369,
#22370,#22371,#22372,#22373,#22374,#22375,#22376,#22377,#22378));
#22819=CLOSED_SHELL('',(#22379,#22380,#22381,#22382,#22383,#22384,#22385,
#22386,#22387,#22388,#22389,#22390,#22391,#22392,#22393,#22394,#22395,#22396,
#22397,#22398,#22399,#22400,#22401,#22402,#22403,#22404,#22405,#22406,#22407,
#22408,#22409,#22410,#22411,#22412,#22413,#22414,#22415,#22416,#22417,#22418,
#22419,#22420,#22421,#22422,#22423,#22424,#22425,#22426,#22427,#22428,#22429,
#22430,#22431,#22432,#22433,#22434,#22435,#22436,#22437,#22438,#22439,#22440,
#22441,#22442,#22443,#22444,#22445,#22446,#22447,#22448,#22449,#22450,#22451,
#22452,#22453,#22454,#22455,#22456,#22457,#22458,#22459,#22460,#22461,#22462,
#22463,#22464,#22465,#22466,#22467,#22468,#22469,#22470,#22471,#22472,#22473,
#22474,#22475,#22476,#22477,#22478,#22479,#22480,#22481,#22482,#22483,#22484,
#22485,#22486,#22487,#22488,#22489,#22490,#22491,#22492,#22493,#22494,#22495,
#22496,#22497,#22498,#22499,#22500,#22501,#22502,#22503,#22504,#22505,#22506,
#22507,#22508,#22509,#22510,#22511,#22512));
#22820=CLOSED_SHELL('',(#22513,#22514,#22515,#22516,#22517,#22518,#22519,
#22520));
#22821=CLOSED_SHELL('',(#22521,#22522,#22523,#22524,#22525,#22526,#22527,
#22528,#22529,#22530,#22531,#22532));
#22822=CLOSED_SHELL('',(#22533,#22534,#22535,#22536,#22537,#22538,#22539,
#22540,#22541,#22542,#22543,#22544,#22545,#22546,#22547,#22548,#22549,#22550,
#22551,#22552,#22553,#22554,#22555,#22556,#22557,#22558,#22559,#22560,#22561,
#22562,#22563,#22564,#22565,#22566,#22567,#22568,#22569,#22570,#22571,#22572,
#22573,#22574,#22575,#22576,#22577,#22578,#22579,#22580,#22581,#22582,#22583,
#22584,#22585,#22586,#22587,#22588,#22589,#22590,#22591,#22592,#22593,#22594,
#22595,#22596,#22597,#22598,#22599,#22600,#22601,#22602,#22603,#22604,#22605,
#22606,#22607,#22608,#22609,#22610,#22611,#22612,#22613,#22614,#22615,#22616,
#22617,#22618,#22619,#22620,#22621,#22622,#22623,#22624,#22625,#22626,#22627,
#22628,#22629,#22630,#22631,#22632,#22633,#22634,#22635,#22636,#22637,#22638,
#22639,#22640,#22641,#22642,#22643,#22644,#22645,#22646,#22647,#22648,#22649,
#22650,#22651,#22652,#22653,#22654,#22655,#22656,#22657,#22658,#22659,#22660,
#22661,#22662,#22663,#22664,#22665,#22666,#22667,#22668,#22669,#22670,#22671,
#22672,#22673,#22674,#22675,#22676,#22677,#22678,#22679,#22680,#22681,#22682,
#22683,#22684,#22685,#22686,#22687,#22688,#22689,#22690,#22691,#22692,#22693,
#22694,#22695,#22696,#22697,#22698,#22699,#22700,#22701,#22702,#22703,#22704,
#22705,#22706,#22707,#22708,#22709,#22710,#22711,#22712,#22713,#22714,#22715,
#22716,#22717,#22718,#22719,#22720,#22721,#22722,#22723,#22724,#22725,#22726,
#22727,#22728,#22729,#22730,#22731,#22732,#22733,#22734,#22735,#22736,#22737,
#22738,#22739,#22740,#22741,#22742,#22743));
#22823=CLOSED_SHELL('',(#22744,#22745,#22746,#22747,#22748,#22749,#22750,
#22751,#22752,#22753,#22754,#22755,#22756,#22757,#22758,#22759,#22760,#22761,
#22762,#22763,#22764,#22765,#22766,#22767,#22768,#22769,#22770,#22771,#22772,
#22773,#22774,#22775,#22776,#22777,#22778,#22779,#22780,#22781,#22782,#22783,
#22784,#22785,#22786,#22787,#22788,#22789,#22790,#22791,#22792,#22793,#22794,
#22795,#22796,#22797,#22798,#22799,#22800,#22801,#22802,#22803));
#22824=DERIVED_UNIT_ELEMENT(#22864,1.);
#22825=DERIVED_UNIT_ELEMENT(#59206,-3.);
#22826=DERIVED_UNIT_ELEMENT(#22864,1.);
#22827=DERIVED_UNIT_ELEMENT(#59206,-3.);
#22828=DERIVED_UNIT_ELEMENT(#22864,1.);
#22829=DERIVED_UNIT_ELEMENT(#59206,-3.);
#22830=DERIVED_UNIT_ELEMENT(#22864,1.);
#22831=DERIVED_UNIT_ELEMENT(#59206,-3.);
#22832=DERIVED_UNIT_ELEMENT(#22864,1.);
#22833=DERIVED_UNIT_ELEMENT(#59206,-3.);
#22834=DERIVED_UNIT_ELEMENT(#22864,1.);
#22835=DERIVED_UNIT_ELEMENT(#59206,-3.);
#22836=DERIVED_UNIT_ELEMENT(#22864,1.);
#22837=DERIVED_UNIT_ELEMENT(#59206,-3.);
#22838=DERIVED_UNIT_ELEMENT(#22864,1.);
#22839=DERIVED_UNIT_ELEMENT(#59206,-3.);
#22840=DERIVED_UNIT_ELEMENT(#22864,1.);
#22841=DERIVED_UNIT_ELEMENT(#59206,-3.);
#22842=DERIVED_UNIT_ELEMENT(#22864,1.);
#22843=DERIVED_UNIT_ELEMENT(#59206,-3.);
#22844=DERIVED_UNIT_ELEMENT(#22864,1.);
#22845=DERIVED_UNIT_ELEMENT(#59206,-3.);
#22846=DERIVED_UNIT_ELEMENT(#22864,1.);
#22847=DERIVED_UNIT_ELEMENT(#59206,-3.);
#22848=DERIVED_UNIT_ELEMENT(#22864,1.);
#22849=DERIVED_UNIT_ELEMENT(#59206,-3.);
#22850=DERIVED_UNIT_ELEMENT(#22864,1.);
#22851=DERIVED_UNIT_ELEMENT(#59206,-3.);
#22852=DERIVED_UNIT_ELEMENT(#22864,1.);
#22853=DERIVED_UNIT_ELEMENT(#59206,-3.);
#22854=DERIVED_UNIT_ELEMENT(#22864,1.);
#22855=DERIVED_UNIT_ELEMENT(#59206,-3.);
#22856=DERIVED_UNIT_ELEMENT(#22864,1.);
#22857=DERIVED_UNIT_ELEMENT(#59206,-3.);
#22858=DERIVED_UNIT_ELEMENT(#22864,1.);
#22859=DERIVED_UNIT_ELEMENT(#59206,-3.);
#22860=DERIVED_UNIT_ELEMENT(#22864,1.);
#22861=DERIVED_UNIT_ELEMENT(#59206,-3.);
#22862=DERIVED_UNIT_ELEMENT(#22864,1.);
#22863=DERIVED_UNIT_ELEMENT(#59206,-3.);
#22864=(
MASS_UNIT()
NAMED_UNIT(*)
SI_UNIT(.KILO.,.GRAM.)
);
#22865=DERIVED_UNIT((#22824,#22825));
#22866=DERIVED_UNIT((#22826,#22827));
#22867=DERIVED_UNIT((#22828,#22829));
#22868=DERIVED_UNIT((#22830,#22831));
#22869=DERIVED_UNIT((#22832,#22833));
#22870=DERIVED_UNIT((#22834,#22835));
#22871=DERIVED_UNIT((#22836,#22837));
#22872=DERIVED_UNIT((#22838,#22839));
#22873=DERIVED_UNIT((#22840,#22841));
#22874=DERIVED_UNIT((#22842,#22843));
#22875=DERIVED_UNIT((#22844,#22845));
#22876=DERIVED_UNIT((#22846,#22847));
#22877=DERIVED_UNIT((#22848,#22849));
#22878=DERIVED_UNIT((#22850,#22851));
#22879=DERIVED_UNIT((#22852,#22853));
#22880=DERIVED_UNIT((#22854,#22855));
#22881=DERIVED_UNIT((#22856,#22857));
#22882=DERIVED_UNIT((#22858,#22859));
#22883=DERIVED_UNIT((#22860,#22861));
#22884=DERIVED_UNIT((#22862,#22863));
#22885=MEASURE_REPRESENTATION_ITEM('density measure',
POSITIVE_RATIO_MEASURE(7850.),#22865);
#22886=MEASURE_REPRESENTATION_ITEM('density measure',
POSITIVE_RATIO_MEASURE(7850.),#22866);
#22887=MEASURE_REPRESENTATION_ITEM('density measure',
POSITIVE_RATIO_MEASURE(7850.),#22867);
#22888=MEASURE_REPRESENTATION_ITEM('density measure',
POSITIVE_RATIO_MEASURE(7850.),#22868);
#22889=MEASURE_REPRESENTATION_ITEM('density measure',
POSITIVE_RATIO_MEASURE(7850.),#22869);
#22890=MEASURE_REPRESENTATION_ITEM('density measure',
POSITIVE_RATIO_MEASURE(930.),#22870);
#22891=MEASURE_REPRESENTATION_ITEM('density measure',
POSITIVE_RATIO_MEASURE(7850.),#22871);
#22892=MEASURE_REPRESENTATION_ITEM('density measure',
POSITIVE_RATIO_MEASURE(7850.),#22872);
#22893=MEASURE_REPRESENTATION_ITEM('density measure',
POSITIVE_RATIO_MEASURE(7850.),#22873);
#22894=MEASURE_REPRESENTATION_ITEM('density measure',
POSITIVE_RATIO_MEASURE(7850.),#22874);
#22895=MEASURE_REPRESENTATION_ITEM('density measure',
POSITIVE_RATIO_MEASURE(7150.),#22875);
#22896=MEASURE_REPRESENTATION_ITEM('density measure',
POSITIVE_RATIO_MEASURE(7850.),#22876);
#22897=MEASURE_REPRESENTATION_ITEM('density measure',
POSITIVE_RATIO_MEASURE(7150.),#22877);
#22898=MEASURE_REPRESENTATION_ITEM('density measure',
POSITIVE_RATIO_MEASURE(7850.),#22878);
#22899=MEASURE_REPRESENTATION_ITEM('density measure',
POSITIVE_RATIO_MEASURE(8470.),#22879);
#22900=MEASURE_REPRESENTATION_ITEM('density measure',
POSITIVE_RATIO_MEASURE(7850.),#22880);
#22901=MEASURE_REPRESENTATION_ITEM('density measure',
POSITIVE_RATIO_MEASURE(7850.),#22881);
#22902=MEASURE_REPRESENTATION_ITEM('density measure',
POSITIVE_RATIO_MEASURE(7850.),#22882);
#22903=MEASURE_REPRESENTATION_ITEM('density measure',
POSITIVE_RATIO_MEASURE(7850.),#22883);
#22904=MEASURE_REPRESENTATION_ITEM('density measure',
POSITIVE_RATIO_MEASURE(7850.),#22884);
#22905=PROPERTY_DEFINITION_REPRESENTATION(#23005,#22945);
#22906=PROPERTY_DEFINITION_REPRESENTATION(#23006,#22946);
#22907=PROPERTY_DEFINITION_REPRESENTATION(#23007,#22947);
#22908=PROPERTY_DEFINITION_REPRESENTATION(#23008,#22948);
#22909=PROPERTY_DEFINITION_REPRESENTATION(#23009,#22949);
#22910=PROPERTY_DEFINITION_REPRESENTATION(#23010,#22950);
#22911=PROPERTY_DEFINITION_REPRESENTATION(#23011,#22951);
#22912=PROPERTY_DEFINITION_REPRESENTATION(#23012,#22952);
#22913=PROPERTY_DEFINITION_REPRESENTATION(#23013,#22953);
#22914=PROPERTY_DEFINITION_REPRESENTATION(#23014,#22954);
#22915=PROPERTY_DEFINITION_REPRESENTATION(#23015,#22955);
#22916=PROPERTY_DEFINITION_REPRESENTATION(#23016,#22956);
#22917=PROPERTY_DEFINITION_REPRESENTATION(#23017,#22957);
#22918=PROPERTY_DEFINITION_REPRESENTATION(#23018,#22958);
#22919=PROPERTY_DEFINITION_REPRESENTATION(#23019,#22959);
#22920=PROPERTY_DEFINITION_REPRESENTATION(#23020,#22960);
#22921=PROPERTY_DEFINITION_REPRESENTATION(#23021,#22961);
#22922=PROPERTY_DEFINITION_REPRESENTATION(#23022,#22962);
#22923=PROPERTY_DEFINITION_REPRESENTATION(#23023,#22963);
#22924=PROPERTY_DEFINITION_REPRESENTATION(#23024,#22964);
#22925=PROPERTY_DEFINITION_REPRESENTATION(#23025,#22965);
#22926=PROPERTY_DEFINITION_REPRESENTATION(#23026,#22966);
#22927=PROPERTY_DEFINITION_REPRESENTATION(#23027,#22967);
#22928=PROPERTY_DEFINITION_REPRESENTATION(#23028,#22968);
#22929=PROPERTY_DEFINITION_REPRESENTATION(#23029,#22969);
#22930=PROPERTY_DEFINITION_REPRESENTATION(#23030,#22970);
#22931=PROPERTY_DEFINITION_REPRESENTATION(#23031,#22971);
#22932=PROPERTY_DEFINITION_REPRESENTATION(#23032,#22972);
#22933=PROPERTY_DEFINITION_REPRESENTATION(#23033,#22973);
#22934=PROPERTY_DEFINITION_REPRESENTATION(#23034,#22974);
#22935=PROPERTY_DEFINITION_REPRESENTATION(#23035,#22975);
#22936=PROPERTY_DEFINITION_REPRESENTATION(#23036,#22976);
#22937=PROPERTY_DEFINITION_REPRESENTATION(#23037,#22977);
#22938=PROPERTY_DEFINITION_REPRESENTATION(#23038,#22978);
#22939=PROPERTY_DEFINITION_REPRESENTATION(#23039,#22979);
#22940=PROPERTY_DEFINITION_REPRESENTATION(#23040,#22980);
#22941=PROPERTY_DEFINITION_REPRESENTATION(#23041,#22981);
#22942=PROPERTY_DEFINITION_REPRESENTATION(#23042,#22982);
#22943=PROPERTY_DEFINITION_REPRESENTATION(#23043,#22983);
#22944=PROPERTY_DEFINITION_REPRESENTATION(#23044,#22984);
#22945=REPRESENTATION('material name',(#22985),#59184);
#22946=REPRESENTATION('density',(#22885),#59184);
#22947=REPRESENTATION('material name',(#22986),#59185);
#22948=REPRESENTATION('density',(#22886),#59185);
#22949=REPRESENTATION('material name',(#22987),#59186);
#22950=REPRESENTATION('density',(#22887),#59186);
#22951=REPRESENTATION('material name',(#22988),#59187);
#22952=REPRESENTATION('density',(#22888),#59187);
#22953=REPRESENTATION('material name',(#22989),#59188);
#22954=REPRESENTATION('density',(#22889),#59188);
#22955=REPRESENTATION('material name',(#22990),#59189);
#22956=REPRESENTATION('density',(#22890),#59189);
#22957=REPRESENTATION('material name',(#22991),#59190);
#22958=REPRESENTATION('density',(#22891),#59190);
#22959=REPRESENTATION('material name',(#22992),#59191);
#22960=REPRESENTATION('density',(#22892),#59191);
#22961=REPRESENTATION('material name',(#22993),#59192);
#22962=REPRESENTATION('density',(#22893),#59192);
#22963=REPRESENTATION('material name',(#22994),#59193);
#22964=REPRESENTATION('density',(#22894),#59193);
#22965=REPRESENTATION('material name',(#22995),#59194);
#22966=REPRESENTATION('density',(#22895),#59194);
#22967=REPRESENTATION('material name',(#22996),#59195);
#22968=REPRESENTATION('density',(#22896),#59195);
#22969=REPRESENTATION('material name',(#22997),#59196);
#22970=REPRESENTATION('density',(#22897),#59196);
#22971=REPRESENTATION('material name',(#22998),#59197);
#22972=REPRESENTATION('density',(#22898),#59197);
#22973=REPRESENTATION('material name',(#22999),#59198);
#22974=REPRESENTATION('density',(#22899),#59198);
#22975=REPRESENTATION('material name',(#23000),#59199);
#22976=REPRESENTATION('density',(#22900),#59199);
#22977=REPRESENTATION('material name',(#23001),#59200);
#22978=REPRESENTATION('density',(#22901),#59200);
#22979=REPRESENTATION('material name',(#23002),#59201);
#22980=REPRESENTATION('density',(#22902),#59201);
#22981=REPRESENTATION('material name',(#23003),#59202);
#22982=REPRESENTATION('density',(#22903),#59202);
#22983=REPRESENTATION('material name',(#23004),#59203);
#22984=REPRESENTATION('density',(#22904),#59203);
#22985=DESCRIPTIVE_REPRESENTATION_ITEM('Steel','Steel');
#22986=DESCRIPTIVE_REPRESENTATION_ITEM('Steel','Steel');
#22987=DESCRIPTIVE_REPRESENTATION_ITEM('Steel','Steel');
#22988=DESCRIPTIVE_REPRESENTATION_ITEM('Steel','Steel');
#22989=DESCRIPTIVE_REPRESENTATION_ITEM('Steel','Steel');
#22990=DESCRIPTIVE_REPRESENTATION_ITEM('Rubber','Rubber');
#22991=DESCRIPTIVE_REPRESENTATION_ITEM('Steel','Steel');
#22992=DESCRIPTIVE_REPRESENTATION_ITEM('Steel','Steel');
#22993=DESCRIPTIVE_REPRESENTATION_ITEM('Steel','Steel');
#22994=DESCRIPTIVE_REPRESENTATION_ITEM('Steel','Steel');
#22995=DESCRIPTIVE_REPRESENTATION_ITEM('Iron, Cast','Iron, Cast');
#22996=DESCRIPTIVE_REPRESENTATION_ITEM('Steel','Steel');
#22997=DESCRIPTIVE_REPRESENTATION_ITEM('Iron, Cast','Iron, Cast');
#22998=DESCRIPTIVE_REPRESENTATION_ITEM('Steel','Steel');
#22999=DESCRIPTIVE_REPRESENTATION_ITEM('Bronze','Bronze');
#23000=DESCRIPTIVE_REPRESENTATION_ITEM('Steel','Steel');
#23001=DESCRIPTIVE_REPRESENTATION_ITEM('Steel','Steel');
#23002=DESCRIPTIVE_REPRESENTATION_ITEM('Steel','Steel');
#23003=DESCRIPTIVE_REPRESENTATION_ITEM('Steel','Steel');
#23004=DESCRIPTIVE_REPRESENTATION_ITEM('Steel','Steel');
#23005=PROPERTY_DEFINITION('material property','material name',#59319);
#23006=PROPERTY_DEFINITION('material property','density of part',#59319);
#23007=PROPERTY_DEFINITION('material property','material name',#59320);
#23008=PROPERTY_DEFINITION('material property','density of part',#59320);
#23009=PROPERTY_DEFINITION('material property','material name',#59321);
#23010=PROPERTY_DEFINITION('material property','density of part',#59321);
#23011=PROPERTY_DEFINITION('material property','material name',#59322);
#23012=PROPERTY_DEFINITION('material property','density of part',#59322);
#23013=PROPERTY_DEFINITION('material property','material name',#59323);
#23014=PROPERTY_DEFINITION('material property','density of part',#59323);
#23015=PROPERTY_DEFINITION('material property','material name',#59324);
#23016=PROPERTY_DEFINITION('material property','density of part',#59324);
#23017=PROPERTY_DEFINITION('material property','material name',#59325);
#23018=PROPERTY_DEFINITION('material property','density of part',#59325);
#23019=PROPERTY_DEFINITION('material property','material name',#59326);
#23020=PROPERTY_DEFINITION('material property','density of part',#59326);
#23021=PROPERTY_DEFINITION('material property','material name',#59327);
#23022=PROPERTY_DEFINITION('material property','density of part',#59327);
#23023=PROPERTY_DEFINITION('material property','material name',#59328);
#23024=PROPERTY_DEFINITION('material property','density of part',#59328);
#23025=PROPERTY_DEFINITION('material property','material name',#59329);
#23026=PROPERTY_DEFINITION('material property','density of part',#59329);
#23027=PROPERTY_DEFINITION('material property','material name',#59330);
#23028=PROPERTY_DEFINITION('material property','density of part',#59330);
#23029=PROPERTY_DEFINITION('material property','material name',#59331);
#23030=PROPERTY_DEFINITION('material property','density of part',#59331);
#23031=PROPERTY_DEFINITION('material property','material name',#59332);
#23032=PROPERTY_DEFINITION('material property','density of part',#59332);
#23033=PROPERTY_DEFINITION('material property','material name',#59333);
#23034=PROPERTY_DEFINITION('material property','density of part',#59333);
#23035=PROPERTY_DEFINITION('material property','material name',#59334);
#23036=PROPERTY_DEFINITION('material property','density of part',#59334);
#23037=PROPERTY_DEFINITION('material property','material name',#59335);
#23038=PROPERTY_DEFINITION('material property','density of part',#59335);
#23039=PROPERTY_DEFINITION('material property','material name',#59336);
#23040=PROPERTY_DEFINITION('material property','density of part',#59336);
#23041=PROPERTY_DEFINITION('material property','material name',#59337);
#23042=PROPERTY_DEFINITION('material property','density of part',#59337);
#23043=PROPERTY_DEFINITION('material property','material name',#59338);
#23044=PROPERTY_DEFINITION('material property','density of part',#59338);
#23045=AXIS2_PLACEMENT_3D('',#30691,#25116,#25117);
#23046=AXIS2_PLACEMENT_3D('',#30692,#25118,#25119);
#23047=AXIS2_PLACEMENT_3D('',#30693,#25120,#25121);
#23048=AXIS2_PLACEMENT_3D('',#30695,#25122,#25123);
#23049=AXIS2_PLACEMENT_3D('',#30698,#25125,#25126);
#23050=AXIS2_PLACEMENT_3D('',#30699,#25127,#25128);
#23051=AXIS2_PLACEMENT_3D('',#30702,#25130,#25131);
#23052=AXIS2_PLACEMENT_3D('',#30703,#25132,#25133);
#23053=AXIS2_PLACEMENT_3D('',#30705,#25134,#25135);
#23054=AXIS2_PLACEMENT_3D('',#30707,#25136,#25137);
#23055=AXIS2_PLACEMENT_3D('',#30709,#25138,#25139);
#23056=AXIS2_PLACEMENT_3D('',#30711,#25140,#25141);
#23057=AXIS2_PLACEMENT_3D('',#30713,#25142,#25143);
#23058=AXIS2_PLACEMENT_3D('',#30715,#25144,#25145);
#23059=AXIS2_PLACEMENT_3D('',#30717,#25146,#25147);
#23060=AXIS2_PLACEMENT_3D('',#30719,#25148,#25149);
#23061=AXIS2_PLACEMENT_3D('',#30721,#25150,#25151);
#23062=AXIS2_PLACEMENT_3D('',#30723,#25152,#25153);
#23063=AXIS2_PLACEMENT_3D('',#30724,#25154,#25155);
#23064=AXIS2_PLACEMENT_3D('',#30726,#25156,#25157);
#23065=AXIS2_PLACEMENT_3D('',#30728,#25159,#25160);
#23066=AXIS2_PLACEMENT_3D('',#30730,#25161,#25162);
#23067=AXIS2_PLACEMENT_3D('',#30732,#25163,#25164);
#23068=AXIS2_PLACEMENT_3D('',#30734,#25165,#25166);
#23069=AXIS2_PLACEMENT_3D('',#30736,#25167,#25168);
#23070=AXIS2_PLACEMENT_3D('',#30738,#25169,#25170);
#23071=AXIS2_PLACEMENT_3D('',#30740,#25171,#25172);
#23072=AXIS2_PLACEMENT_3D('',#30742,#25173,#25174);
#23073=AXIS2_PLACEMENT_3D('',#30744,#25175,#25176);
#23074=AXIS2_PLACEMENT_3D('',#30746,#25177,#25178);
#23075=AXIS2_PLACEMENT_3D('',#30748,#25179,#25180);
#23076=AXIS2_PLACEMENT_3D('',#30749,#25181,#25182);
#23077=AXIS2_PLACEMENT_3D('',#30752,#25184,#25185);
#23078=AXIS2_PLACEMENT_3D('',#30753,#25186,#25187);
#23079=AXIS2_PLACEMENT_3D('',#30756,#25189,#25190);
#23080=AXIS2_PLACEMENT_3D('',#30757,#25191,#25192);
#23081=AXIS2_PLACEMENT_3D('',#30759,#25194,#25195);
#23082=AXIS2_PLACEMENT_3D('',#30762,#25197,#25198);
#23083=AXIS2_PLACEMENT_3D('',#30763,#25199,#25200);
#23084=AXIS2_PLACEMENT_3D('',#30766,#25202,#25203);
#23085=AXIS2_PLACEMENT_3D('',#30767,#25204,#25205);
#23086=AXIS2_PLACEMENT_3D('',#30769,#25207,#25208);
#23087=AXIS2_PLACEMENT_3D('',#30772,#25210,#25211);
#23088=AXIS2_PLACEMENT_3D('',#30773,#25212,#25213);
#23089=AXIS2_PLACEMENT_3D('',#30776,#25215,#25216);
#23090=AXIS2_PLACEMENT_3D('',#30777,#25217,#25218);
#23091=AXIS2_PLACEMENT_3D('',#30779,#25220,#25221);
#23092=AXIS2_PLACEMENT_3D('',#30782,#25223,#25224);
#23093=AXIS2_PLACEMENT_3D('',#30783,#25225,#25226);
#23094=AXIS2_PLACEMENT_3D('',#30786,#25228,#25229);
#23095=AXIS2_PLACEMENT_3D('',#30787,#25230,#25231);
#23096=AXIS2_PLACEMENT_3D('',#30789,#25233,#25234);
#23097=AXIS2_PLACEMENT_3D('',#30792,#25236,#25237);
#23098=AXIS2_PLACEMENT_3D('',#30793,#25238,#25239);
#23099=AXIS2_PLACEMENT_3D('',#30796,#25241,#25242);
#23100=AXIS2_PLACEMENT_3D('',#30797,#25243,#25244);
#23101=AXIS2_PLACEMENT_3D('',#30799,#25246,#25247);
#23102=AXIS2_PLACEMENT_3D('',#30802,#25249,#25250);
#23103=AXIS2_PLACEMENT_3D('',#30803,#25251,#25252);
#23104=AXIS2_PLACEMENT_3D('',#30806,#25254,#25255);
#23105=AXIS2_PLACEMENT_3D('',#30807,#25256,#25257);
#23106=AXIS2_PLACEMENT_3D('',#30809,#25259,#25260);
#23107=AXIS2_PLACEMENT_3D('',#30812,#25262,#25263);
#23108=AXIS2_PLACEMENT_3D('',#30813,#25264,#25265);
#23109=AXIS2_PLACEMENT_3D('',#30816,#25267,#25268);
#23110=AXIS2_PLACEMENT_3D('',#30817,#25269,#25270);
#23111=AXIS2_PLACEMENT_3D('',#30819,#25272,#25273);
#23112=AXIS2_PLACEMENT_3D('',#30822,#25275,#25276);
#23113=AXIS2_PLACEMENT_3D('',#30823,#25277,#25278);
#23114=AXIS2_PLACEMENT_3D('',#30826,#25280,#25281);
#23115=AXIS2_PLACEMENT_3D('',#30827,#25282,#25283);
#23116=AXIS2_PLACEMENT_3D('',#30829,#25285,#25286);
#23117=AXIS2_PLACEMENT_3D('',#30830,#25287,#25288);
#23118=AXIS2_PLACEMENT_3D('',#30831,#25289,#25290);
#23119=AXIS2_PLACEMENT_3D('',#30833,#25291,#25292);
#23120=AXIS2_PLACEMENT_3D('',#30835,#25294,#25295);
#23121=AXIS2_PLACEMENT_3D('',#30837,#25296,#25297);
#23122=AXIS2_PLACEMENT_3D('',#30839,#25299,#25300);
#23123=AXIS2_PLACEMENT_3D('',#30841,#25302,#25303);
#23124=AXIS2_PLACEMENT_3D('',#30842,#25304,#25305);
#23125=AXIS2_PLACEMENT_3D('',#30844,#25306,#25307);
#23126=AXIS2_PLACEMENT_3D('',#30847,#25309,#25310);
#23127=AXIS2_PLACEMENT_3D('',#30848,#25311,#25312);
#23128=AXIS2_PLACEMENT_3D('',#30850,#25313,#25314);
#23129=AXIS2_PLACEMENT_3D('',#30851,#25315,#25316);
#23130=AXIS2_PLACEMENT_3D('',#30853,#25317,#25318);
#23131=AXIS2_PLACEMENT_3D('',#30855,#25320,#25321);
#23132=AXIS2_PLACEMENT_3D('',#30857,#25322,#25323);
#23133=AXIS2_PLACEMENT_3D('',#30859,#25325,#25326);
#23134=AXIS2_PLACEMENT_3D('',#30861,#25327,#25328);
#23135=AXIS2_PLACEMENT_3D('',#30862,#25329,#25330);
#23136=AXIS2_PLACEMENT_3D('',#30865,#25332,#25333);
#23137=AXIS2_PLACEMENT_3D('',#30866,#25334,#25335);
#23138=AXIS2_PLACEMENT_3D('',#30869,#25337,#25338);
#23139=AXIS2_PLACEMENT_3D('',#30870,#25339,#25340);
#23140=AXIS2_PLACEMENT_3D('',#30873,#25342,#25343);
#23141=AXIS2_PLACEMENT_3D('',#30874,#25344,#25345);
#23142=AXIS2_PLACEMENT_3D('',#30876,#25346,#25347);
#23143=AXIS2_PLACEMENT_3D('',#30877,#25348,#25349);
#23144=AXIS2_PLACEMENT_3D('',#30878,#25350,#25351);
#23145=AXIS2_PLACEMENT_3D('',#30879,#25352,#25353);
#23146=AXIS2_PLACEMENT_3D('',#30880,#25354,#25355);
#23147=AXIS2_PLACEMENT_3D('',#30906,#25363,#25364);
#23148=AXIS2_PLACEMENT_3D('',#30932,#25372,#25373);
#23149=AXIS2_PLACEMENT_3D('',#30935,#25376,#25377);
#23150=AXIS2_PLACEMENT_3D('',#30936,#25378,#25379);
#23151=AXIS2_PLACEMENT_3D('',#30938,#25380,#25381);
#23152=AXIS2_PLACEMENT_3D('',#30939,#25382,#25383);
#23153=AXIS2_PLACEMENT_3D('',#30940,#25384,#25385);
#23154=AXIS2_PLACEMENT_3D('',#31004,#25387,#25388);
#23155=AXIS2_PLACEMENT_3D('',#31008,#25390,#25391);
#23156=AXIS2_PLACEMENT_3D('',#31009,#25392,#25393);
#23157=AXIS2_PLACEMENT_3D('',#31010,#25394,#25395);
#23158=AXIS2_PLACEMENT_3D('',#31090,#25397,#25398);
#23159=AXIS2_PLACEMENT_3D('',#31109,#25399,#25400);
#23160=AXIS2_PLACEMENT_3D('',#31110,#25401,#25402);
#23161=AXIS2_PLACEMENT_3D('',#31180,#25404,#25405);
#23162=AXIS2_PLACEMENT_3D('',#31181,#25406,#25407);
#23163=AXIS2_PLACEMENT_3D('',#31182,#25408,#25409);
#23164=AXIS2_PLACEMENT_3D('',#31183,#25410,#25411);
#23165=AXIS2_PLACEMENT_3D('',#31184,#25412,#25413);
#23166=AXIS2_PLACEMENT_3D('',#31185,#25414,#25415);
#23167=AXIS2_PLACEMENT_3D('',#31186,#25416,#25417);
#23168=AXIS2_PLACEMENT_3D('',#31226,#25419,#25420);
#23169=AXIS2_PLACEMENT_3D('',#31228,#25421,#25422);
#23170=AXIS2_PLACEMENT_3D('',#31229,#25423,#25424);
#23171=AXIS2_PLACEMENT_3D('',#31230,#25425,#25426);
#23172=AXIS2_PLACEMENT_3D('',#31273,#25428,#25429);
#23173=AXIS2_PLACEMENT_3D('',#31274,#25430,#25431);
#23174=AXIS2_PLACEMENT_3D('',#32185,#25432,#25433);
#23175=AXIS2_PLACEMENT_3D('',#32186,#25434,#25435);
#23176=AXIS2_PLACEMENT_3D('',#32195,#25440,#25441);
#23177=AXIS2_PLACEMENT_3D('',#32199,#25443,#25444);
#23178=AXIS2_PLACEMENT_3D('',#32200,#25445,#25446);
#23179=AXIS2_PLACEMENT_3D('',#32201,#25447,#25448);
#23180=AXIS2_PLACEMENT_3D('',#32207,#25452,#25453);
#23181=AXIS2_PLACEMENT_3D('',#32208,#25454,#25455);
#23182=AXIS2_PLACEMENT_3D('',#32209,#25456,#25457);
#23183=AXIS2_PLACEMENT_3D('',#32210,#25458,#25459);
#23184=AXIS2_PLACEMENT_3D('',#32214,#25461,#25462);
#23185=AXIS2_PLACEMENT_3D('',#32216,#25464,#25465);
#23186=AXIS2_PLACEMENT_3D('',#32220,#25468,#25469);
#23187=AXIS2_PLACEMENT_3D('',#32221,#25470,#25471);
#23188=AXIS2_PLACEMENT_3D('',#32224,#25473,#25474);
#23189=AXIS2_PLACEMENT_3D('',#32225,#25475,#25476);
#23190=AXIS2_PLACEMENT_3D('',#32227,#25478,#25479);
#23191=AXIS2_PLACEMENT_3D('',#32228,#25480,#25481);
#23192=AXIS2_PLACEMENT_3D('',#32229,#25482,#25483);
#23193=AXIS2_PLACEMENT_3D('',#32231,#25484,#25485);
#23194=AXIS2_PLACEMENT_3D('',#32234,#25487,#25488);
#23195=AXIS2_PLACEMENT_3D('',#32235,#25489,#25490);
#23196=AXIS2_PLACEMENT_3D('',#32237,#25491,#25492);
#23197=AXIS2_PLACEMENT_3D('',#32240,#25494,#25495);
#23198=AXIS2_PLACEMENT_3D('',#32241,#25496,#25497);
#23199=AXIS2_PLACEMENT_3D('',#32242,#25498,#25499);
#23200=AXIS2_PLACEMENT_3D('',#32244,#25500,#25501);
#23201=AXIS2_PLACEMENT_3D('',#32245,#25502,#25503);
#23202=AXIS2_PLACEMENT_3D('',#32247,#25504,#25505);
#23203=AXIS2_PLACEMENT_3D('',#32251,#25507,#25508);
#23204=AXIS2_PLACEMENT_3D('',#32252,#25509,#25510);
#23205=AXIS2_PLACEMENT_3D('',#32253,#25511,#25512);
#23206=AXIS2_PLACEMENT_3D('',#32257,#25514,#25515);
#23207=AXIS2_PLACEMENT_3D('',#32258,#25516,#25517);
#23208=AXIS2_PLACEMENT_3D('',#32259,#25518,#25519);
#23209=AXIS2_PLACEMENT_3D('',#32260,#25520,#25521);
#23210=AXIS2_PLACEMENT_3D('',#32263,#25523,#25524);
#23211=AXIS2_PLACEMENT_3D('',#32264,#25525,#25526);
#23212=AXIS2_PLACEMENT_3D('',#32266,#25527,#25528);
#23213=AXIS2_PLACEMENT_3D('',#32267,#25529,#25530);
#23214=AXIS2_PLACEMENT_3D('',#32269,#25531,#25532);
#23215=AXIS2_PLACEMENT_3D('',#32271,#25534,#25535);
#23216=AXIS2_PLACEMENT_3D('',#32274,#25537,#25538);
#23217=AXIS2_PLACEMENT_3D('',#32275,#25539,#25540);
#23218=AXIS2_PLACEMENT_3D('',#32278,#25542,#25543);
#23219=AXIS2_PLACEMENT_3D('',#32279,#25544,#25545);
#23220=AXIS2_PLACEMENT_3D('',#32282,#25547,#25548);
#23221=AXIS2_PLACEMENT_3D('',#32283,#25549,#25550);
#23222=AXIS2_PLACEMENT_3D('',#32286,#25552,#25553);
#23223=AXIS2_PLACEMENT_3D('',#32287,#25554,#25555);
#23224=AXIS2_PLACEMENT_3D('',#32290,#25557,#25558);
#23225=AXIS2_PLACEMENT_3D('',#32291,#25559,#25560);
#23226=AXIS2_PLACEMENT_3D('',#32294,#25562,#25563);
#23227=AXIS2_PLACEMENT_3D('',#32295,#25564,#25565);
#23228=AXIS2_PLACEMENT_3D('',#32296,#25566,#25567);
#23229=AXIS2_PLACEMENT_3D('',#32297,#25568,#25569);
#23230=AXIS2_PLACEMENT_3D('',#32314,#25571,#25572);
#23231=AXIS2_PLACEMENT_3D('',#32325,#25573,#25574);
#23232=AXIS2_PLACEMENT_3D('',#32363,#25576,#25577);
#23233=AXIS2_PLACEMENT_3D('',#32401,#25579,#25580);
#23234=AXIS2_PLACEMENT_3D('',#32438,#25582,#25583);
#23235=AXIS2_PLACEMENT_3D('',#32475,#25585,#25586);
#23236=AXIS2_PLACEMENT_3D('',#32513,#25588,#25589);
#23237=AXIS2_PLACEMENT_3D('',#32551,#25591,#25592);
#23238=AXIS2_PLACEMENT_3D('',#32556,#25594,#25595);
#23239=AXIS2_PLACEMENT_3D('',#34639,#25596,#25597);
#23240=AXIS2_PLACEMENT_3D('',#34641,#25598,#25599);
#23241=AXIS2_PLACEMENT_3D('',#34642,#25600,#25601);
#23242=AXIS2_PLACEMENT_3D('',#34708,#25602,#25603);
#23243=AXIS2_PLACEMENT_3D('',#34709,#25604,#25605);
#23244=AXIS2_PLACEMENT_3D('',#36391,#25606,#25607);
#23245=AXIS2_PLACEMENT_3D('',#36400,#25612,#25613);
#23246=AXIS2_PLACEMENT_3D('',#36406,#25617,#25618);
#23247=AXIS2_PLACEMENT_3D('',#36412,#25622,#25623);
#23248=AXIS2_PLACEMENT_3D('',#36418,#25627,#25628);
#23249=AXIS2_PLACEMENT_3D('',#36424,#25632,#25633);
#23250=AXIS2_PLACEMENT_3D('',#36427,#25636,#25637);
#23251=AXIS2_PLACEMENT_3D('',#36428,#25638,#25639);
#23252=AXIS2_PLACEMENT_3D('',#36437,#25644,#25645);
#23253=AXIS2_PLACEMENT_3D('',#36439,#25646,#25647);
#23254=AXIS2_PLACEMENT_3D('',#36441,#25649,#25650);
#23255=AXIS2_PLACEMENT_3D('',#36445,#25653,#25654);
#23256=AXIS2_PLACEMENT_3D('',#36446,#25655,#25656);
#23257=AXIS2_PLACEMENT_3D('',#36447,#25657,#25658);
#23258=AXIS2_PLACEMENT_3D('',#36456,#25663,#25664);
#23259=AXIS2_PLACEMENT_3D('',#36458,#25665,#25666);
#23260=AXIS2_PLACEMENT_3D('',#36460,#25668,#25669);
#23261=AXIS2_PLACEMENT_3D('',#36464,#25672,#25673);
#23262=AXIS2_PLACEMENT_3D('',#36465,#25674,#25675);
#23263=AXIS2_PLACEMENT_3D('',#36466,#25676,#25677);
#23264=AXIS2_PLACEMENT_3D('',#36475,#25682,#25683);
#23265=AXIS2_PLACEMENT_3D('',#36477,#25684,#25685);
#23266=AXIS2_PLACEMENT_3D('',#36479,#25687,#25688);
#23267=AXIS2_PLACEMENT_3D('',#36483,#25691,#25692);
#23268=AXIS2_PLACEMENT_3D('',#36484,#25693,#25694);
#23269=AXIS2_PLACEMENT_3D('',#36485,#25695,#25696);
#23270=AXIS2_PLACEMENT_3D('',#36494,#25701,#25702);
#23271=AXIS2_PLACEMENT_3D('',#36496,#25703,#25704);
#23272=AXIS2_PLACEMENT_3D('',#36498,#25706,#25707);
#23273=AXIS2_PLACEMENT_3D('',#36502,#25710,#25711);
#23274=AXIS2_PLACEMENT_3D('',#36503,#25712,#25713);
#23275=AXIS2_PLACEMENT_3D('',#36504,#25714,#25715);
#23276=AXIS2_PLACEMENT_3D('',#36513,#25720,#25721);
#23277=AXIS2_PLACEMENT_3D('',#36515,#25722,#25723);
#23278=AXIS2_PLACEMENT_3D('',#36517,#25725,#25726);
#23279=AXIS2_PLACEMENT_3D('',#36521,#25729,#25730);
#23280=AXIS2_PLACEMENT_3D('',#36522,#25731,#25732);
#23281=AXIS2_PLACEMENT_3D('',#36523,#25733,#25734);
#23282=AXIS2_PLACEMENT_3D('',#36532,#25739,#25740);
#23283=AXIS2_PLACEMENT_3D('',#36534,#25741,#25742);
#23284=AXIS2_PLACEMENT_3D('',#36536,#25744,#25745);
#23285=AXIS2_PLACEMENT_3D('',#36540,#25748,#25749);
#23286=AXIS2_PLACEMENT_3D('',#36541,#25750,#25751);
#23287=AXIS2_PLACEMENT_3D('',#36542,#25752,#25753);
#23288=AXIS2_PLACEMENT_3D('',#36551,#25758,#25759);
#23289=AXIS2_PLACEMENT_3D('',#36553,#25760,#25761);
#23290=AXIS2_PLACEMENT_3D('',#36555,#25763,#25764);
#23291=AXIS2_PLACEMENT_3D('',#36559,#25767,#25768);
#23292=AXIS2_PLACEMENT_3D('',#36560,#25769,#25770);
#23293=AXIS2_PLACEMENT_3D('',#36561,#25771,#25772);
#23294=AXIS2_PLACEMENT_3D('',#36564,#25773,#25774);
#23295=AXIS2_PLACEMENT_3D('',#36568,#25777,#25778);
#23296=AXIS2_PLACEMENT_3D('',#36574,#25782,#25783);
#23297=AXIS2_PLACEMENT_3D('',#36578,#25786,#25787);
#23298=AXIS2_PLACEMENT_3D('',#36579,#25788,#25789);
#23299=AXIS2_PLACEMENT_3D('',#36580,#25790,#25791);
#23300=AXIS2_PLACEMENT_3D('',#36589,#25796,#25797);
#23301=AXIS2_PLACEMENT_3D('',#36591,#25798,#25799);
#23302=AXIS2_PLACEMENT_3D('',#36593,#25801,#25802);
#23303=AXIS2_PLACEMENT_3D('',#36597,#25805,#25806);
#23304=AXIS2_PLACEMENT_3D('',#36598,#25807,#25808);
#23305=AXIS2_PLACEMENT_3D('',#36599,#25809,#25810);
#23306=AXIS2_PLACEMENT_3D('',#36608,#25815,#25816);
#23307=AXIS2_PLACEMENT_3D('',#36610,#25817,#25818);
#23308=AXIS2_PLACEMENT_3D('',#36612,#25820,#25821);
#23309=AXIS2_PLACEMENT_3D('',#36616,#25824,#25825);
#23310=AXIS2_PLACEMENT_3D('',#36617,#25826,#25827);
#23311=AXIS2_PLACEMENT_3D('',#36618,#25828,#25829);
#23312=AXIS2_PLACEMENT_3D('',#36627,#25834,#25835);
#23313=AXIS2_PLACEMENT_3D('',#36629,#25836,#25837);
#23314=AXIS2_PLACEMENT_3D('',#36631,#25839,#25840);
#23315=AXIS2_PLACEMENT_3D('',#36635,#25843,#25844);
#23316=AXIS2_PLACEMENT_3D('',#36636,#25845,#25846);
#23317=AXIS2_PLACEMENT_3D('',#36637,#25847,#25848);
#23318=AXIS2_PLACEMENT_3D('',#36646,#25853,#25854);
#23319=AXIS2_PLACEMENT_3D('',#36648,#25855,#25856);
#23320=AXIS2_PLACEMENT_3D('',#36650,#25858,#25859);
#23321=AXIS2_PLACEMENT_3D('',#36654,#25862,#25863);
#23322=AXIS2_PLACEMENT_3D('',#36655,#25864,#25865);
#23323=AXIS2_PLACEMENT_3D('',#36656,#25866,#25867);
#23324=AXIS2_PLACEMENT_3D('',#36665,#25872,#25873);
#23325=AXIS2_PLACEMENT_3D('',#36667,#25874,#25875);
#23326=AXIS2_PLACEMENT_3D('',#36669,#25877,#25878);
#23327=AXIS2_PLACEMENT_3D('',#36673,#25881,#25882);
#23328=AXIS2_PLACEMENT_3D('',#36674,#25883,#25884);
#23329=AXIS2_PLACEMENT_3D('',#36675,#25885,#25886);
#23330=AXIS2_PLACEMENT_3D('',#36684,#25891,#25892);
#23331=AXIS2_PLACEMENT_3D('',#36686,#25893,#25894);
#23332=AXIS2_PLACEMENT_3D('',#36688,#25896,#25897);
#23333=AXIS2_PLACEMENT_3D('',#36692,#25900,#25901);
#23334=AXIS2_PLACEMENT_3D('',#36693,#25902,#25903);
#23335=AXIS2_PLACEMENT_3D('',#36694,#25904,#25905);
#23336=AXIS2_PLACEMENT_3D('',#36703,#25910,#25911);
#23337=AXIS2_PLACEMENT_3D('',#36705,#25912,#25913);
#23338=AXIS2_PLACEMENT_3D('',#36707,#25915,#25916);
#23339=AXIS2_PLACEMENT_3D('',#36711,#25919,#25920);
#23340=AXIS2_PLACEMENT_3D('',#36712,#25921,#25922);
#23341=AXIS2_PLACEMENT_3D('',#36713,#25923,#25924);
#23342=AXIS2_PLACEMENT_3D('',#36722,#25929,#25930);
#23343=AXIS2_PLACEMENT_3D('',#36724,#25931,#25932);
#23344=AXIS2_PLACEMENT_3D('',#36726,#25934,#25935);
#23345=AXIS2_PLACEMENT_3D('',#36730,#25938,#25939);
#23346=AXIS2_PLACEMENT_3D('',#36731,#25940,#25941);
#23347=AXIS2_PLACEMENT_3D('',#36732,#25942,#25943);
#23348=AXIS2_PLACEMENT_3D('',#36741,#25948,#25949);
#23349=AXIS2_PLACEMENT_3D('',#36743,#25950,#25951);
#23350=AXIS2_PLACEMENT_3D('',#36745,#25953,#25954);
#23351=AXIS2_PLACEMENT_3D('',#36749,#25957,#25958);
#23352=AXIS2_PLACEMENT_3D('',#36750,#25959,#25960);
#23353=AXIS2_PLACEMENT_3D('',#36751,#25961,#25962);
#23354=AXIS2_PLACEMENT_3D('',#36760,#25967,#25968);
#23355=AXIS2_PLACEMENT_3D('',#36762,#25969,#25970);
#23356=AXIS2_PLACEMENT_3D('',#36764,#25972,#25973);
#23357=AXIS2_PLACEMENT_3D('',#36768,#25976,#25977);
#23358=AXIS2_PLACEMENT_3D('',#36769,#25978,#25979);
#23359=AXIS2_PLACEMENT_3D('',#36770,#25980,#25981);
#23360=AXIS2_PLACEMENT_3D('',#36779,#25986,#25987);
#23361=AXIS2_PLACEMENT_3D('',#36781,#25988,#25989);
#23362=AXIS2_PLACEMENT_3D('',#36783,#25991,#25992);
#23363=AXIS2_PLACEMENT_3D('',#36787,#25995,#25996);
#23364=AXIS2_PLACEMENT_3D('',#36788,#25997,#25998);
#23365=AXIS2_PLACEMENT_3D('',#36789,#25999,#26000);
#23366=AXIS2_PLACEMENT_3D('',#36798,#26005,#26006);
#23367=AXIS2_PLACEMENT_3D('',#36800,#26007,#26008);
#23368=AXIS2_PLACEMENT_3D('',#36802,#26010,#26011);
#23369=AXIS2_PLACEMENT_3D('',#36806,#26014,#26015);
#23370=AXIS2_PLACEMENT_3D('',#36807,#26016,#26017);
#23371=AXIS2_PLACEMENT_3D('',#36808,#26018,#26019);
#23372=AXIS2_PLACEMENT_3D('',#36817,#26024,#26025);
#23373=AXIS2_PLACEMENT_3D('',#36819,#26026,#26027);
#23374=AXIS2_PLACEMENT_3D('',#36821,#26029,#26030);
#23375=AXIS2_PLACEMENT_3D('',#36825,#26033,#26034);
#23376=AXIS2_PLACEMENT_3D('',#36826,#26035,#26036);
#23377=AXIS2_PLACEMENT_3D('',#36827,#26037,#26038);
#23378=AXIS2_PLACEMENT_3D('',#36836,#26043,#26044);
#23379=AXIS2_PLACEMENT_3D('',#36838,#26045,#26046);
#23380=AXIS2_PLACEMENT_3D('',#36840,#26048,#26049);
#23381=AXIS2_PLACEMENT_3D('',#36844,#26052,#26053);
#23382=AXIS2_PLACEMENT_3D('',#36845,#26054,#26055);
#23383=AXIS2_PLACEMENT_3D('',#36846,#26056,#26057);
#23384=AXIS2_PLACEMENT_3D('',#36855,#26062,#26063);
#23385=AXIS2_PLACEMENT_3D('',#36857,#26064,#26065);
#23386=AXIS2_PLACEMENT_3D('',#36860,#26067,#26068);
#23387=AXIS2_PLACEMENT_3D('',#36861,#26069,#26070);
#23388=AXIS2_PLACEMENT_3D('',#36865,#26073,#26074);
#23389=AXIS2_PLACEMENT_3D('',#36867,#26075,#26076);
#23390=AXIS2_PLACEMENT_3D('',#36868,#26077,#26078);
#23391=AXIS2_PLACEMENT_3D('',#36869,#26079,#26080);
#23392=AXIS2_PLACEMENT_3D('',#36878,#26085,#26086);
#23393=AXIS2_PLACEMENT_3D('',#36880,#26087,#26088);
#23394=AXIS2_PLACEMENT_3D('',#36882,#26090,#26091);
#23395=AXIS2_PLACEMENT_3D('',#36886,#26094,#26095);
#23396=AXIS2_PLACEMENT_3D('',#36887,#26096,#26097);
#23397=AXIS2_PLACEMENT_3D('',#36888,#26098,#26099);
#23398=AXIS2_PLACEMENT_3D('',#36897,#26104,#26105);
#23399=AXIS2_PLACEMENT_3D('',#36899,#26106,#26107);
#23400=AXIS2_PLACEMENT_3D('',#36901,#26109,#26110);
#23401=AXIS2_PLACEMENT_3D('',#36905,#26113,#26114);
#23402=AXIS2_PLACEMENT_3D('',#36906,#26115,#26116);
#23403=AXIS2_PLACEMENT_3D('',#36907,#26117,#26118);
#23404=AXIS2_PLACEMENT_3D('',#36916,#26123,#26124);
#23405=AXIS2_PLACEMENT_3D('',#36918,#26125,#26126);
#23406=AXIS2_PLACEMENT_3D('',#36920,#26128,#26129);
#23407=AXIS2_PLACEMENT_3D('',#36924,#26132,#26133);
#23408=AXIS2_PLACEMENT_3D('',#36925,#26134,#26135);
#23409=AXIS2_PLACEMENT_3D('',#36926,#26136,#26137);
#23410=AXIS2_PLACEMENT_3D('',#36935,#26142,#26143);
#23411=AXIS2_PLACEMENT_3D('',#36937,#26144,#26145);
#23412=AXIS2_PLACEMENT_3D('',#36939,#26147,#26148);
#23413=AXIS2_PLACEMENT_3D('',#36943,#26151,#26152);
#23414=AXIS2_PLACEMENT_3D('',#36944,#26153,#26154);
#23415=AXIS2_PLACEMENT_3D('',#36945,#26155,#26156);
#23416=AXIS2_PLACEMENT_3D('',#36954,#26161,#26162);
#23417=AXIS2_PLACEMENT_3D('',#36956,#26163,#26164);
#23418=AXIS2_PLACEMENT_3D('',#36958,#26166,#26167);
#23419=AXIS2_PLACEMENT_3D('',#36962,#26170,#26171);
#23420=AXIS2_PLACEMENT_3D('',#36963,#26172,#26173);
#23421=AXIS2_PLACEMENT_3D('',#36964,#26174,#26175);
#23422=AXIS2_PLACEMENT_3D('',#36973,#26180,#26181);
#23423=AXIS2_PLACEMENT_3D('',#36975,#26182,#26183);
#23424=AXIS2_PLACEMENT_3D('',#36977,#26185,#26186);
#23425=AXIS2_PLACEMENT_3D('',#36981,#26189,#26190);
#23426=AXIS2_PLACEMENT_3D('',#36982,#26191,#26192);
#23427=AXIS2_PLACEMENT_3D('',#36983,#26193,#26194);
#23428=AXIS2_PLACEMENT_3D('',#36992,#26199,#26200);
#23429=AXIS2_PLACEMENT_3D('',#36994,#26201,#26202);
#23430=AXIS2_PLACEMENT_3D('',#36996,#26204,#26205);
#23431=AXIS2_PLACEMENT_3D('',#37000,#26208,#26209);
#23432=AXIS2_PLACEMENT_3D('',#37001,#26210,#26211);
#23433=AXIS2_PLACEMENT_3D('',#37002,#26212,#26213);
#23434=AXIS2_PLACEMENT_3D('',#37004,#26214,#26215);
#23435=AXIS2_PLACEMENT_3D('',#37034,#26217,#26218);
#23436=AXIS2_PLACEMENT_3D('',#37042,#26221,#26222);
#23437=AXIS2_PLACEMENT_3D('',#37048,#26224,#26225);
#23438=AXIS2_PLACEMENT_3D('',#37054,#26227,#26228);
#23439=AXIS2_PLACEMENT_3D('',#37065,#26230,#26231);
#23440=AXIS2_PLACEMENT_3D('',#37073,#26232,#26233);
#23441=AXIS2_PLACEMENT_3D('',#37075,#26235,#26236);
#23442=AXIS2_PLACEMENT_3D('',#37077,#26237,#26238);
#23443=AXIS2_PLACEMENT_3D('',#37078,#26239,#26240);
#23444=AXIS2_PLACEMENT_3D('',#37080,#26241,#26242);
#23445=AXIS2_PLACEMENT_3D('',#37081,#26243,#26244);
#23446=AXIS2_PLACEMENT_3D('',#37083,#26246,#26247);
#23447=AXIS2_PLACEMENT_3D('',#37084,#26248,#26249);
#23448=AXIS2_PLACEMENT_3D('',#37086,#26250,#26251);
#23449=AXIS2_PLACEMENT_3D('',#37089,#26253,#26254);
#23450=AXIS2_PLACEMENT_3D('',#37090,#26255,#26256);
#23451=AXIS2_PLACEMENT_3D('',#37093,#26258,#26259);
#23452=AXIS2_PLACEMENT_3D('',#37095,#26260,#26261);
#23453=AXIS2_PLACEMENT_3D('',#37096,#26262,#26263);
#23454=AXIS2_PLACEMENT_3D('',#37098,#26265,#26266);
#23455=AXIS2_PLACEMENT_3D('',#37100,#26267,#26268);
#23456=AXIS2_PLACEMENT_3D('',#37101,#26269,#26270);
#23457=AXIS2_PLACEMENT_3D('',#37103,#26272,#26273);
#23458=AXIS2_PLACEMENT_3D('',#37104,#26274,#26275);
#23459=AXIS2_PLACEMENT_3D('',#37105,#26276,#26277);
#23460=AXIS2_PLACEMENT_3D('',#37106,#26278,#26279);
#23461=AXIS2_PLACEMENT_3D('',#37107,#26280,#26281);
#23462=AXIS2_PLACEMENT_3D('',#37108,#26282,#26283);
#23463=AXIS2_PLACEMENT_3D('',#37109,#26284,#26285);
#23464=AXIS2_PLACEMENT_3D('',#37110,#26286,#26287);
#23465=AXIS2_PLACEMENT_3D('',#37111,#26288,#26289);
#23466=AXIS2_PLACEMENT_3D('',#37112,#26290,#26291);
#23467=AXIS2_PLACEMENT_3D('',#37113,#26292,#26293);
#23468=AXIS2_PLACEMENT_3D('',#37114,#26294,#26295);
#23469=AXIS2_PLACEMENT_3D('',#37115,#26296,#26297);
#23470=AXIS2_PLACEMENT_3D('',#37116,#26298,#26299);
#23471=AXIS2_PLACEMENT_3D('',#37118,#26301,#26302);
#23472=AXIS2_PLACEMENT_3D('',#37119,#26303,#26304);
#23473=AXIS2_PLACEMENT_3D('',#37120,#26305,#26306);
#23474=AXIS2_PLACEMENT_3D('',#37121,#26307,#26308);
#23475=AXIS2_PLACEMENT_3D('',#37122,#26309,#26310);
#23476=AXIS2_PLACEMENT_3D('',#37123,#26311,#26312);
#23477=AXIS2_PLACEMENT_3D('',#37124,#26313,#26314);
#23478=AXIS2_PLACEMENT_3D('',#37125,#26315,#26316);
#23479=AXIS2_PLACEMENT_3D('',#37126,#26317,#26318);
#23480=AXIS2_PLACEMENT_3D('',#37127,#26319,#26320);
#23481=AXIS2_PLACEMENT_3D('',#37128,#26321,#26322);
#23482=AXIS2_PLACEMENT_3D('',#37129,#26323,#26324);
#23483=AXIS2_PLACEMENT_3D('',#37130,#26325,#26326);
#23484=AXIS2_PLACEMENT_3D('',#37131,#26327,#26328);
#23485=AXIS2_PLACEMENT_3D('',#37132,#26329,#26330);
#23486=AXIS2_PLACEMENT_3D('',#37133,#26331,#26332);
#23487=AXIS2_PLACEMENT_3D('',#37134,#26333,#26334);
#23488=AXIS2_PLACEMENT_3D('',#37135,#26335,#26336);
#23489=AXIS2_PLACEMENT_3D('',#37137,#26337,#26338);
#23490=AXIS2_PLACEMENT_3D('',#37139,#26340,#26341);
#23491=AXIS2_PLACEMENT_3D('',#37140,#26342,#26343);
#23492=AXIS2_PLACEMENT_3D('',#37141,#26344,#26345);
#23493=AXIS2_PLACEMENT_3D('',#37158,#26347,#26348);
#23494=AXIS2_PLACEMENT_3D('',#37169,#26349,#26350);
#23495=AXIS2_PLACEMENT_3D('',#37207,#26352,#26353);
#23496=AXIS2_PLACEMENT_3D('',#37245,#26355,#26356);
#23497=AXIS2_PLACEMENT_3D('',#37283,#26358,#26359);
#23498=AXIS2_PLACEMENT_3D('',#37288,#26361,#26362);
#23499=AXIS2_PLACEMENT_3D('',#37322,#26363,#26364);
#23500=AXIS2_PLACEMENT_3D('',#37344,#26366,#26367);
#23501=AXIS2_PLACEMENT_3D('',#37355,#26368,#26369);
#23502=AXIS2_PLACEMENT_3D('',#37439,#26371,#26372);
#23503=AXIS2_PLACEMENT_3D('',#37529,#26374,#26375);
#23504=AXIS2_PLACEMENT_3D('',#37613,#26377,#26378);
#23505=AXIS2_PLACEMENT_3D('',#37703,#26380,#26381);
#23506=AXIS2_PLACEMENT_3D('',#37793,#26383,#26384);
#23507=AXIS2_PLACEMENT_3D('',#37877,#26386,#26387);
#23508=AXIS2_PLACEMENT_3D('',#37891,#26389,#26390);
#23509=AXIS2_PLACEMENT_3D('',#37897,#26391,#26392);
#23510=AXIS2_PLACEMENT_3D('',#37934,#26394,#26395);
#23511=AXIS2_PLACEMENT_3D('',#37971,#26397,#26398);
#23512=AXIS2_PLACEMENT_3D('',#38009,#26400,#26401);
#23513=AXIS2_PLACEMENT_3D('',#38046,#26403,#26404);
#23514=AXIS2_PLACEMENT_3D('',#38083,#26406,#26407);
#23515=AXIS2_PLACEMENT_3D('',#38120,#26409,#26410);
#23516=AXIS2_PLACEMENT_3D('',#38196,#26411,#26412);
#23517=AXIS2_PLACEMENT_3D('',#38198,#26413,#26414);
#23518=AXIS2_PLACEMENT_3D('',#38774,#26415,#26416);
#23519=AXIS2_PLACEMENT_3D('',#38776,#26417,#26418);
#23520=AXIS2_PLACEMENT_3D('',#39270,#26419,#26420);
#23521=AXIS2_PLACEMENT_3D('',#39271,#26421,#26422);
#23522=AXIS2_PLACEMENT_3D('',#40593,#26423,#26424);
#23523=AXIS2_PLACEMENT_3D('',#40595,#26425,#26426);
#23524=AXIS2_PLACEMENT_3D('',#40596,#26427,#26428);
#23525=AXIS2_PLACEMENT_3D('',#40662,#26429,#26430);
#23526=AXIS2_PLACEMENT_3D('',#40663,#26431,#26432);
#23527=AXIS2_PLACEMENT_3D('',#41734,#26433,#26434);
#23528=AXIS2_PLACEMENT_3D('',#41736,#26435,#26436);
#23529=AXIS2_PLACEMENT_3D('',#41766,#26438,#26439);
#23530=AXIS2_PLACEMENT_3D('',#41774,#26442,#26443);
#23531=AXIS2_PLACEMENT_3D('',#41780,#26445,#26446);
#23532=AXIS2_PLACEMENT_3D('',#41786,#26448,#26449);
#23533=AXIS2_PLACEMENT_3D('',#41797,#26451,#26452);
#23534=AXIS2_PLACEMENT_3D('',#41805,#26453,#26454);
#23535=AXIS2_PLACEMENT_3D('',#41807,#26456,#26457);
#23536=AXIS2_PLACEMENT_3D('',#41808,#26458,#26459);
#23537=AXIS2_PLACEMENT_3D('',#41810,#26460,#26461);
#23538=AXIS2_PLACEMENT_3D('',#41811,#26462,#26463);
#23539=AXIS2_PLACEMENT_3D('',#41813,#26464,#26465);
#23540=AXIS2_PLACEMENT_3D('',#41814,#26466,#26467);
#23541=AXIS2_PLACEMENT_3D('',#41816,#26468,#26469);
#23542=AXIS2_PLACEMENT_3D('',#41817,#26470,#26471);
#23543=AXIS2_PLACEMENT_3D('',#41819,#26473,#26474);
#23544=AXIS2_PLACEMENT_3D('',#41820,#26475,#26476);
#23545=AXIS2_PLACEMENT_3D('',#41823,#26478,#26479);
#23546=AXIS2_PLACEMENT_3D('',#41824,#26480,#26481);
#23547=AXIS2_PLACEMENT_3D('',#41826,#26482,#26483);
#23548=AXIS2_PLACEMENT_3D('',#41828,#26485,#26486);
#23549=AXIS2_PLACEMENT_3D('',#41830,#26487,#26488);
#23550=AXIS2_PLACEMENT_3D('',#41831,#26489,#26490);
#23551=AXIS2_PLACEMENT_3D('',#41833,#26492,#26493);
#23552=AXIS2_PLACEMENT_3D('',#41835,#26494,#26495);
#23553=AXIS2_PLACEMENT_3D('',#41836,#26496,#26497);
#23554=AXIS2_PLACEMENT_3D('',#41838,#26499,#26500);
#23555=AXIS2_PLACEMENT_3D('',#41840,#26501,#26502);
#23556=AXIS2_PLACEMENT_3D('',#41842,#26504,#26505);
#23557=AXIS2_PLACEMENT_3D('',#41844,#26506,#26507);
#23558=AXIS2_PLACEMENT_3D('',#41845,#26508,#26509);
#23559=AXIS2_PLACEMENT_3D('',#41847,#26511,#26512);
#23560=AXIS2_PLACEMENT_3D('',#41848,#26513,#26514);
#23561=AXIS2_PLACEMENT_3D('',#41850,#26515,#26516);
#23562=AXIS2_PLACEMENT_3D('',#41853,#26518,#26519);
#23563=AXIS2_PLACEMENT_3D('',#41854,#26520,#26521);
#23564=AXIS2_PLACEMENT_3D('',#41857,#26523,#26524);
#23565=AXIS2_PLACEMENT_3D('',#41866,#26529,#26530);
#23566=AXIS2_PLACEMENT_3D('',#41887,#26531,#26532);
#23567=AXIS2_PLACEMENT_3D('',#41889,#26534,#26535);
#23568=AXIS2_PLACEMENT_3D('',#41895,#26539,#26540);
#23569=AXIS2_PLACEMENT_3D('',#41914,#26541,#26542);
#23570=AXIS2_PLACEMENT_3D('',#41915,#26543,#26544);
#23571=AXIS2_PLACEMENT_3D('',#41916,#26545,#26546);
#23572=AXIS2_PLACEMENT_3D('',#41925,#26551,#26552);
#23573=AXIS2_PLACEMENT_3D('',#41946,#26553,#26554);
#23574=AXIS2_PLACEMENT_3D('',#41948,#26556,#26557);
#23575=AXIS2_PLACEMENT_3D('',#41954,#26561,#26562);
#23576=AXIS2_PLACEMENT_3D('',#41973,#26563,#26564);
#23577=AXIS2_PLACEMENT_3D('',#41974,#26565,#26566);
#23578=AXIS2_PLACEMENT_3D('',#41975,#26567,#26568);
#23579=AXIS2_PLACEMENT_3D('',#41977,#26569,#26570);
#23580=AXIS2_PLACEMENT_3D('',#41978,#26571,#26572);
#23581=AXIS2_PLACEMENT_3D('',#41980,#26573,#26574);
#23582=AXIS2_PLACEMENT_3D('',#41982,#26576,#26577);
#23583=AXIS2_PLACEMENT_3D('',#41984,#26578,#26579);
#23584=AXIS2_PLACEMENT_3D('',#41986,#26581,#26582);
#23585=AXIS2_PLACEMENT_3D('',#41988,#26583,#26584);
#23586=AXIS2_PLACEMENT_3D('',#41989,#26585,#26586);
#23587=AXIS2_PLACEMENT_3D('',#41991,#26587,#26588);
#23588=AXIS2_PLACEMENT_3D('',#41993,#26590,#26591);
#23589=AXIS2_PLACEMENT_3D('',#41995,#26592,#26593);
#23590=AXIS2_PLACEMENT_3D('',#41997,#26595,#26596);
#23591=AXIS2_PLACEMENT_3D('',#41999,#26597,#26598);
#23592=AXIS2_PLACEMENT_3D('',#42000,#26599,#26600);
#23593=AXIS2_PLACEMENT_3D('',#42002,#26601,#26602);
#23594=AXIS2_PLACEMENT_3D('',#42004,#26604,#26605);
#23595=AXIS2_PLACEMENT_3D('',#42006,#26606,#26607);
#23596=AXIS2_PLACEMENT_3D('',#42007,#26608,#26609);
#23597=AXIS2_PLACEMENT_3D('',#42009,#26610,#26611);
#23598=AXIS2_PLACEMENT_3D('',#42011,#26613,#26614);
#23599=AXIS2_PLACEMENT_3D('',#42013,#26615,#26616);
#23600=AXIS2_PLACEMENT_3D('',#42014,#26617,#26618);
#23601=AXIS2_PLACEMENT_3D('',#42016,#26619,#26620);
#23602=AXIS2_PLACEMENT_3D('',#42018,#26622,#26623);
#23603=AXIS2_PLACEMENT_3D('',#42020,#26624,#26625);
#23604=AXIS2_PLACEMENT_3D('',#42021,#26626,#26627);
#23605=AXIS2_PLACEMENT_3D('',#42023,#26628,#26629);
#23606=AXIS2_PLACEMENT_3D('',#42025,#26631,#26632);
#23607=AXIS2_PLACEMENT_3D('',#42027,#26633,#26634);
#23608=AXIS2_PLACEMENT_3D('',#42029,#26636,#26637);
#23609=AXIS2_PLACEMENT_3D('',#42030,#26638,#26639);
#23610=AXIS2_PLACEMENT_3D('',#42031,#26640,#26641);
#23611=AXIS2_PLACEMENT_3D('',#42033,#26642,#26643);
#23612=AXIS2_PLACEMENT_3D('',#42035,#26644,#26645);
#23613=AXIS2_PLACEMENT_3D('',#42036,#26646,#26647);
#23614=AXIS2_PLACEMENT_3D('',#42038,#26648,#26649);
#23615=AXIS2_PLACEMENT_3D('',#42040,#26651,#26652);
#23616=AXIS2_PLACEMENT_3D('',#42042,#26653,#26654);
#23617=AXIS2_PLACEMENT_3D('',#42043,#26655,#26656);
#23618=AXIS2_PLACEMENT_3D('',#42046,#26658,#26659);
#23619=AXIS2_PLACEMENT_3D('',#42047,#26660,#26661);
#23620=AXIS2_PLACEMENT_3D('',#42056,#26666,#26667);
#23621=AXIS2_PLACEMENT_3D('',#42062,#26671,#26672);
#23622=AXIS2_PLACEMENT_3D('',#42068,#26676,#26677);
#23623=AXIS2_PLACEMENT_3D('',#42070,#26678,#26679);
#23624=AXIS2_PLACEMENT_3D('',#42071,#26680,#26681);
#23625=AXIS2_PLACEMENT_3D('',#42072,#26682,#26683);
#23626=AXIS2_PLACEMENT_3D('',#42074,#26684,#26685);
#23627=AXIS2_PLACEMENT_3D('',#42077,#26687,#26688);
#23628=AXIS2_PLACEMENT_3D('',#42078,#26689,#26690);
#23629=AXIS2_PLACEMENT_3D('',#42080,#26691,#26692);
#23630=AXIS2_PLACEMENT_3D('',#42083,#26694,#26695);
#23631=AXIS2_PLACEMENT_3D('',#42084,#26696,#26697);
#23632=AXIS2_PLACEMENT_3D('',#42086,#26698,#26699);
#23633=AXIS2_PLACEMENT_3D('',#42089,#26701,#26702);
#23634=AXIS2_PLACEMENT_3D('',#42090,#26703,#26704);
#23635=AXIS2_PLACEMENT_3D('',#42092,#26705,#26706);
#23636=AXIS2_PLACEMENT_3D('',#42095,#26708,#26709);
#23637=AXIS2_PLACEMENT_3D('',#42096,#26710,#26711);
#23638=AXIS2_PLACEMENT_3D('',#42098,#26712,#26713);
#23639=AXIS2_PLACEMENT_3D('',#42101,#26715,#26716);
#23640=AXIS2_PLACEMENT_3D('',#42102,#26717,#26718);
#23641=AXIS2_PLACEMENT_3D('',#42104,#26719,#26720);
#23642=AXIS2_PLACEMENT_3D('',#42107,#26722,#26723);
#23643=AXIS2_PLACEMENT_3D('',#42108,#26724,#26725);
#23644=AXIS2_PLACEMENT_3D('',#42110,#26726,#26727);
#23645=AXIS2_PLACEMENT_3D('',#42113,#26729,#26730);
#23646=AXIS2_PLACEMENT_3D('',#42114,#26731,#26732);
#23647=AXIS2_PLACEMENT_3D('',#42116,#26733,#26734);
#23648=AXIS2_PLACEMENT_3D('',#42119,#26736,#26737);
#23649=AXIS2_PLACEMENT_3D('',#42120,#26738,#26739);
#23650=AXIS2_PLACEMENT_3D('',#42122,#26740,#26741);
#23651=AXIS2_PLACEMENT_3D('',#42125,#26743,#26744);
#23652=AXIS2_PLACEMENT_3D('',#42126,#26745,#26746);
#23653=AXIS2_PLACEMENT_3D('',#42136,#26747,#26748);
#23654=AXIS2_PLACEMENT_3D('',#42139,#26750,#26751);
#23655=AXIS2_PLACEMENT_3D('',#42140,#26752,#26753);
#23656=AXIS2_PLACEMENT_3D('',#42141,#26754,#26755);
#23657=AXIS2_PLACEMENT_3D('',#42142,#26756,#26757);
#23658=AXIS2_PLACEMENT_3D('',#42152,#26758,#26759);
#23659=AXIS2_PLACEMENT_3D('',#42155,#26761,#26762);
#23660=AXIS2_PLACEMENT_3D('',#42156,#26763,#26764);
#23661=AXIS2_PLACEMENT_3D('',#42157,#26765,#26766);
#23662=AXIS2_PLACEMENT_3D('',#42158,#26767,#26768);
#23663=AXIS2_PLACEMENT_3D('',#42168,#26769,#26770);
#23664=AXIS2_PLACEMENT_3D('',#42171,#26772,#26773);
#23665=AXIS2_PLACEMENT_3D('',#42172,#26774,#26775);
#23666=AXIS2_PLACEMENT_3D('',#42173,#26776,#26777);
#23667=AXIS2_PLACEMENT_3D('',#42174,#26778,#26779);
#23668=AXIS2_PLACEMENT_3D('',#42184,#26780,#26781);
#23669=AXIS2_PLACEMENT_3D('',#42187,#26783,#26784);
#23670=AXIS2_PLACEMENT_3D('',#42188,#26785,#26786);
#23671=AXIS2_PLACEMENT_3D('',#42189,#26787,#26788);
#23672=AXIS2_PLACEMENT_3D('',#42190,#26789,#26790);
#23673=AXIS2_PLACEMENT_3D('',#42200,#26791,#26792);
#23674=AXIS2_PLACEMENT_3D('',#42203,#26794,#26795);
#23675=AXIS2_PLACEMENT_3D('',#42204,#26796,#26797);
#23676=AXIS2_PLACEMENT_3D('',#42205,#26798,#26799);
#23677=AXIS2_PLACEMENT_3D('',#42206,#26800,#26801);
#23678=AXIS2_PLACEMENT_3D('',#42216,#26802,#26803);
#23679=AXIS2_PLACEMENT_3D('',#42219,#26805,#26806);
#23680=AXIS2_PLACEMENT_3D('',#42220,#26807,#26808);
#23681=AXIS2_PLACEMENT_3D('',#42221,#26809,#26810);
#23682=AXIS2_PLACEMENT_3D('',#42222,#26811,#26812);
#23683=AXIS2_PLACEMENT_3D('',#42232,#26813,#26814);
#23684=AXIS2_PLACEMENT_3D('',#42235,#26816,#26817);
#23685=AXIS2_PLACEMENT_3D('',#42236,#26818,#26819);
#23686=AXIS2_PLACEMENT_3D('',#42237,#26820,#26821);
#23687=AXIS2_PLACEMENT_3D('',#42238,#26822,#26823);
#23688=AXIS2_PLACEMENT_3D('',#42248,#26824,#26825);
#23689=AXIS2_PLACEMENT_3D('',#42251,#26827,#26828);
#23690=AXIS2_PLACEMENT_3D('',#42252,#26829,#26830);
#23691=AXIS2_PLACEMENT_3D('',#42253,#26831,#26832);
#23692=AXIS2_PLACEMENT_3D('',#42254,#26833,#26834);
#23693=AXIS2_PLACEMENT_3D('',#42264,#26835,#26836);
#23694=AXIS2_PLACEMENT_3D('',#42267,#26838,#26839);
#23695=AXIS2_PLACEMENT_3D('',#42268,#26840,#26841);
#23696=AXIS2_PLACEMENT_3D('',#42269,#26842,#26843);
#23697=AXIS2_PLACEMENT_3D('',#42270,#26844,#26845);
#23698=AXIS2_PLACEMENT_3D('',#42271,#26846,#26847);
#23699=AXIS2_PLACEMENT_3D('',#42272,#26848,#26849);
#23700=AXIS2_PLACEMENT_3D('',#42274,#26850,#26851);
#23701=AXIS2_PLACEMENT_3D('',#42275,#26852,#26853);
#23702=AXIS2_PLACEMENT_3D('',#42276,#26854,#26855);
#23703=AXIS2_PLACEMENT_3D('',#42277,#26856,#26857);
#23704=AXIS2_PLACEMENT_3D('',#42278,#26858,#26859);
#23705=AXIS2_PLACEMENT_3D('',#42279,#26860,#26861);
#23706=AXIS2_PLACEMENT_3D('',#42280,#26862,#26863);
#23707=AXIS2_PLACEMENT_3D('',#42281,#26864,#26865);
#23708=AXIS2_PLACEMENT_3D('',#42283,#26866,#26867);
#23709=AXIS2_PLACEMENT_3D('',#42284,#26868,#26869);
#23710=AXIS2_PLACEMENT_3D('',#42287,#26871,#26872);
#23711=AXIS2_PLACEMENT_3D('',#42288,#26873,#26874);
#23712=AXIS2_PLACEMENT_3D('',#42290,#26876,#26877);
#23713=AXIS2_PLACEMENT_3D('',#42292,#26879,#26880);
#23714=AXIS2_PLACEMENT_3D('',#42294,#26881,#26882);
#23715=AXIS2_PLACEMENT_3D('',#42296,#26884,#26885);
#23716=AXIS2_PLACEMENT_3D('',#42298,#26886,#26887);
#23717=AXIS2_PLACEMENT_3D('',#42300,#26889,#26890);
#23718=AXIS2_PLACEMENT_3D('',#42301,#26891,#26892);
#23719=AXIS2_PLACEMENT_3D('',#42302,#26893,#26894);
#23720=AXIS2_PLACEMENT_3D('',#42303,#26895,#26896);
#23721=AXIS2_PLACEMENT_3D('',#42304,#26897,#26898);
#23722=AXIS2_PLACEMENT_3D('',#42313,#26903,#26904);
#23723=AXIS2_PLACEMENT_3D('',#42319,#26908,#26909);
#23724=AXIS2_PLACEMENT_3D('',#42325,#26913,#26914);
#23725=AXIS2_PLACEMENT_3D('',#42331,#26918,#26919);
#23726=AXIS2_PLACEMENT_3D('',#42333,#26920,#26921);
#23727=AXIS2_PLACEMENT_3D('',#42336,#26923,#26924);
#23728=AXIS2_PLACEMENT_3D('',#42337,#26925,#26926);
#23729=AXIS2_PLACEMENT_3D('',#42343,#26930,#26931);
#23730=AXIS2_PLACEMENT_3D('',#42344,#26932,#26933);
#23731=AXIS2_PLACEMENT_3D('',#42345,#26934,#26935);
#23732=AXIS2_PLACEMENT_3D('',#42346,#26936,#26937);
#23733=AXIS2_PLACEMENT_3D('',#42347,#26938,#26939);
#23734=AXIS2_PLACEMENT_3D('',#42349,#26940,#26941);
#23735=AXIS2_PLACEMENT_3D('',#42353,#26943,#26944);
#23736=AXIS2_PLACEMENT_3D('',#42354,#26945,#26946);
#23737=AXIS2_PLACEMENT_3D('',#42355,#26947,#26948);
#23738=AXIS2_PLACEMENT_3D('',#42357,#26949,#26950);
#23739=AXIS2_PLACEMENT_3D('',#42358,#26951,#26952);
#23740=AXIS2_PLACEMENT_3D('',#42361,#26954,#26955);
#23741=AXIS2_PLACEMENT_3D('',#42362,#26956,#26957);
#23742=AXIS2_PLACEMENT_3D('',#42364,#26958,#26959);
#23743=AXIS2_PLACEMENT_3D('',#42368,#26961,#26962);
#23744=AXIS2_PLACEMENT_3D('',#42369,#26963,#26964);
#23745=AXIS2_PLACEMENT_3D('',#42370,#26965,#26966);
#23746=AXIS2_PLACEMENT_3D('',#42372,#26967,#26968);
#23747=AXIS2_PLACEMENT_3D('',#42373,#26969,#26970);
#23748=AXIS2_PLACEMENT_3D('',#42376,#26972,#26973);
#23749=AXIS2_PLACEMENT_3D('',#42377,#26974,#26975);
#23750=AXIS2_PLACEMENT_3D('',#42379,#26976,#26977);
#23751=AXIS2_PLACEMENT_3D('',#42383,#26979,#26980);
#23752=AXIS2_PLACEMENT_3D('',#42384,#26981,#26982);
#23753=AXIS2_PLACEMENT_3D('',#42385,#26983,#26984);
#23754=AXIS2_PLACEMENT_3D('',#42387,#26985,#26986);
#23755=AXIS2_PLACEMENT_3D('',#42388,#26987,#26988);
#23756=AXIS2_PLACEMENT_3D('',#42391,#26990,#26991);
#23757=AXIS2_PLACEMENT_3D('',#42392,#26992,#26993);
#23758=AXIS2_PLACEMENT_3D('',#42394,#26994,#26995);
#23759=AXIS2_PLACEMENT_3D('',#42398,#26997,#26998);
#23760=AXIS2_PLACEMENT_3D('',#42399,#26999,#27000);
#23761=AXIS2_PLACEMENT_3D('',#42400,#27001,#27002);
#23762=AXIS2_PLACEMENT_3D('',#42402,#27003,#27004);
#23763=AXIS2_PLACEMENT_3D('',#42403,#27005,#27006);
#23764=AXIS2_PLACEMENT_3D('',#42406,#27008,#27009);
#23765=AXIS2_PLACEMENT_3D('',#42407,#27010,#27011);
#23766=AXIS2_PLACEMENT_3D('',#42409,#27012,#27013);
#23767=AXIS2_PLACEMENT_3D('',#42413,#27015,#27016);
#23768=AXIS2_PLACEMENT_3D('',#42414,#27017,#27018);
#23769=AXIS2_PLACEMENT_3D('',#42415,#27019,#27020);
#23770=AXIS2_PLACEMENT_3D('',#42417,#27021,#27022);
#23771=AXIS2_PLACEMENT_3D('',#42418,#27023,#27024);
#23772=AXIS2_PLACEMENT_3D('',#42421,#27026,#27027);
#23773=AXIS2_PLACEMENT_3D('',#42422,#27028,#27029);
#23774=AXIS2_PLACEMENT_3D('',#42424,#27030,#27031);
#23775=AXIS2_PLACEMENT_3D('',#42428,#27033,#27034);
#23776=AXIS2_PLACEMENT_3D('',#42429,#27035,#27036);
#23777=AXIS2_PLACEMENT_3D('',#42430,#27037,#27038);
#23778=AXIS2_PLACEMENT_3D('',#42432,#27039,#27040);
#23779=AXIS2_PLACEMENT_3D('',#42433,#27041,#27042);
#23780=AXIS2_PLACEMENT_3D('',#42436,#27044,#27045);
#23781=AXIS2_PLACEMENT_3D('',#42437,#27046,#27047);
#23782=AXIS2_PLACEMENT_3D('',#42440,#27048,#27049);
#23783=AXIS2_PLACEMENT_3D('',#42458,#27050,#27051);
#23784=AXIS2_PLACEMENT_3D('',#42460,#27053,#27054);
#23785=AXIS2_PLACEMENT_3D('',#42462,#27055,#27056);
#23786=AXIS2_PLACEMENT_3D('',#42464,#27057,#27058);
#23787=AXIS2_PLACEMENT_3D('',#42477,#27059,#27060);
#23788=AXIS2_PLACEMENT_3D('',#42496,#27061,#27062);
#23789=AXIS2_PLACEMENT_3D('',#42515,#27063,#27064);
#23790=AXIS2_PLACEMENT_3D('',#42538,#27065,#27066);
#23791=AXIS2_PLACEMENT_3D('',#42540,#27067,#27068);
#23792=AXIS2_PLACEMENT_3D('',#42559,#27069,#27070);
#23793=AXIS2_PLACEMENT_3D('',#42570,#27071,#27072);
#23794=AXIS2_PLACEMENT_3D('',#42572,#27073,#27074);
#23795=AXIS2_PLACEMENT_3D('',#42574,#27076,#27077);
#23796=AXIS2_PLACEMENT_3D('',#42575,#27078,#27079);
#23797=AXIS2_PLACEMENT_3D('',#42577,#27080,#27081);
#23798=AXIS2_PLACEMENT_3D('',#42578,#27082,#27083);
#23799=AXIS2_PLACEMENT_3D('',#42580,#27084,#27085);
#23800=AXIS2_PLACEMENT_3D('',#42581,#27086,#27087);
#23801=AXIS2_PLACEMENT_3D('',#42583,#27088,#27089);
#23802=AXIS2_PLACEMENT_3D('',#42584,#27090,#27091);
#23803=AXIS2_PLACEMENT_3D('',#42586,#27092,#27093);
#23804=AXIS2_PLACEMENT_3D('',#42587,#27094,#27095);
#23805=AXIS2_PLACEMENT_3D('',#42588,#27096,#27097);
#23806=AXIS2_PLACEMENT_3D('',#42590,#27099,#27100);
#23807=AXIS2_PLACEMENT_3D('',#42592,#27102,#27103);
#23808=AXIS2_PLACEMENT_3D('',#42594,#27105,#27106);
#23809=AXIS2_PLACEMENT_3D('',#42596,#27108,#27109);
#23810=AXIS2_PLACEMENT_3D('',#42598,#27110,#27111);
#23811=AXIS2_PLACEMENT_3D('',#42601,#27113,#27114);
#23812=AXIS2_PLACEMENT_3D('',#42602,#27115,#27116);
#23813=AXIS2_PLACEMENT_3D('',#42642,#27118,#27119);
#23814=AXIS2_PLACEMENT_3D('',#42644,#27120,#27121);
#23815=AXIS2_PLACEMENT_3D('',#42645,#27122,#27123);
#23816=AXIS2_PLACEMENT_3D('',#42648,#27125,#27126);
#23817=AXIS2_PLACEMENT_3D('',#42649,#27127,#27128);
#23818=AXIS2_PLACEMENT_3D('',#42689,#27130,#27131);
#23819=AXIS2_PLACEMENT_3D('',#42692,#27132,#27133);
#23820=AXIS2_PLACEMENT_3D('',#42693,#27134,#27135);
#23821=AXIS2_PLACEMENT_3D('',#42696,#27137,#27138);
#23822=AXIS2_PLACEMENT_3D('',#42697,#27139,#27140);
#23823=AXIS2_PLACEMENT_3D('',#42699,#27141,#27142);
#23824=AXIS2_PLACEMENT_3D('',#42700,#27143,#27144);
#23825=AXIS2_PLACEMENT_3D('',#42703,#27146,#27147);
#23826=AXIS2_PLACEMENT_3D('',#42704,#27148,#27149);
#23827=AXIS2_PLACEMENT_3D('',#42706,#27150,#27151);
#23828=AXIS2_PLACEMENT_3D('',#42710,#27153,#27154);
#23829=AXIS2_PLACEMENT_3D('',#42711,#27155,#27156);
#23830=AXIS2_PLACEMENT_3D('',#42712,#27157,#27158);
#23831=AXIS2_PLACEMENT_3D('',#42714,#27159,#27160);
#23832=AXIS2_PLACEMENT_3D('',#42716,#27162,#27163);
#23833=AXIS2_PLACEMENT_3D('',#42718,#27164,#27165);
#23834=AXIS2_PLACEMENT_3D('',#42719,#27166,#27167);
#23835=AXIS2_PLACEMENT_3D('',#42721,#27168,#27169);
#23836=AXIS2_PLACEMENT_3D('',#42723,#27170,#27171);
#23837=AXIS2_PLACEMENT_3D('',#42724,#27172,#27173);
#23838=AXIS2_PLACEMENT_3D('',#42725,#27174,#27175);
#23839=AXIS2_PLACEMENT_3D('',#42727,#27177,#27178);
#23840=AXIS2_PLACEMENT_3D('',#42730,#27180,#27181);
#23841=AXIS2_PLACEMENT_3D('',#42731,#27182,#27183);
#23842=AXIS2_PLACEMENT_3D('',#42733,#27184,#27185);
#23843=AXIS2_PLACEMENT_3D('',#42735,#27187,#27188);
#23844=AXIS2_PLACEMENT_3D('',#42737,#27190,#27191);
#23845=AXIS2_PLACEMENT_3D('',#42739,#27192,#27193);
#23846=AXIS2_PLACEMENT_3D('',#42741,#27195,#27196);
#23847=AXIS2_PLACEMENT_3D('',#42743,#27197,#27198);
#23848=AXIS2_PLACEMENT_3D('',#42745,#27200,#27201);
#23849=AXIS2_PLACEMENT_3D('',#42747,#27203,#27204);
#23850=AXIS2_PLACEMENT_3D('',#42749,#27205,#27206);
#23851=AXIS2_PLACEMENT_3D('',#42750,#27207,#27208);
#23852=AXIS2_PLACEMENT_3D('',#42753,#27210,#27211);
#23853=AXIS2_PLACEMENT_3D('',#42754,#27212,#27213);
#23854=AXIS2_PLACEMENT_3D('',#42756,#27214,#27215);
#23855=AXIS2_PLACEMENT_3D('',#42757,#27216,#27217);
#23856=AXIS2_PLACEMENT_3D('',#42760,#27219,#27220);
#23857=AXIS2_PLACEMENT_3D('',#42761,#27221,#27222);
#23858=AXIS2_PLACEMENT_3D('',#42763,#27223,#27224);
#23859=AXIS2_PLACEMENT_3D('',#42764,#27225,#27226);
#23860=AXIS2_PLACEMENT_3D('',#42767,#27228,#27229);
#23861=AXIS2_PLACEMENT_3D('',#42768,#27230,#27231);
#23862=AXIS2_PLACEMENT_3D('',#42770,#27232,#27233);
#23863=AXIS2_PLACEMENT_3D('',#42771,#27234,#27235);
#23864=AXIS2_PLACEMENT_3D('',#42774,#27237,#27238);
#23865=AXIS2_PLACEMENT_3D('',#42775,#27239,#27240);
#23866=AXIS2_PLACEMENT_3D('',#42776,#27241,#27242);
#23867=AXIS2_PLACEMENT_3D('',#42777,#27243,#27244);
#23868=AXIS2_PLACEMENT_3D('',#42779,#27245,#27246);
#23869=AXIS2_PLACEMENT_3D('',#42782,#27248,#27249);
#23870=AXIS2_PLACEMENT_3D('',#42783,#27250,#27251);
#23871=AXIS2_PLACEMENT_3D('',#42785,#27252,#27253);
#23872=AXIS2_PLACEMENT_3D('',#42787,#27255,#27256);
#23873=AXIS2_PLACEMENT_3D('',#42792,#27258,#27259);
#23874=AXIS2_PLACEMENT_3D('',#42795,#27261,#27262);
#23875=AXIS2_PLACEMENT_3D('',#42797,#27263,#27264);
#23876=AXIS2_PLACEMENT_3D('',#42799,#27265,#27266);
#23877=AXIS2_PLACEMENT_3D('',#42801,#27267,#27268);
#23878=AXIS2_PLACEMENT_3D('',#42803,#27269,#27270);
#23879=AXIS2_PLACEMENT_3D('',#42805,#27271,#27272);
#23880=AXIS2_PLACEMENT_3D('',#42807,#27273,#27274);
#23881=AXIS2_PLACEMENT_3D('',#42809,#27275,#27276);
#23882=AXIS2_PLACEMENT_3D('',#42810,#27277,#27278);
#23883=AXIS2_PLACEMENT_3D('',#42812,#27279,#27280);
#23884=AXIS2_PLACEMENT_3D('',#42814,#27282,#27283);
#23885=AXIS2_PLACEMENT_3D('',#42819,#27285,#27286);
#23886=AXIS2_PLACEMENT_3D('',#42822,#27288,#27289);
#23887=AXIS2_PLACEMENT_3D('',#42824,#27290,#27291);
#23888=AXIS2_PLACEMENT_3D('',#42826,#27292,#27293);
#23889=AXIS2_PLACEMENT_3D('',#42828,#27294,#27295);
#23890=AXIS2_PLACEMENT_3D('',#42831,#27296,#27297);
#23891=AXIS2_PLACEMENT_3D('',#42833,#27298,#27299);
#23892=AXIS2_PLACEMENT_3D('',#42835,#27300,#27301);
#23893=AXIS2_PLACEMENT_3D('',#42836,#27302,#27303);
#23894=AXIS2_PLACEMENT_3D('',#42839,#27304,#27305);
#23895=AXIS2_PLACEMENT_3D('',#42841,#27306,#27307);
#23896=AXIS2_PLACEMENT_3D('',#42843,#27308,#27309);
#23897=AXIS2_PLACEMENT_3D('',#42844,#27310,#27311);
#23898=AXIS2_PLACEMENT_3D('',#42846,#27312,#27313);
#23899=AXIS2_PLACEMENT_3D('',#42848,#27314,#27315);
#23900=AXIS2_PLACEMENT_3D('',#42850,#27316,#27317);
#23901=AXIS2_PLACEMENT_3D('',#42851,#27318,#27319);
#23902=AXIS2_PLACEMENT_3D('',#42854,#27321,#27322);
#23903=AXIS2_PLACEMENT_3D('',#42855,#27323,#27324);
#23904=AXIS2_PLACEMENT_3D('',#42857,#27325,#27326);
#23905=AXIS2_PLACEMENT_3D('',#42859,#27328,#27329);
#23906=AXIS2_PLACEMENT_3D('',#42861,#27331,#27332);
#23907=AXIS2_PLACEMENT_3D('',#42864,#27334,#27335);
#23908=AXIS2_PLACEMENT_3D('',#42865,#27336,#27337);
#23909=AXIS2_PLACEMENT_3D('',#42867,#27338,#27339);
#23910=AXIS2_PLACEMENT_3D('',#42869,#27341,#27342);
#23911=AXIS2_PLACEMENT_3D('',#42871,#27344,#27345);
#23912=AXIS2_PLACEMENT_3D('',#42874,#27347,#27348);
#23913=AXIS2_PLACEMENT_3D('',#42875,#27349,#27350);
#23914=AXIS2_PLACEMENT_3D('',#42877,#27351,#27352);
#23915=AXIS2_PLACEMENT_3D('',#42879,#27354,#27355);
#23916=AXIS2_PLACEMENT_3D('',#42881,#27357,#27358);
#23917=AXIS2_PLACEMENT_3D('',#42884,#27360,#27361);
#23918=AXIS2_PLACEMENT_3D('',#42885,#27362,#27363);
#23919=AXIS2_PLACEMENT_3D('',#42887,#27364,#27365);
#23920=AXIS2_PLACEMENT_3D('',#42889,#27367,#27368);
#23921=AXIS2_PLACEMENT_3D('',#42891,#27370,#27371);
#23922=AXIS2_PLACEMENT_3D('',#42894,#27373,#27374);
#23923=AXIS2_PLACEMENT_3D('',#42895,#27375,#27376);
#23924=AXIS2_PLACEMENT_3D('',#42897,#27377,#27378);
#23925=AXIS2_PLACEMENT_3D('',#42899,#27380,#27381);
#23926=AXIS2_PLACEMENT_3D('',#42901,#27383,#27384);
#23927=AXIS2_PLACEMENT_3D('',#42941,#27386,#27387);
#23928=AXIS2_PLACEMENT_3D('',#42943,#27388,#27389);
#23929=AXIS2_PLACEMENT_3D('',#42946,#27391,#27392);
#23930=AXIS2_PLACEMENT_3D('',#42947,#27393,#27394);
#23931=AXIS2_PLACEMENT_3D('',#42949,#27395,#27396);
#23932=AXIS2_PLACEMENT_3D('',#42951,#27398,#27399);
#23933=AXIS2_PLACEMENT_3D('',#42970,#27402,#27403);
#23934=AXIS2_PLACEMENT_3D('',#42972,#27404,#27405);
#23935=AXIS2_PLACEMENT_3D('',#42975,#27407,#27408);
#23936=AXIS2_PLACEMENT_3D('',#42976,#27409,#27410);
#23937=AXIS2_PLACEMENT_3D('',#42979,#27412,#27413);
#23938=AXIS2_PLACEMENT_3D('',#42980,#27414,#27415);
#23939=AXIS2_PLACEMENT_3D('',#42999,#27418,#27419);
#23940=AXIS2_PLACEMENT_3D('',#43001,#27420,#27421);
#23941=AXIS2_PLACEMENT_3D('',#43018,#27424,#27425);
#23942=AXIS2_PLACEMENT_3D('',#43031,#27427,#27428);
#23943=AXIS2_PLACEMENT_3D('',#43049,#27429,#27430);
#23944=AXIS2_PLACEMENT_3D('',#43050,#27431,#27432);
#23945=AXIS2_PLACEMENT_3D('',#43051,#27433,#27434);
#23946=AXIS2_PLACEMENT_3D('',#43052,#27435,#27436);
#23947=AXIS2_PLACEMENT_3D('',#43075,#27438,#27439);
#23948=AXIS2_PLACEMENT_3D('',#43077,#27440,#27441);
#23949=AXIS2_PLACEMENT_3D('',#43081,#27444,#27445);
#23950=AXIS2_PLACEMENT_3D('',#43082,#27446,#27447);
#23951=AXIS2_PLACEMENT_3D('',#43084,#27448,#27449);
#23952=AXIS2_PLACEMENT_3D('',#43085,#27450,#27451);
#23953=AXIS2_PLACEMENT_3D('',#43086,#27452,#27453);
#23954=AXIS2_PLACEMENT_3D('',#43087,#27454,#27455);
#23955=AXIS2_PLACEMENT_3D('',#43088,#27456,#27457);
#23956=AXIS2_PLACEMENT_3D('',#43089,#27458,#27459);
#23957=AXIS2_PLACEMENT_3D('',#43090,#27460,#27461);
#23958=AXIS2_PLACEMENT_3D('',#43091,#27462,#27463);
#23959=AXIS2_PLACEMENT_3D('',#43108,#27466,#27467);
#23960=AXIS2_PLACEMENT_3D('',#43122,#27469,#27470);
#23961=AXIS2_PLACEMENT_3D('',#43123,#27471,#27472);
#23962=AXIS2_PLACEMENT_3D('',#43141,#27473,#27474);
#23963=AXIS2_PLACEMENT_3D('',#43142,#27475,#27476);
#23964=AXIS2_PLACEMENT_3D('',#43143,#27477,#27478);
#23965=AXIS2_PLACEMENT_3D('',#43166,#27480,#27481);
#23966=AXIS2_PLACEMENT_3D('',#43167,#27482,#27483);
#23967=AXIS2_PLACEMENT_3D('',#43169,#27484,#27485);
#23968=AXIS2_PLACEMENT_3D('',#43173,#27488,#27489);
#23969=AXIS2_PLACEMENT_3D('',#43174,#27490,#27491);
#23970=AXIS2_PLACEMENT_3D('',#43176,#27492,#27493);
#23971=AXIS2_PLACEMENT_3D('',#43177,#27494,#27495);
#23972=AXIS2_PLACEMENT_3D('',#43178,#27496,#27497);
#23973=AXIS2_PLACEMENT_3D('',#43181,#27499,#27500);
#23974=AXIS2_PLACEMENT_3D('',#43182,#27501,#27502);
#23975=AXIS2_PLACEMENT_3D('',#43183,#27503,#27504);
#23976=AXIS2_PLACEMENT_3D('',#43185,#27506,#27507);
#23977=AXIS2_PLACEMENT_3D('',#43186,#27508,#27509);
#23978=AXIS2_PLACEMENT_3D('',#43187,#27510,#27511);
#23979=AXIS2_PLACEMENT_3D('',#43190,#27513,#27514);
#23980=AXIS2_PLACEMENT_3D('',#43191,#27515,#27516);
#23981=AXIS2_PLACEMENT_3D('',#43192,#27517,#27518);
#23982=AXIS2_PLACEMENT_3D('',#43194,#27520,#27521);
#23983=AXIS2_PLACEMENT_3D('',#43195,#27522,#27523);
#23984=AXIS2_PLACEMENT_3D('',#43196,#27524,#27525);
#23985=AXIS2_PLACEMENT_3D('',#43200,#27527,#27528);
#23986=AXIS2_PLACEMENT_3D('',#43201,#27529,#27530);
#23987=AXIS2_PLACEMENT_3D('',#43202,#27531,#27532);
#23988=AXIS2_PLACEMENT_3D('',#43205,#27533,#27534);
#23989=AXIS2_PLACEMENT_3D('',#43206,#27535,#27536);
#23990=AXIS2_PLACEMENT_3D('',#43208,#27538,#27539);
#23991=AXIS2_PLACEMENT_3D('',#43210,#27541,#27542);
#23992=AXIS2_PLACEMENT_3D('',#43211,#27543,#27544);
#23993=AXIS2_PLACEMENT_3D('',#43212,#27545,#27546);
#23994=AXIS2_PLACEMENT_3D('',#43213,#27547,#27548);
#23995=AXIS2_PLACEMENT_3D('',#43214,#27549,#27550);
#23996=AXIS2_PLACEMENT_3D('',#43215,#27551,#27552);
#23997=AXIS2_PLACEMENT_3D('',#43354,#27563,#27564);
#23998=AXIS2_PLACEMENT_3D('',#43390,#27570,#27571);
#23999=AXIS2_PLACEMENT_3D('',#43501,#27582,#27583);
#24000=AXIS2_PLACEMENT_3D('',#43732,#27602,#27603);
#24001=AXIS2_PLACEMENT_3D('',#43735,#27606,#27607);
#24002=AXIS2_PLACEMENT_3D('',#44036,#27628,#27629);
#24003=AXIS2_PLACEMENT_3D('',#44070,#27633,#27634);
#24004=AXIS2_PLACEMENT_3D('',#44106,#27640,#27641);
#24005=AXIS2_PLACEMENT_3D('',#44112,#27645,#27646);
#24006=AXIS2_PLACEMENT_3D('',#44118,#27650,#27651);
#24007=AXIS2_PLACEMENT_3D('',#44124,#27655,#27656);
#24008=AXIS2_PLACEMENT_3D('',#44127,#27659,#27660);
#24009=AXIS2_PLACEMENT_3D('',#44128,#27661,#27662);
#24010=AXIS2_PLACEMENT_3D('',#44137,#27667,#27668);
#24011=AXIS2_PLACEMENT_3D('',#44143,#27672,#27673);
#24012=AXIS2_PLACEMENT_3D('',#44149,#27677,#27678);
#24013=AXIS2_PLACEMENT_3D('',#44155,#27682,#27683);
#24014=AXIS2_PLACEMENT_3D('',#44161,#27687,#27688);
#24015=AXIS2_PLACEMENT_3D('',#44167,#27692,#27693);
#24016=AXIS2_PLACEMENT_3D('',#44173,#27697,#27698);
#24017=AXIS2_PLACEMENT_3D('',#44209,#27704,#27705);
#24018=AXIS2_PLACEMENT_3D('',#44215,#27709,#27710);
#24019=AXIS2_PLACEMENT_3D('',#44221,#27714,#27715);
#24020=AXIS2_PLACEMENT_3D('',#44227,#27719,#27720);
#24021=AXIS2_PLACEMENT_3D('',#44233,#27724,#27725);
#24022=AXIS2_PLACEMENT_3D('',#44236,#27728,#27729);
#24023=AXIS2_PLACEMENT_3D('',#44405,#27742,#27743);
#24024=AXIS2_PLACEMENT_3D('',#44516,#27754,#27755);
#24025=AXIS2_PLACEMENT_3D('',#44627,#27766,#27767);
#24026=AXIS2_PLACEMENT_3D('',#44660,#27772,#27773);
#24027=AXIS2_PLACEMENT_3D('',#44661,#27774,#27775);
#24028=AXIS2_PLACEMENT_3D('',#44670,#27780,#27781);
#24029=AXIS2_PLACEMENT_3D('',#44676,#27785,#27786);
#24030=AXIS2_PLACEMENT_3D('',#44682,#27790,#27791);
#24031=AXIS2_PLACEMENT_3D('',#44685,#27794,#27795);
#24032=AXIS2_PLACEMENT_3D('',#44719,#27799,#27800);
#24033=AXIS2_PLACEMENT_3D('',#44725,#27804,#27805);
#24034=AXIS2_PLACEMENT_3D('',#44731,#27809,#27810);
#24035=AXIS2_PLACEMENT_3D('',#44734,#27813,#27814);
#24036=AXIS2_PLACEMENT_3D('',#44743,#27819,#27820);
#24037=AXIS2_PLACEMENT_3D('',#44749,#27824,#27825);
#24038=AXIS2_PLACEMENT_3D('',#44755,#27829,#27830);
#24039=AXIS2_PLACEMENT_3D('',#44761,#27834,#27835);
#24040=AXIS2_PLACEMENT_3D('',#44767,#27839,#27840);
#24041=AXIS2_PLACEMENT_3D('',#44773,#27844,#27845);
#24042=AXIS2_PLACEMENT_3D('',#44779,#27849,#27850);
#24043=AXIS2_PLACEMENT_3D('',#44782,#27853,#27854);
#24044=AXIS2_PLACEMENT_3D('',#44981,#27869,#27870);
#24045=AXIS2_PLACEMENT_3D('',#45257,#27892,#27893);
#24046=AXIS2_PLACEMENT_3D('',#45290,#27898,#27899);
#24047=AXIS2_PLACEMENT_3D('',#45459,#27912,#27913);
#24048=AXIS2_PLACEMENT_3D('',#45570,#27924,#27925);
#24049=AXIS2_PLACEMENT_3D('',#45681,#27936,#27937);
#24050=AXIS2_PLACEMENT_3D('',#45714,#27942,#27943);
#24051=AXIS2_PLACEMENT_3D('',#45838,#27953,#27954);
#24052=AXIS2_PLACEMENT_3D('',#45979,#27967,#27968);
#24053=AXIS2_PLACEMENT_3D('',#45985,#27972,#27973);
#24054=AXIS2_PLACEMENT_3D('',#45991,#27977,#27978);
#24055=AXIS2_PLACEMENT_3D('',#46009,#27982,#27983);
#24056=AXIS2_PLACEMENT_3D('',#46010,#27984,#27985);
#24057=AXIS2_PLACEMENT_3D('',#46094,#27995,#27996);
#24058=AXIS2_PLACEMENT_3D('',#46100,#28000,#28001);
#24059=AXIS2_PLACEMENT_3D('',#46103,#28004,#28005);
#24060=AXIS2_PLACEMENT_3D('',#46202,#28016,#28017);
#24061=AXIS2_PLACEMENT_3D('',#46208,#28021,#28022);
#24062=AXIS2_PLACEMENT_3D('',#46214,#28026,#28027);
#24063=AXIS2_PLACEMENT_3D('',#46220,#28031,#28032);
#24064=AXIS2_PLACEMENT_3D('',#46223,#28035,#28036);
#24065=AXIS2_PLACEMENT_3D('',#46602,#28063,#28064);
#24066=AXIS2_PLACEMENT_3D('',#46635,#28069,#28070);
#24067=AXIS2_PLACEMENT_3D('',#46864,#28087,#28088);
#24068=AXIS2_PLACEMENT_3D('',#46870,#28092,#28093);
#24069=AXIS2_PLACEMENT_3D('',#46876,#28097,#28098);
#24070=AXIS2_PLACEMENT_3D('',#46882,#28102,#28103);
#24071=AXIS2_PLACEMENT_3D('',#46888,#28107,#28108);
#24072=AXIS2_PLACEMENT_3D('',#46906,#28112,#28113);
#24073=AXIS2_PLACEMENT_3D('',#46970,#28119,#28120);
#24074=AXIS2_PLACEMENT_3D('',#47021,#28127,#28128);
#24075=AXIS2_PLACEMENT_3D('',#47027,#28132,#28133);
#24076=AXIS2_PLACEMENT_3D('',#47033,#28137,#28138);
#24077=AXIS2_PLACEMENT_3D('',#47039,#28142,#28143);
#24078=AXIS2_PLACEMENT_3D('',#47045,#28147,#28148);
#24079=AXIS2_PLACEMENT_3D('',#47048,#28151,#28152);
#24080=AXIS2_PLACEMENT_3D('',#47049,#28153,#28154);
#24081=AXIS2_PLACEMENT_3D('',#47050,#28155,#28156);
#24082=AXIS2_PLACEMENT_3D('',#47051,#28157,#28158);
#24083=AXIS2_PLACEMENT_3D('',#47052,#28159,#28160);
#24084=AXIS2_PLACEMENT_3D('',#47053,#28161,#28162);
#24085=AXIS2_PLACEMENT_3D('',#47054,#28163,#28164);
#24086=AXIS2_PLACEMENT_3D('',#47055,#28165,#28166);
#24087=AXIS2_PLACEMENT_3D('',#47057,#28167,#28168);
#24088=AXIS2_PLACEMENT_3D('',#47103,#28170,#28171);
#24089=AXIS2_PLACEMENT_3D('',#47105,#28172,#28173);
#24090=AXIS2_PLACEMENT_3D('',#47108,#28175,#28176);
#24091=AXIS2_PLACEMENT_3D('',#47109,#28177,#28178);
#24092=AXIS2_PLACEMENT_3D('',#47111,#28179,#28180);
#24093=AXIS2_PLACEMENT_3D('',#47113,#28182,#28183);
#24094=AXIS2_PLACEMENT_3D('',#47147,#28187,#28188);
#24095=AXIS2_PLACEMENT_3D('',#47151,#28190,#28191);
#24096=AXIS2_PLACEMENT_3D('',#47152,#28192,#28193);
#24097=AXIS2_PLACEMENT_3D('',#47156,#28196,#28197);
#24098=AXIS2_PLACEMENT_3D('',#47157,#28198,#28199);
#24099=AXIS2_PLACEMENT_3D('',#47158,#28200,#28201);
#24100=AXIS2_PLACEMENT_3D('',#47159,#28202,#28203);
#24101=AXIS2_PLACEMENT_3D('',#47160,#28204,#28205);
#24102=AXIS2_PLACEMENT_3D('',#47162,#28206,#28207);
#24103=AXIS2_PLACEMENT_3D('',#47165,#28209,#28210);
#24104=AXIS2_PLACEMENT_3D('',#47166,#28211,#28212);
#24105=AXIS2_PLACEMENT_3D('',#47167,#28213,#28214);
#24106=AXIS2_PLACEMENT_3D('',#47169,#28215,#28216);
#24107=AXIS2_PLACEMENT_3D('',#47170,#28217,#28218);
#24108=AXIS2_PLACEMENT_3D('',#47171,#28219,#28220);
#24109=AXIS2_PLACEMENT_3D('',#47173,#28221,#28222);
#24110=AXIS2_PLACEMENT_3D('',#47176,#28224,#28225);
#24111=AXIS2_PLACEMENT_3D('',#47177,#28226,#28227);
#24112=AXIS2_PLACEMENT_3D('',#47179,#28228,#28229);
#24113=AXIS2_PLACEMENT_3D('',#47181,#28230,#28231);
#24114=AXIS2_PLACEMENT_3D('',#47183,#28232,#28233);
#24115=AXIS2_PLACEMENT_3D('',#47185,#28234,#28235);
#24116=AXIS2_PLACEMENT_3D('',#47187,#28236,#28237);
#24117=AXIS2_PLACEMENT_3D('',#47189,#28238,#28239);
#24118=AXIS2_PLACEMENT_3D('',#47191,#28240,#28241);
#24119=AXIS2_PLACEMENT_3D('',#47192,#28242,#28243);
#24120=AXIS2_PLACEMENT_3D('',#47195,#28245,#28246);
#24121=AXIS2_PLACEMENT_3D('',#47196,#28247,#28248);
#24122=AXIS2_PLACEMENT_3D('',#47199,#28250,#28251);
#24123=AXIS2_PLACEMENT_3D('',#47200,#28252,#28253);
#24124=AXIS2_PLACEMENT_3D('',#47203,#28255,#28256);
#24125=AXIS2_PLACEMENT_3D('',#47204,#28257,#28258);
#24126=AXIS2_PLACEMENT_3D('',#47207,#28260,#28261);
#24127=AXIS2_PLACEMENT_3D('',#47208,#28262,#28263);
#24128=AXIS2_PLACEMENT_3D('',#47211,#28265,#28266);
#24129=AXIS2_PLACEMENT_3D('',#47212,#28267,#28268);
#24130=AXIS2_PLACEMENT_3D('',#47215,#28270,#28271);
#24131=AXIS2_PLACEMENT_3D('',#47216,#28272,#28273);
#24132=AXIS2_PLACEMENT_3D('',#47219,#28275,#28276);
#24133=AXIS2_PLACEMENT_3D('',#47220,#28277,#28278);
#24134=AXIS2_PLACEMENT_3D('',#47223,#28280,#28281);
#24135=AXIS2_PLACEMENT_3D('',#47224,#28282,#28283);
#24136=AXIS2_PLACEMENT_3D('',#47227,#28285,#28286);
#24137=AXIS2_PLACEMENT_3D('',#47228,#28287,#28288);
#24138=AXIS2_PLACEMENT_3D('',#47231,#28290,#28291);
#24139=AXIS2_PLACEMENT_3D('',#47232,#28292,#28293);
#24140=AXIS2_PLACEMENT_3D('',#47235,#28295,#28296);
#24141=AXIS2_PLACEMENT_3D('',#47236,#28297,#28298);
#24142=AXIS2_PLACEMENT_3D('',#47239,#28300,#28301);
#24143=AXIS2_PLACEMENT_3D('',#47242,#28303,#28304);
#24144=AXIS2_PLACEMENT_3D('',#47245,#28306,#28307);
#24145=AXIS2_PLACEMENT_3D('',#47248,#28309,#28310);
#24146=AXIS2_PLACEMENT_3D('',#47251,#28312,#28313);
#24147=AXIS2_PLACEMENT_3D('',#47254,#28315,#28316);
#24148=AXIS2_PLACEMENT_3D('',#47258,#28318,#28319);
#24149=AXIS2_PLACEMENT_3D('',#47259,#28320,#28321);
#24150=AXIS2_PLACEMENT_3D('',#47260,#28322,#28323);
#24151=AXIS2_PLACEMENT_3D('',#47262,#28324,#28325);
#24152=AXIS2_PLACEMENT_3D('',#47264,#28327,#28328);
#24153=AXIS2_PLACEMENT_3D('',#47265,#28329,#28330);
#24154=AXIS2_PLACEMENT_3D('',#47267,#28332,#28333);
#24155=AXIS2_PLACEMENT_3D('',#47269,#28334,#28335);
#24156=AXIS2_PLACEMENT_3D('',#47270,#28336,#28337);
#24157=AXIS2_PLACEMENT_3D('',#47273,#28339,#28340);
#24158=AXIS2_PLACEMENT_3D('',#47274,#28341,#28342);
#24159=AXIS2_PLACEMENT_3D('',#47275,#28343,#28344);
#24160=AXIS2_PLACEMENT_3D('',#47276,#28345,#28346);
#24161=AXIS2_PLACEMENT_3D('',#47278,#28347,#28348);
#24162=AXIS2_PLACEMENT_3D('',#47280,#28349,#28350);
#24163=AXIS2_PLACEMENT_3D('',#47281,#28351,#28352);
#24164=AXIS2_PLACEMENT_3D('',#47283,#28353,#28354);
#24165=AXIS2_PLACEMENT_3D('',#47285,#28356,#28357);
#24166=AXIS2_PLACEMENT_3D('',#47287,#28358,#28359);
#24167=AXIS2_PLACEMENT_3D('',#47288,#28360,#28361);
#24168=AXIS2_PLACEMENT_3D('',#47291,#28363,#28364);
#24169=AXIS2_PLACEMENT_3D('',#47292,#28365,#28366);
#24170=AXIS2_PLACEMENT_3D('',#47294,#28367,#28368);
#24171=AXIS2_PLACEMENT_3D('',#47295,#28369,#28370);
#24172=AXIS2_PLACEMENT_3D('',#47297,#28371,#28372);
#24173=AXIS2_PLACEMENT_3D('',#47299,#28374,#28375);
#24174=AXIS2_PLACEMENT_3D('',#47301,#28376,#28377);
#24175=AXIS2_PLACEMENT_3D('',#47302,#28378,#28379);
#24176=AXIS2_PLACEMENT_3D('',#47305,#28381,#28382);
#24177=AXIS2_PLACEMENT_3D('',#47306,#28383,#28384);
#24178=AXIS2_PLACEMENT_3D('',#47308,#28385,#28386);
#24179=AXIS2_PLACEMENT_3D('',#47311,#28388,#28389);
#24180=AXIS2_PLACEMENT_3D('',#47312,#28390,#28391);
#24181=AXIS2_PLACEMENT_3D('',#47314,#28392,#28393);
#24182=AXIS2_PLACEMENT_3D('',#47316,#28395,#28396);
#24183=AXIS2_PLACEMENT_3D('',#47318,#28398,#28399);
#24184=AXIS2_PLACEMENT_3D('',#47320,#28400,#28401);
#24185=AXIS2_PLACEMENT_3D('',#47322,#28403,#28404);
#24186=AXIS2_PLACEMENT_3D('',#47324,#28405,#28406);
#24187=AXIS2_PLACEMENT_3D('',#47326,#28408,#28409);
#24188=AXIS2_PLACEMENT_3D('',#47328,#28410,#28411);
#24189=AXIS2_PLACEMENT_3D('',#47329,#28412,#28413);
#24190=AXIS2_PLACEMENT_3D('',#47332,#28415,#28416);
#24191=AXIS2_PLACEMENT_3D('',#47333,#28417,#28418);
#24192=AXIS2_PLACEMENT_3D('',#47336,#28420,#28421);
#24193=AXIS2_PLACEMENT_3D('',#47337,#28422,#28423);
#24194=AXIS2_PLACEMENT_3D('',#47340,#28425,#28426);
#24195=AXIS2_PLACEMENT_3D('',#47341,#28427,#28428);
#24196=AXIS2_PLACEMENT_3D('',#47342,#28429,#28430);
#24197=AXIS2_PLACEMENT_3D('',#47343,#28431,#28432);
#24198=AXIS2_PLACEMENT_3D('',#47344,#28433,#28434);
#24199=AXIS2_PLACEMENT_3D('',#47346,#28435,#28436);
#24200=AXIS2_PLACEMENT_3D('',#47349,#28438,#28439);
#24201=AXIS2_PLACEMENT_3D('',#47350,#28440,#28441);
#24202=AXIS2_PLACEMENT_3D('',#47352,#28442,#28443);
#24203=AXIS2_PLACEMENT_3D('',#47355,#28445,#28446);
#24204=AXIS2_PLACEMENT_3D('',#47356,#28447,#28448);
#24205=AXIS2_PLACEMENT_3D('',#47357,#28449,#28450);
#24206=AXIS2_PLACEMENT_3D('',#47359,#28451,#28452);
#24207=AXIS2_PLACEMENT_3D('',#47360,#28453,#28454);
#24208=AXIS2_PLACEMENT_3D('',#47362,#28455,#28456);
#24209=AXIS2_PLACEMENT_3D('',#47364,#28457,#28458);
#24210=AXIS2_PLACEMENT_3D('',#47365,#28459,#28460);
#24211=AXIS2_PLACEMENT_3D('',#47366,#28461,#28462);
#24212=AXIS2_PLACEMENT_3D('',#47369,#28464,#28465);
#24213=AXIS2_PLACEMENT_3D('',#47370,#28466,#28467);
#24214=AXIS2_PLACEMENT_3D('',#47372,#28468,#28469);
#24215=AXIS2_PLACEMENT_3D('',#47373,#28470,#28471);
#24216=AXIS2_PLACEMENT_3D('',#47376,#28473,#28474);
#24217=AXIS2_PLACEMENT_3D('',#47377,#28475,#28476);
#24218=AXIS2_PLACEMENT_3D('',#47378,#28477,#28478);
#24219=AXIS2_PLACEMENT_3D('',#47380,#28479,#28480);
#24220=AXIS2_PLACEMENT_3D('',#47382,#28482,#28483);
#24221=AXIS2_PLACEMENT_3D('',#47384,#28484,#28485);
#24222=AXIS2_PLACEMENT_3D('',#47386,#28487,#28488);
#24223=AXIS2_PLACEMENT_3D('',#47388,#28489,#28490);
#24224=AXIS2_PLACEMENT_3D('',#47390,#28492,#28493);
#24225=AXIS2_PLACEMENT_3D('',#47392,#28494,#28495);
#24226=AXIS2_PLACEMENT_3D('',#47393,#28496,#28497);
#24227=AXIS2_PLACEMENT_3D('',#47395,#28498,#28499);
#24228=AXIS2_PLACEMENT_3D('',#47397,#28501,#28502);
#24229=AXIS2_PLACEMENT_3D('',#47399,#28503,#28504);
#24230=AXIS2_PLACEMENT_3D('',#47401,#28506,#28507);
#24231=AXIS2_PLACEMENT_3D('',#47402,#28508,#28509);
#24232=AXIS2_PLACEMENT_3D('',#47403,#28510,#28511);
#24233=AXIS2_PLACEMENT_3D('',#47405,#28512,#28513);
#24234=AXIS2_PLACEMENT_3D('',#47408,#28515,#28516);
#24235=AXIS2_PLACEMENT_3D('',#47411,#28517,#28518);
#24236=AXIS2_PLACEMENT_3D('',#47418,#28519,#28520);
#24237=AXIS2_PLACEMENT_3D('',#47425,#28521,#28522);
#24238=AXIS2_PLACEMENT_3D('',#47432,#28523,#28524);
#24239=AXIS2_PLACEMENT_3D('',#47439,#28525,#28526);
#24240=AXIS2_PLACEMENT_3D('',#47446,#28527,#28528);
#24241=AXIS2_PLACEMENT_3D('',#47453,#28529,#28530);
#24242=AXIS2_PLACEMENT_3D('',#47460,#28531,#28532);
#24243=AXIS2_PLACEMENT_3D('',#47467,#28533,#28534);
#24244=AXIS2_PLACEMENT_3D('',#47474,#28535,#28536);
#24245=AXIS2_PLACEMENT_3D('',#47481,#28537,#28538);
#24246=AXIS2_PLACEMENT_3D('',#47488,#28539,#28540);
#24247=AXIS2_PLACEMENT_3D('',#47495,#28541,#28542);
#24248=AXIS2_PLACEMENT_3D('',#47502,#28543,#28544);
#24249=AXIS2_PLACEMENT_3D('',#47509,#28545,#28546);
#24250=AXIS2_PLACEMENT_3D('',#47516,#28547,#28548);
#24251=AXIS2_PLACEMENT_3D('',#47523,#28549,#28550);
#24252=AXIS2_PLACEMENT_3D('',#47530,#28551,#28552);
#24253=AXIS2_PLACEMENT_3D('',#47537,#28553,#28554);
#24254=AXIS2_PLACEMENT_3D('',#47544,#28555,#28556);
#24255=AXIS2_PLACEMENT_3D('',#47551,#28557,#28558);
#24256=AXIS2_PLACEMENT_3D('',#47558,#28559,#28560);
#24257=AXIS2_PLACEMENT_3D('',#47565,#28561,#28562);
#24258=AXIS2_PLACEMENT_3D('',#47572,#28563,#28564);
#24259=AXIS2_PLACEMENT_3D('',#47579,#28565,#28566);
#24260=AXIS2_PLACEMENT_3D('',#47586,#28567,#28568);
#24261=AXIS2_PLACEMENT_3D('',#47593,#28569,#28570);
#24262=AXIS2_PLACEMENT_3D('',#47600,#28571,#28572);
#24263=AXIS2_PLACEMENT_3D('',#47607,#28573,#28574);
#24264=AXIS2_PLACEMENT_3D('',#47614,#28575,#28576);
#24265=AXIS2_PLACEMENT_3D('',#47621,#28577,#28578);
#24266=AXIS2_PLACEMENT_3D('',#47628,#28579,#28580);
#24267=AXIS2_PLACEMENT_3D('',#47640,#28581,#28582);
#24268=AXIS2_PLACEMENT_3D('',#47646,#28583,#28584);
#24269=AXIS2_PLACEMENT_3D('',#47647,#28585,#28586);
#24270=AXIS2_PLACEMENT_3D('',#47649,#28587,#28588);
#24271=AXIS2_PLACEMENT_3D('',#47652,#28590,#28591);
#24272=AXIS2_PLACEMENT_3D('',#47655,#28592,#28593);
#24273=AXIS2_PLACEMENT_3D('',#47662,#28594,#28595);
#24274=AXIS2_PLACEMENT_3D('',#47669,#28596,#28597);
#24275=AXIS2_PLACEMENT_3D('',#47676,#28598,#28599);
#24276=AXIS2_PLACEMENT_3D('',#47683,#28600,#28601);
#24277=AXIS2_PLACEMENT_3D('',#47690,#28602,#28603);
#24278=AXIS2_PLACEMENT_3D('',#47697,#28604,#28605);
#24279=AXIS2_PLACEMENT_3D('',#47704,#28606,#28607);
#24280=AXIS2_PLACEMENT_3D('',#47711,#28608,#28609);
#24281=AXIS2_PLACEMENT_3D('',#47718,#28610,#28611);
#24282=AXIS2_PLACEMENT_3D('',#47725,#28612,#28613);
#24283=AXIS2_PLACEMENT_3D('',#47732,#28614,#28615);
#24284=AXIS2_PLACEMENT_3D('',#47739,#28616,#28617);
#24285=AXIS2_PLACEMENT_3D('',#47746,#28618,#28619);
#24286=AXIS2_PLACEMENT_3D('',#47753,#28620,#28621);
#24287=AXIS2_PLACEMENT_3D('',#47760,#28622,#28623);
#24288=AXIS2_PLACEMENT_3D('',#47767,#28624,#28625);
#24289=AXIS2_PLACEMENT_3D('',#47774,#28626,#28627);
#24290=AXIS2_PLACEMENT_3D('',#47781,#28628,#28629);
#24291=AXIS2_PLACEMENT_3D('',#47788,#28630,#28631);
#24292=AXIS2_PLACEMENT_3D('',#47795,#28632,#28633);
#24293=AXIS2_PLACEMENT_3D('',#47802,#28634,#28635);
#24294=AXIS2_PLACEMENT_3D('',#47809,#28636,#28637);
#24295=AXIS2_PLACEMENT_3D('',#47816,#28638,#28639);
#24296=AXIS2_PLACEMENT_3D('',#47823,#28640,#28641);
#24297=AXIS2_PLACEMENT_3D('',#47830,#28642,#28643);
#24298=AXIS2_PLACEMENT_3D('',#47837,#28644,#28645);
#24299=AXIS2_PLACEMENT_3D('',#47844,#28646,#28647);
#24300=AXIS2_PLACEMENT_3D('',#47851,#28648,#28649);
#24301=AXIS2_PLACEMENT_3D('',#47858,#28650,#28651);
#24302=AXIS2_PLACEMENT_3D('',#47865,#28652,#28653);
#24303=AXIS2_PLACEMENT_3D('',#47872,#28654,#28655);
#24304=AXIS2_PLACEMENT_3D('',#47884,#28656,#28657);
#24305=AXIS2_PLACEMENT_3D('',#47890,#28658,#28659);
#24306=AXIS2_PLACEMENT_3D('',#47891,#28660,#28661);
#24307=AXIS2_PLACEMENT_3D('',#47893,#28663,#28664);
#24308=AXIS2_PLACEMENT_3D('',#47895,#28666,#28667);
#24309=AXIS2_PLACEMENT_3D('',#47896,#28668,#28669);
#24310=AXIS2_PLACEMENT_3D('',#47897,#28670,#28671);
#24311=AXIS2_PLACEMENT_3D('',#47899,#28672,#28673);
#24312=AXIS2_PLACEMENT_3D('',#47901,#28674,#28675);
#24313=AXIS2_PLACEMENT_3D('',#47902,#28676,#28677);
#24314=AXIS2_PLACEMENT_3D('',#47903,#28678,#28679);
#24315=AXIS2_PLACEMENT_3D('',#47904,#28680,#28681);
#24316=AXIS2_PLACEMENT_3D('',#47905,#28682,#28683);
#24317=AXIS2_PLACEMENT_3D('',#47907,#28684,#28685);
#24318=AXIS2_PLACEMENT_3D('',#47909,#28686,#28687);
#24319=AXIS2_PLACEMENT_3D('',#47914,#28688,#28689);
#24320=AXIS2_PLACEMENT_3D('',#47915,#28690,#28691);
#24321=AXIS2_PLACEMENT_3D('',#47916,#28692,#28693);
#24322=AXIS2_PLACEMENT_3D('',#47917,#28694,#28695);
#24323=AXIS2_PLACEMENT_3D('',#47919,#28696,#28697);
#24324=AXIS2_PLACEMENT_3D('',#47921,#28698,#28699);
#24325=AXIS2_PLACEMENT_3D('',#47922,#28700,#28701);
#24326=AXIS2_PLACEMENT_3D('',#47923,#28702,#28703);
#24327=AXIS2_PLACEMENT_3D('',#47924,#28704,#28705);
#24328=AXIS2_PLACEMENT_3D('',#47925,#28706,#28707);
#24329=AXIS2_PLACEMENT_3D('',#47927,#28708,#28709);
#24330=AXIS2_PLACEMENT_3D('',#47929,#28710,#28711);
#24331=AXIS2_PLACEMENT_3D('',#47934,#28712,#28713);
#24332=AXIS2_PLACEMENT_3D('',#47935,#28714,#28715);
#24333=AXIS2_PLACEMENT_3D('',#47936,#28716,#28717);
#24334=AXIS2_PLACEMENT_3D('',#47937,#28718,#28719);
#24335=AXIS2_PLACEMENT_3D('',#47939,#28720,#28721);
#24336=AXIS2_PLACEMENT_3D('',#47941,#28722,#28723);
#24337=AXIS2_PLACEMENT_3D('',#47942,#28724,#28725);
#24338=AXIS2_PLACEMENT_3D('',#47943,#28726,#28727);
#24339=AXIS2_PLACEMENT_3D('',#47944,#28728,#28729);
#24340=AXIS2_PLACEMENT_3D('',#47945,#28730,#28731);
#24341=AXIS2_PLACEMENT_3D('',#47947,#28732,#28733);
#24342=AXIS2_PLACEMENT_3D('',#47949,#28734,#28735);
#24343=AXIS2_PLACEMENT_3D('',#47954,#28736,#28737);
#24344=AXIS2_PLACEMENT_3D('',#47955,#28738,#28739);
#24345=AXIS2_PLACEMENT_3D('',#47956,#28740,#28741);
#24346=AXIS2_PLACEMENT_3D('',#47957,#28742,#28743);
#24347=AXIS2_PLACEMENT_3D('',#47959,#28744,#28745);
#24348=AXIS2_PLACEMENT_3D('',#47961,#28746,#28747);
#24349=AXIS2_PLACEMENT_3D('',#47962,#28748,#28749);
#24350=AXIS2_PLACEMENT_3D('',#47963,#28750,#28751);
#24351=AXIS2_PLACEMENT_3D('',#47964,#28752,#28753);
#24352=AXIS2_PLACEMENT_3D('',#47965,#28754,#28755);
#24353=AXIS2_PLACEMENT_3D('',#47967,#28756,#28757);
#24354=AXIS2_PLACEMENT_3D('',#47969,#28758,#28759);
#24355=AXIS2_PLACEMENT_3D('',#47974,#28760,#28761);
#24356=AXIS2_PLACEMENT_3D('',#47975,#28762,#28763);
#24357=AXIS2_PLACEMENT_3D('',#47976,#28764,#28765);
#24358=AXIS2_PLACEMENT_3D('',#47977,#28766,#28767);
#24359=AXIS2_PLACEMENT_3D('',#47979,#28768,#28769);
#24360=AXIS2_PLACEMENT_3D('',#47981,#28770,#28771);
#24361=AXIS2_PLACEMENT_3D('',#47982,#28772,#28773);
#24362=AXIS2_PLACEMENT_3D('',#47983,#28774,#28775);
#24363=AXIS2_PLACEMENT_3D('',#47984,#28776,#28777);
#24364=AXIS2_PLACEMENT_3D('',#47985,#28778,#28779);
#24365=AXIS2_PLACEMENT_3D('',#47987,#28780,#28781);
#24366=AXIS2_PLACEMENT_3D('',#47989,#28782,#28783);
#24367=AXIS2_PLACEMENT_3D('',#47994,#28784,#28785);
#24368=AXIS2_PLACEMENT_3D('',#47995,#28786,#28787);
#24369=AXIS2_PLACEMENT_3D('',#47996,#28788,#28789);
#24370=AXIS2_PLACEMENT_3D('',#47997,#28790,#28791);
#24371=AXIS2_PLACEMENT_3D('',#47999,#28792,#28793);
#24372=AXIS2_PLACEMENT_3D('',#48001,#28794,#28795);
#24373=AXIS2_PLACEMENT_3D('',#48002,#28796,#28797);
#24374=AXIS2_PLACEMENT_3D('',#48003,#28798,#28799);
#24375=AXIS2_PLACEMENT_3D('',#48004,#28800,#28801);
#24376=AXIS2_PLACEMENT_3D('',#48005,#28802,#28803);
#24377=AXIS2_PLACEMENT_3D('',#48007,#28804,#28805);
#24378=AXIS2_PLACEMENT_3D('',#48009,#28806,#28807);
#24379=AXIS2_PLACEMENT_3D('',#48014,#28808,#28809);
#24380=AXIS2_PLACEMENT_3D('',#48015,#28810,#28811);
#24381=AXIS2_PLACEMENT_3D('',#48016,#28812,#28813);
#24382=AXIS2_PLACEMENT_3D('',#48017,#28814,#28815);
#24383=AXIS2_PLACEMENT_3D('',#48019,#28816,#28817);
#24384=AXIS2_PLACEMENT_3D('',#48021,#28818,#28819);
#24385=AXIS2_PLACEMENT_3D('',#48022,#28820,#28821);
#24386=AXIS2_PLACEMENT_3D('',#48023,#28822,#28823);
#24387=AXIS2_PLACEMENT_3D('',#48024,#28824,#28825);
#24388=AXIS2_PLACEMENT_3D('',#48025,#28826,#28827);
#24389=AXIS2_PLACEMENT_3D('',#48027,#28828,#28829);
#24390=AXIS2_PLACEMENT_3D('',#48029,#28830,#28831);
#24391=AXIS2_PLACEMENT_3D('',#48034,#28832,#28833);
#24392=AXIS2_PLACEMENT_3D('',#48035,#28834,#28835);
#24393=AXIS2_PLACEMENT_3D('',#48036,#28836,#28837);
#24394=AXIS2_PLACEMENT_3D('',#48037,#28838,#28839);
#24395=AXIS2_PLACEMENT_3D('',#48039,#28840,#28841);
#24396=AXIS2_PLACEMENT_3D('',#48041,#28842,#28843);
#24397=AXIS2_PLACEMENT_3D('',#48042,#28844,#28845);
#24398=AXIS2_PLACEMENT_3D('',#48043,#28846,#28847);
#24399=AXIS2_PLACEMENT_3D('',#48044,#28848,#28849);
#24400=AXIS2_PLACEMENT_3D('',#48045,#28850,#28851);
#24401=AXIS2_PLACEMENT_3D('',#48047,#28852,#28853);
#24402=AXIS2_PLACEMENT_3D('',#48049,#28854,#28855);
#24403=AXIS2_PLACEMENT_3D('',#48054,#28856,#28857);
#24404=AXIS2_PLACEMENT_3D('',#48055,#28858,#28859);
#24405=AXIS2_PLACEMENT_3D('',#48056,#28860,#28861);
#24406=AXIS2_PLACEMENT_3D('',#48057,#28862,#28863);
#24407=AXIS2_PLACEMENT_3D('',#48059,#28864,#28865);
#24408=AXIS2_PLACEMENT_3D('',#48061,#28866,#28867);
#24409=AXIS2_PLACEMENT_3D('',#48062,#28868,#28869);
#24410=AXIS2_PLACEMENT_3D('',#48063,#28870,#28871);
#24411=AXIS2_PLACEMENT_3D('',#48064,#28872,#28873);
#24412=AXIS2_PLACEMENT_3D('',#48065,#28874,#28875);
#24413=AXIS2_PLACEMENT_3D('',#48067,#28876,#28877);
#24414=AXIS2_PLACEMENT_3D('',#48069,#28878,#28879);
#24415=AXIS2_PLACEMENT_3D('',#48074,#28880,#28881);
#24416=AXIS2_PLACEMENT_3D('',#48075,#28882,#28883);
#24417=AXIS2_PLACEMENT_3D('',#48076,#28884,#28885);
#24418=AXIS2_PLACEMENT_3D('',#48077,#28886,#28887);
#24419=AXIS2_PLACEMENT_3D('',#48079,#28888,#28889);
#24420=AXIS2_PLACEMENT_3D('',#48081,#28890,#28891);
#24421=AXIS2_PLACEMENT_3D('',#48082,#28892,#28893);
#24422=AXIS2_PLACEMENT_3D('',#48083,#28894,#28895);
#24423=AXIS2_PLACEMENT_3D('',#48084,#28896,#28897);
#24424=AXIS2_PLACEMENT_3D('',#48085,#28898,#28899);
#24425=AXIS2_PLACEMENT_3D('',#48087,#28900,#28901);
#24426=AXIS2_PLACEMENT_3D('',#48089,#28902,#28903);
#24427=AXIS2_PLACEMENT_3D('',#48094,#28904,#28905);
#24428=AXIS2_PLACEMENT_3D('',#48095,#28906,#28907);
#24429=AXIS2_PLACEMENT_3D('',#48096,#28908,#28909);
#24430=AXIS2_PLACEMENT_3D('',#48097,#28910,#28911);
#24431=AXIS2_PLACEMENT_3D('',#48099,#28912,#28913);
#24432=AXIS2_PLACEMENT_3D('',#48101,#28914,#28915);
#24433=AXIS2_PLACEMENT_3D('',#48102,#28916,#28917);
#24434=AXIS2_PLACEMENT_3D('',#48103,#28918,#28919);
#24435=AXIS2_PLACEMENT_3D('',#48104,#28920,#28921);
#24436=AXIS2_PLACEMENT_3D('',#48105,#28922,#28923);
#24437=AXIS2_PLACEMENT_3D('',#48107,#28924,#28925);
#24438=AXIS2_PLACEMENT_3D('',#48109,#28926,#28927);
#24439=AXIS2_PLACEMENT_3D('',#48114,#28928,#28929);
#24440=AXIS2_PLACEMENT_3D('',#48115,#28930,#28931);
#24441=AXIS2_PLACEMENT_3D('',#48116,#28932,#28933);
#24442=AXIS2_PLACEMENT_3D('',#48117,#28934,#28935);
#24443=AXIS2_PLACEMENT_3D('',#48119,#28936,#28937);
#24444=AXIS2_PLACEMENT_3D('',#48121,#28938,#28939);
#24445=AXIS2_PLACEMENT_3D('',#48122,#28940,#28941);
#24446=AXIS2_PLACEMENT_3D('',#48123,#28942,#28943);
#24447=AXIS2_PLACEMENT_3D('',#48124,#28944,#28945);
#24448=AXIS2_PLACEMENT_3D('',#48125,#28946,#28947);
#24449=AXIS2_PLACEMENT_3D('',#48127,#28948,#28949);
#24450=AXIS2_PLACEMENT_3D('',#48129,#28950,#28951);
#24451=AXIS2_PLACEMENT_3D('',#48134,#28952,#28953);
#24452=AXIS2_PLACEMENT_3D('',#48135,#28954,#28955);
#24453=AXIS2_PLACEMENT_3D('',#48136,#28956,#28957);
#24454=AXIS2_PLACEMENT_3D('',#48137,#28958,#28959);
#24455=AXIS2_PLACEMENT_3D('',#48139,#28960,#28961);
#24456=AXIS2_PLACEMENT_3D('',#48141,#28962,#28963);
#24457=AXIS2_PLACEMENT_3D('',#48142,#28964,#28965);
#24458=AXIS2_PLACEMENT_3D('',#48143,#28966,#28967);
#24459=AXIS2_PLACEMENT_3D('',#48144,#28968,#28969);
#24460=AXIS2_PLACEMENT_3D('',#48145,#28970,#28971);
#24461=AXIS2_PLACEMENT_3D('',#48147,#28972,#28973);
#24462=AXIS2_PLACEMENT_3D('',#48149,#28974,#28975);
#24463=AXIS2_PLACEMENT_3D('',#48154,#28976,#28977);
#24464=AXIS2_PLACEMENT_3D('',#48155,#28978,#28979);
#24465=AXIS2_PLACEMENT_3D('',#48156,#28980,#28981);
#24466=AXIS2_PLACEMENT_3D('',#48157,#28982,#28983);
#24467=AXIS2_PLACEMENT_3D('',#48159,#28984,#28985);
#24468=AXIS2_PLACEMENT_3D('',#48161,#28986,#28987);
#24469=AXIS2_PLACEMENT_3D('',#48162,#28988,#28989);
#24470=AXIS2_PLACEMENT_3D('',#48163,#28990,#28991);
#24471=AXIS2_PLACEMENT_3D('',#48164,#28992,#28993);
#24472=AXIS2_PLACEMENT_3D('',#48165,#28994,#28995);
#24473=AXIS2_PLACEMENT_3D('',#48167,#28996,#28997);
#24474=AXIS2_PLACEMENT_3D('',#48169,#28998,#28999);
#24475=AXIS2_PLACEMENT_3D('',#48174,#29000,#29001);
#24476=AXIS2_PLACEMENT_3D('',#48175,#29002,#29003);
#24477=AXIS2_PLACEMENT_3D('',#48176,#29004,#29005);
#24478=AXIS2_PLACEMENT_3D('',#48177,#29006,#29007);
#24479=AXIS2_PLACEMENT_3D('',#48179,#29008,#29009);
#24480=AXIS2_PLACEMENT_3D('',#48181,#29010,#29011);
#24481=AXIS2_PLACEMENT_3D('',#48182,#29012,#29013);
#24482=AXIS2_PLACEMENT_3D('',#48183,#29014,#29015);
#24483=AXIS2_PLACEMENT_3D('',#48184,#29016,#29017);
#24484=AXIS2_PLACEMENT_3D('',#48185,#29018,#29019);
#24485=AXIS2_PLACEMENT_3D('',#48187,#29020,#29021);
#24486=AXIS2_PLACEMENT_3D('',#48189,#29022,#29023);
#24487=AXIS2_PLACEMENT_3D('',#48194,#29024,#29025);
#24488=AXIS2_PLACEMENT_3D('',#48195,#29026,#29027);
#24489=AXIS2_PLACEMENT_3D('',#48196,#29028,#29029);
#24490=AXIS2_PLACEMENT_3D('',#48197,#29030,#29031);
#24491=AXIS2_PLACEMENT_3D('',#48199,#29032,#29033);
#24492=AXIS2_PLACEMENT_3D('',#48201,#29034,#29035);
#24493=AXIS2_PLACEMENT_3D('',#48202,#29036,#29037);
#24494=AXIS2_PLACEMENT_3D('',#48203,#29038,#29039);
#24495=AXIS2_PLACEMENT_3D('',#48204,#29040,#29041);
#24496=AXIS2_PLACEMENT_3D('',#48205,#29042,#29043);
#24497=AXIS2_PLACEMENT_3D('',#48207,#29044,#29045);
#24498=AXIS2_PLACEMENT_3D('',#48209,#29046,#29047);
#24499=AXIS2_PLACEMENT_3D('',#48214,#29048,#29049);
#24500=AXIS2_PLACEMENT_3D('',#48215,#29050,#29051);
#24501=AXIS2_PLACEMENT_3D('',#48216,#29052,#29053);
#24502=AXIS2_PLACEMENT_3D('',#48217,#29054,#29055);
#24503=AXIS2_PLACEMENT_3D('',#48218,#29056,#29057);
#24504=AXIS2_PLACEMENT_3D('',#48219,#29058,#29059);
#24505=AXIS2_PLACEMENT_3D('',#48221,#29060,#29061);
#24506=AXIS2_PLACEMENT_3D('',#48223,#29062,#29063);
#24507=AXIS2_PLACEMENT_3D('',#48224,#29064,#29065);
#24508=AXIS2_PLACEMENT_3D('',#48225,#29066,#29067);
#24509=AXIS2_PLACEMENT_3D('',#48226,#29068,#29069);
#24510=AXIS2_PLACEMENT_3D('',#48228,#29070,#29071);
#24511=AXIS2_PLACEMENT_3D('',#48230,#29072,#29073);
#24512=AXIS2_PLACEMENT_3D('',#48235,#29074,#29075);
#24513=AXIS2_PLACEMENT_3D('',#48237,#29076,#29077);
#24514=AXIS2_PLACEMENT_3D('',#48239,#29079,#29080);
#24515=AXIS2_PLACEMENT_3D('',#48245,#29081,#29082);
#24516=AXIS2_PLACEMENT_3D('',#48246,#29083,#29084);
#24517=AXIS2_PLACEMENT_3D('',#48248,#29085,#29086);
#24518=AXIS2_PLACEMENT_3D('',#48252,#29088,#29089);
#24519=AXIS2_PLACEMENT_3D('',#48258,#29090,#29091);
#24520=AXIS2_PLACEMENT_3D('',#48264,#29092,#29093);
#24521=AXIS2_PLACEMENT_3D('',#48270,#29094,#29095);
#24522=AXIS2_PLACEMENT_3D('',#48276,#29096,#29097);
#24523=AXIS2_PLACEMENT_3D('',#48282,#29098,#29099);
#24524=AXIS2_PLACEMENT_3D('',#48288,#29100,#29101);
#24525=AXIS2_PLACEMENT_3D('',#48293,#29102,#29103);
#24526=AXIS2_PLACEMENT_3D('',#48295,#29104,#29105);
#24527=AXIS2_PLACEMENT_3D('',#48301,#29106,#29107);
#24528=AXIS2_PLACEMENT_3D('',#48307,#29108,#29109);
#24529=AXIS2_PLACEMENT_3D('',#48313,#29110,#29111);
#24530=AXIS2_PLACEMENT_3D('',#48319,#29112,#29113);
#24531=AXIS2_PLACEMENT_3D('',#48325,#29114,#29115);
#24532=AXIS2_PLACEMENT_3D('',#48331,#29116,#29117);
#24533=AXIS2_PLACEMENT_3D('',#48337,#29118,#29119);
#24534=AXIS2_PLACEMENT_3D('',#48343,#29120,#29121);
#24535=AXIS2_PLACEMENT_3D('',#48348,#29122,#29123);
#24536=AXIS2_PLACEMENT_3D('',#48349,#29124,#29125);
#24537=AXIS2_PLACEMENT_3D('',#48351,#29126,#29127);
#24538=AXIS2_PLACEMENT_3D('',#48353,#29129,#29130);
#24539=AXIS2_PLACEMENT_3D('',#48354,#29131,#29132);
#24540=AXIS2_PLACEMENT_3D('',#48355,#29133,#29134);
#24541=AXIS2_PLACEMENT_3D('',#48357,#29135,#29136);
#24542=AXIS2_PLACEMENT_3D('',#48359,#29138,#29139);
#24543=AXIS2_PLACEMENT_3D('',#48360,#29140,#29141);
#24544=AXIS2_PLACEMENT_3D('',#48361,#29142,#29143);
#24545=AXIS2_PLACEMENT_3D('',#48363,#29144,#29145);
#24546=AXIS2_PLACEMENT_3D('',#48365,#29147,#29148);
#24547=AXIS2_PLACEMENT_3D('',#48366,#29149,#29150);
#24548=AXIS2_PLACEMENT_3D('',#48367,#29151,#29152);
#24549=AXIS2_PLACEMENT_3D('',#48369,#29153,#29154);
#24550=AXIS2_PLACEMENT_3D('',#48371,#29156,#29157);
#24551=AXIS2_PLACEMENT_3D('',#48372,#29158,#29159);
#24552=AXIS2_PLACEMENT_3D('',#48373,#29160,#29161);
#24553=AXIS2_PLACEMENT_3D('',#48375,#29162,#29163);
#24554=AXIS2_PLACEMENT_3D('',#48377,#29165,#29166);
#24555=AXIS2_PLACEMENT_3D('',#48378,#29167,#29168);
#24556=AXIS2_PLACEMENT_3D('',#48379,#29169,#29170);
#24557=AXIS2_PLACEMENT_3D('',#48381,#29171,#29172);
#24558=AXIS2_PLACEMENT_3D('',#48383,#29174,#29175);
#24559=AXIS2_PLACEMENT_3D('',#48384,#29176,#29177);
#24560=AXIS2_PLACEMENT_3D('',#48385,#29178,#29179);
#24561=AXIS2_PLACEMENT_3D('',#48387,#29180,#29181);
#24562=AXIS2_PLACEMENT_3D('',#48389,#29183,#29184);
#24563=AXIS2_PLACEMENT_3D('',#48390,#29185,#29186);
#24564=AXIS2_PLACEMENT_3D('',#48391,#29187,#29188);
#24565=AXIS2_PLACEMENT_3D('',#48393,#29189,#29190);
#24566=AXIS2_PLACEMENT_3D('',#48395,#29192,#29193);
#24567=AXIS2_PLACEMENT_3D('',#48396,#29194,#29195);
#24568=AXIS2_PLACEMENT_3D('',#48397,#29196,#29197);
#24569=AXIS2_PLACEMENT_3D('',#48399,#29198,#29199);
#24570=AXIS2_PLACEMENT_3D('',#48401,#29201,#29202);
#24571=AXIS2_PLACEMENT_3D('',#48402,#29203,#29204);
#24572=AXIS2_PLACEMENT_3D('',#48403,#29205,#29206);
#24573=AXIS2_PLACEMENT_3D('',#48405,#29207,#29208);
#24574=AXIS2_PLACEMENT_3D('',#48407,#29210,#29211);
#24575=AXIS2_PLACEMENT_3D('',#48408,#29212,#29213);
#24576=AXIS2_PLACEMENT_3D('',#48409,#29214,#29215);
#24577=AXIS2_PLACEMENT_3D('',#48411,#29216,#29217);
#24578=AXIS2_PLACEMENT_3D('',#48413,#29219,#29220);
#24579=AXIS2_PLACEMENT_3D('',#48414,#29221,#29222);
#24580=AXIS2_PLACEMENT_3D('',#48415,#29223,#29224);
#24581=AXIS2_PLACEMENT_3D('',#48417,#29225,#29226);
#24582=AXIS2_PLACEMENT_3D('',#48419,#29228,#29229);
#24583=AXIS2_PLACEMENT_3D('',#48420,#29230,#29231);
#24584=AXIS2_PLACEMENT_3D('',#48421,#29232,#29233);
#24585=AXIS2_PLACEMENT_3D('',#48423,#29234,#29235);
#24586=AXIS2_PLACEMENT_3D('',#48425,#29237,#29238);
#24587=AXIS2_PLACEMENT_3D('',#48426,#29239,#29240);
#24588=AXIS2_PLACEMENT_3D('',#48427,#29241,#29242);
#24589=AXIS2_PLACEMENT_3D('',#48429,#29243,#29244);
#24590=AXIS2_PLACEMENT_3D('',#48431,#29246,#29247);
#24591=AXIS2_PLACEMENT_3D('',#48432,#29248,#29249);
#24592=AXIS2_PLACEMENT_3D('',#48433,#29250,#29251);
#24593=AXIS2_PLACEMENT_3D('',#48435,#29252,#29253);
#24594=AXIS2_PLACEMENT_3D('',#48437,#29255,#29256);
#24595=AXIS2_PLACEMENT_3D('',#48438,#29257,#29258);
#24596=AXIS2_PLACEMENT_3D('',#48439,#29259,#29260);
#24597=AXIS2_PLACEMENT_3D('',#48441,#29261,#29262);
#24598=AXIS2_PLACEMENT_3D('',#48442,#29263,#29264);
#24599=AXIS2_PLACEMENT_3D('',#48443,#29265,#29266);
#24600=AXIS2_PLACEMENT_3D('',#48445,#29268,#29269);
#24601=AXIS2_PLACEMENT_3D('',#48447,#29270,#29271);
#24602=AXIS2_PLACEMENT_3D('',#48450,#29273,#29274);
#24603=AXIS2_PLACEMENT_3D('',#48451,#29275,#29276);
#24604=AXIS2_PLACEMENT_3D('',#48453,#29277,#29278);
#24605=AXIS2_PLACEMENT_3D('',#48454,#29279,#29280);
#24606=AXIS2_PLACEMENT_3D('',#48456,#29281,#29282);
#24607=AXIS2_PLACEMENT_3D('',#48458,#29284,#29285);
#24608=AXIS2_PLACEMENT_3D('',#48460,#29286,#29287);
#24609=AXIS2_PLACEMENT_3D('',#48462,#29289,#29290);
#24610=AXIS2_PLACEMENT_3D('',#48463,#29291,#29292);
#24611=AXIS2_PLACEMENT_3D('',#48465,#29293,#29294);
#24612=AXIS2_PLACEMENT_3D('',#48466,#29295,#29296);
#24613=AXIS2_PLACEMENT_3D('',#48468,#29297,#29298);
#24614=AXIS2_PLACEMENT_3D('',#48470,#29300,#29301);
#24615=AXIS2_PLACEMENT_3D('',#48472,#29302,#29303);
#24616=AXIS2_PLACEMENT_3D('',#48473,#29304,#29305);
#24617=AXIS2_PLACEMENT_3D('',#48476,#29307,#29308);
#24618=AXIS2_PLACEMENT_3D('',#48477,#29309,#29310);
#24619=AXIS2_PLACEMENT_3D('',#48479,#29312,#29313);
#24620=AXIS2_PLACEMENT_3D('',#48480,#29314,#29315);
#24621=AXIS2_PLACEMENT_3D('',#48482,#29316,#29317);
#24622=AXIS2_PLACEMENT_3D('',#48485,#29319,#29320);
#24623=AXIS2_PLACEMENT_3D('',#48486,#29321,#29322);
#24624=AXIS2_PLACEMENT_3D('',#48488,#29323,#29324);
#24625=AXIS2_PLACEMENT_3D('',#48489,#29325,#29326);
#24626=AXIS2_PLACEMENT_3D('',#48491,#29327,#29328);
#24627=AXIS2_PLACEMENT_3D('',#48493,#29330,#29331);
#24628=AXIS2_PLACEMENT_3D('',#48495,#29332,#29333);
#24629=AXIS2_PLACEMENT_3D('',#48497,#29335,#29336);
#24630=AXIS2_PLACEMENT_3D('',#48499,#29337,#29338);
#24631=AXIS2_PLACEMENT_3D('',#48501,#29340,#29341);
#24632=AXIS2_PLACEMENT_3D('',#48503,#29342,#29343);
#24633=AXIS2_PLACEMENT_3D('',#48504,#29344,#29345);
#24634=AXIS2_PLACEMENT_3D('',#48507,#29347,#29348);
#24635=AXIS2_PLACEMENT_3D('',#48508,#29349,#29350);
#24636=AXIS2_PLACEMENT_3D('',#48510,#29352,#29353);
#24637=AXIS2_PLACEMENT_3D('',#48511,#29354,#29355);
#24638=AXIS2_PLACEMENT_3D('',#48513,#29356,#29357);
#24639=AXIS2_PLACEMENT_3D('',#48516,#29359,#29360);
#24640=AXIS2_PLACEMENT_3D('',#48517,#29361,#29362);
#24641=AXIS2_PLACEMENT_3D('',#48519,#29363,#29364);
#24642=AXIS2_PLACEMENT_3D('',#48522,#29366,#29367);
#24643=AXIS2_PLACEMENT_3D('',#48523,#29368,#29369);
#24644=AXIS2_PLACEMENT_3D('',#48532,#29374,#29375);
#24645=AXIS2_PLACEMENT_3D('',#48534,#29376,#29377);
#24646=AXIS2_PLACEMENT_3D('',#48536,#29378,#29379);
#24647=AXIS2_PLACEMENT_3D('',#48538,#29381,#29382);
#24648=AXIS2_PLACEMENT_3D('',#48544,#29386,#29387);
#24649=AXIS2_PLACEMENT_3D('',#48546,#29388,#29389);
#24650=AXIS2_PLACEMENT_3D('',#48548,#29390,#29391);
#24651=AXIS2_PLACEMENT_3D('',#48550,#29393,#29394);
#24652=AXIS2_PLACEMENT_3D('',#48556,#29398,#29399);
#24653=AXIS2_PLACEMENT_3D('',#48558,#29400,#29401);
#24654=AXIS2_PLACEMENT_3D('',#48560,#29402,#29403);
#24655=AXIS2_PLACEMENT_3D('',#48562,#29405,#29406);
#24656=AXIS2_PLACEMENT_3D('',#48568,#29410,#29411);
#24657=AXIS2_PLACEMENT_3D('',#48569,#29412,#29413);
#24658=AXIS2_PLACEMENT_3D('',#48570,#29414,#29415);
#24659=AXIS2_PLACEMENT_3D('',#48571,#29416,#29417);
#24660=AXIS2_PLACEMENT_3D('',#48572,#29418,#29419);
#24661=AXIS2_PLACEMENT_3D('',#48573,#29420,#29421);
#24662=AXIS2_PLACEMENT_3D('',#48574,#29422,#29423);
#24663=AXIS2_PLACEMENT_3D('',#48593,#29425,#29426);
#24664=AXIS2_PLACEMENT_3D('',#48596,#29428,#29429);
#24665=AXIS2_PLACEMENT_3D('',#48598,#29430,#29431);
#24666=AXIS2_PLACEMENT_3D('',#48609,#29432,#29433);
#24667=AXIS2_PLACEMENT_3D('',#48657,#29435,#29436);
#24668=AXIS2_PLACEMENT_3D('',#48705,#29438,#29439);
#24669=AXIS2_PLACEMENT_3D('',#48753,#29441,#29442);
#24670=AXIS2_PLACEMENT_3D('',#48807,#29444,#29445);
#24671=AXIS2_PLACEMENT_3D('',#48855,#29447,#29448);
#24672=AXIS2_PLACEMENT_3D('',#48903,#29450,#29451);
#24673=AXIS2_PLACEMENT_3D('',#48957,#29453,#29454);
#24674=AXIS2_PLACEMENT_3D('',#49005,#29456,#29457);
#24675=AXIS2_PLACEMENT_3D('',#49053,#29459,#29460);
#24676=AXIS2_PLACEMENT_3D('',#49101,#29462,#29463);
#24677=AXIS2_PLACEMENT_3D('',#49155,#29465,#29466);
#24678=AXIS2_PLACEMENT_3D('',#49203,#29468,#29469);
#24679=AXIS2_PLACEMENT_3D('',#49251,#29471,#29472);
#24680=AXIS2_PLACEMENT_3D('',#49305,#29474,#29475);
#24681=AXIS2_PLACEMENT_3D('',#49353,#29477,#29478);
#24682=AXIS2_PLACEMENT_3D('',#49401,#29480,#29481);
#24683=AXIS2_PLACEMENT_3D('',#49449,#29483,#29484);
#24684=AXIS2_PLACEMENT_3D('',#49503,#29486,#29487);
#24685=AXIS2_PLACEMENT_3D('',#49551,#29489,#29490);
#24686=AXIS2_PLACEMENT_3D('',#49599,#29492,#29493);
#24687=AXIS2_PLACEMENT_3D('',#49653,#29495,#29496);
#24688=AXIS2_PLACEMENT_3D('',#49658,#29498,#29499);
#24689=AXIS2_PLACEMENT_3D('',#49700,#29500,#29501);
#24690=AXIS2_PLACEMENT_3D('',#49713,#29503,#29504);
#24691=AXIS2_PLACEMENT_3D('',#49720,#29505,#29506);
#24692=AXIS2_PLACEMENT_3D('',#49745,#29508,#29509);
#24693=AXIS2_PLACEMENT_3D('',#49770,#29511,#29512);
#24694=AXIS2_PLACEMENT_3D('',#49794,#29514,#29515);
#24695=AXIS2_PLACEMENT_3D('',#49819,#29517,#29518);
#24696=AXIS2_PLACEMENT_3D('',#49844,#29520,#29521);
#24697=AXIS2_PLACEMENT_3D('',#49868,#29523,#29524);
#24698=AXIS2_PLACEMENT_3D('',#49892,#29526,#29527);
#24699=AXIS2_PLACEMENT_3D('',#49917,#29529,#29530);
#24700=AXIS2_PLACEMENT_3D('',#49942,#29532,#29533);
#24701=AXIS2_PLACEMENT_3D('',#49966,#29535,#29536);
#24702=AXIS2_PLACEMENT_3D('',#49991,#29538,#29539);
#24703=AXIS2_PLACEMENT_3D('',#50016,#29541,#29542);
#24704=AXIS2_PLACEMENT_3D('',#50040,#29544,#29545);
#24705=AXIS2_PLACEMENT_3D('',#50064,#29547,#29548);
#24706=AXIS2_PLACEMENT_3D('',#50089,#29550,#29551);
#24707=AXIS2_PLACEMENT_3D('',#50114,#29553,#29554);
#24708=AXIS2_PLACEMENT_3D('',#50138,#29556,#29557);
#24709=AXIS2_PLACEMENT_3D('',#50163,#29559,#29560);
#24710=AXIS2_PLACEMENT_3D('',#50188,#29562,#29563);
#24711=AXIS2_PLACEMENT_3D('',#50212,#29565,#29566);
#24712=AXIS2_PLACEMENT_3D('',#50236,#29568,#29569);
#24713=AXIS2_PLACEMENT_3D('',#50305,#29570,#29571);
#24714=AXIS2_PLACEMENT_3D('',#51033,#29572,#29573);
#24715=AXIS2_PLACEMENT_3D('',#51096,#29574,#29575);
#24716=AXIS2_PLACEMENT_3D('',#51097,#29576,#29577);
#24717=AXIS2_PLACEMENT_3D('',#51691,#29578,#29579);
#24718=AXIS2_PLACEMENT_3D('',#51692,#29580,#29581);
#24719=AXIS2_PLACEMENT_3D('',#51693,#29582,#29583);
#24720=AXIS2_PLACEMENT_3D('',#51695,#29584,#29585);
#24721=AXIS2_PLACEMENT_3D('',#51696,#29586,#29587);
#24722=AXIS2_PLACEMENT_3D('',#51697,#29588,#29589);
#24723=AXIS2_PLACEMENT_3D('',#51699,#29590,#29591);
#24724=AXIS2_PLACEMENT_3D('',#51700,#29592,#29593);
#24725=AXIS2_PLACEMENT_3D('',#51704,#29595,#29596);
#24726=AXIS2_PLACEMENT_3D('',#51705,#29597,#29598);
#24727=AXIS2_PLACEMENT_3D('',#51714,#29603,#29604);
#24728=AXIS2_PLACEMENT_3D('',#51720,#29608,#29609);
#24729=AXIS2_PLACEMENT_3D('',#51726,#29613,#29614);
#24730=AXIS2_PLACEMENT_3D('',#51732,#29618,#29619);
#24731=AXIS2_PLACEMENT_3D('',#51738,#29623,#29624);
#24732=AXIS2_PLACEMENT_3D('',#51741,#29627,#29628);
#24733=AXIS2_PLACEMENT_3D('',#51742,#29629,#29630);
#24734=AXIS2_PLACEMENT_3D('',#51751,#29635,#29636);
#24735=AXIS2_PLACEMENT_3D('',#51753,#29637,#29638);
#24736=AXIS2_PLACEMENT_3D('',#51755,#29640,#29641);
#24737=AXIS2_PLACEMENT_3D('',#51759,#29644,#29645);
#24738=AXIS2_PLACEMENT_3D('',#51760,#29646,#29647);
#24739=AXIS2_PLACEMENT_3D('',#51761,#29648,#29649);
#24740=AXIS2_PLACEMENT_3D('',#51770,#29654,#29655);
#24741=AXIS2_PLACEMENT_3D('',#51772,#29656,#29657);
#24742=AXIS2_PLACEMENT_3D('',#51774,#29659,#29660);
#24743=AXIS2_PLACEMENT_3D('',#51778,#29663,#29664);
#24744=AXIS2_PLACEMENT_3D('',#51779,#29665,#29666);
#24745=AXIS2_PLACEMENT_3D('',#51780,#29667,#29668);
#24746=AXIS2_PLACEMENT_3D('',#51789,#29673,#29674);
#24747=AXIS2_PLACEMENT_3D('',#51791,#29675,#29676);
#24748=AXIS2_PLACEMENT_3D('',#51793,#29678,#29679);
#24749=AXIS2_PLACEMENT_3D('',#51797,#29682,#29683);
#24750=AXIS2_PLACEMENT_3D('',#51798,#29684,#29685);
#24751=AXIS2_PLACEMENT_3D('',#51799,#29686,#29687);
#24752=AXIS2_PLACEMENT_3D('',#51808,#29692,#29693);
#24753=AXIS2_PLACEMENT_3D('',#51810,#29694,#29695);
#24754=AXIS2_PLACEMENT_3D('',#51812,#29697,#29698);
#24755=AXIS2_PLACEMENT_3D('',#51816,#29701,#29702);
#24756=AXIS2_PLACEMENT_3D('',#51817,#29703,#29704);
#24757=AXIS2_PLACEMENT_3D('',#51818,#29705,#29706);
#24758=AXIS2_PLACEMENT_3D('',#51827,#29711,#29712);
#24759=AXIS2_PLACEMENT_3D('',#51829,#29713,#29714);
#24760=AXIS2_PLACEMENT_3D('',#51831,#29716,#29717);
#24761=AXIS2_PLACEMENT_3D('',#51835,#29720,#29721);
#24762=AXIS2_PLACEMENT_3D('',#51836,#29722,#29723);
#24763=AXIS2_PLACEMENT_3D('',#51837,#29724,#29725);
#24764=AXIS2_PLACEMENT_3D('',#51846,#29730,#29731);
#24765=AXIS2_PLACEMENT_3D('',#51848,#29732,#29733);
#24766=AXIS2_PLACEMENT_3D('',#51850,#29735,#29736);
#24767=AXIS2_PLACEMENT_3D('',#51854,#29739,#29740);
#24768=AXIS2_PLACEMENT_3D('',#51855,#29741,#29742);
#24769=AXIS2_PLACEMENT_3D('',#51856,#29743,#29744);
#24770=AXIS2_PLACEMENT_3D('',#51865,#29749,#29750);
#24771=AXIS2_PLACEMENT_3D('',#51867,#29751,#29752);
#24772=AXIS2_PLACEMENT_3D('',#51869,#29754,#29755);
#24773=AXIS2_PLACEMENT_3D('',#51873,#29758,#29759);
#24774=AXIS2_PLACEMENT_3D('',#51874,#29760,#29761);
#24775=AXIS2_PLACEMENT_3D('',#51875,#29762,#29763);
#24776=AXIS2_PLACEMENT_3D('',#51884,#29768,#29769);
#24777=AXIS2_PLACEMENT_3D('',#51886,#29770,#29771);
#24778=AXIS2_PLACEMENT_3D('',#51888,#29773,#29774);
#24779=AXIS2_PLACEMENT_3D('',#51892,#29777,#29778);
#24780=AXIS2_PLACEMENT_3D('',#51893,#29779,#29780);
#24781=AXIS2_PLACEMENT_3D('',#51894,#29781,#29782);
#24782=AXIS2_PLACEMENT_3D('',#51903,#29787,#29788);
#24783=AXIS2_PLACEMENT_3D('',#51905,#29789,#29790);
#24784=AXIS2_PLACEMENT_3D('',#51908,#29792,#29793);
#24785=AXIS2_PLACEMENT_3D('',#51909,#29794,#29795);
#24786=AXIS2_PLACEMENT_3D('',#51913,#29798,#29799);
#24787=AXIS2_PLACEMENT_3D('',#51915,#29800,#29801);
#24788=AXIS2_PLACEMENT_3D('',#51916,#29802,#29803);
#24789=AXIS2_PLACEMENT_3D('',#51917,#29804,#29805);
#24790=AXIS2_PLACEMENT_3D('',#51926,#29810,#29811);
#24791=AXIS2_PLACEMENT_3D('',#51928,#29812,#29813);
#24792=AXIS2_PLACEMENT_3D('',#51930,#29815,#29816);
#24793=AXIS2_PLACEMENT_3D('',#51934,#29819,#29820);
#24794=AXIS2_PLACEMENT_3D('',#51935,#29821,#29822);
#24795=AXIS2_PLACEMENT_3D('',#51936,#29823,#29824);
#24796=AXIS2_PLACEMENT_3D('',#51945,#29829,#29830);
#24797=AXIS2_PLACEMENT_3D('',#51947,#29831,#29832);
#24798=AXIS2_PLACEMENT_3D('',#51949,#29834,#29835);
#24799=AXIS2_PLACEMENT_3D('',#51953,#29838,#29839);
#24800=AXIS2_PLACEMENT_3D('',#51954,#29840,#29841);
#24801=AXIS2_PLACEMENT_3D('',#51955,#29842,#29843);
#24802=AXIS2_PLACEMENT_3D('',#51964,#29848,#29849);
#24803=AXIS2_PLACEMENT_3D('',#51966,#29850,#29851);
#24804=AXIS2_PLACEMENT_3D('',#51968,#29853,#29854);
#24805=AXIS2_PLACEMENT_3D('',#51972,#29857,#29858);
#24806=AXIS2_PLACEMENT_3D('',#51973,#29859,#29860);
#24807=AXIS2_PLACEMENT_3D('',#51974,#29861,#29862);
#24808=AXIS2_PLACEMENT_3D('',#51983,#29867,#29868);
#24809=AXIS2_PLACEMENT_3D('',#51985,#29869,#29870);
#24810=AXIS2_PLACEMENT_3D('',#51987,#29872,#29873);
#24811=AXIS2_PLACEMENT_3D('',#51991,#29876,#29877);
#24812=AXIS2_PLACEMENT_3D('',#51992,#29878,#29879);
#24813=AXIS2_PLACEMENT_3D('',#51993,#29880,#29881);
#24814=AXIS2_PLACEMENT_3D('',#52002,#29886,#29887);
#24815=AXIS2_PLACEMENT_3D('',#52004,#29888,#29889);
#24816=AXIS2_PLACEMENT_3D('',#52006,#29891,#29892);
#24817=AXIS2_PLACEMENT_3D('',#52010,#29895,#29896);
#24818=AXIS2_PLACEMENT_3D('',#52011,#29897,#29898);
#24819=AXIS2_PLACEMENT_3D('',#52012,#29899,#29900);
#24820=AXIS2_PLACEMENT_3D('',#52021,#29905,#29906);
#24821=AXIS2_PLACEMENT_3D('',#52023,#29907,#29908);
#24822=AXIS2_PLACEMENT_3D('',#52025,#29910,#29911);
#24823=AXIS2_PLACEMENT_3D('',#52029,#29914,#29915);
#24824=AXIS2_PLACEMENT_3D('',#52030,#29916,#29917);
#24825=AXIS2_PLACEMENT_3D('',#52031,#29918,#29919);
#24826=AXIS2_PLACEMENT_3D('',#52040,#29924,#29925);
#24827=AXIS2_PLACEMENT_3D('',#52042,#29926,#29927);
#24828=AXIS2_PLACEMENT_3D('',#52044,#29929,#29930);
#24829=AXIS2_PLACEMENT_3D('',#52048,#29933,#29934);
#24830=AXIS2_PLACEMENT_3D('',#52049,#29935,#29936);
#24831=AXIS2_PLACEMENT_3D('',#52050,#29937,#29938);
#24832=AXIS2_PLACEMENT_3D('',#52059,#29943,#29944);
#24833=AXIS2_PLACEMENT_3D('',#52061,#29945,#29946);
#24834=AXIS2_PLACEMENT_3D('',#52063,#29948,#29949);
#24835=AXIS2_PLACEMENT_3D('',#52067,#29952,#29953);
#24836=AXIS2_PLACEMENT_3D('',#52068,#29954,#29955);
#24837=AXIS2_PLACEMENT_3D('',#52069,#29956,#29957);
#24838=AXIS2_PLACEMENT_3D('',#52078,#29962,#29963);
#24839=AXIS2_PLACEMENT_3D('',#52080,#29964,#29965);
#24840=AXIS2_PLACEMENT_3D('',#52082,#29967,#29968);
#24841=AXIS2_PLACEMENT_3D('',#52086,#29971,#29972);
#24842=AXIS2_PLACEMENT_3D('',#52087,#29973,#29974);
#24843=AXIS2_PLACEMENT_3D('',#52088,#29975,#29976);
#24844=AXIS2_PLACEMENT_3D('',#52097,#29981,#29982);
#24845=AXIS2_PLACEMENT_3D('',#52099,#29983,#29984);
#24846=AXIS2_PLACEMENT_3D('',#52101,#29986,#29987);
#24847=AXIS2_PLACEMENT_3D('',#52105,#29990,#29991);
#24848=AXIS2_PLACEMENT_3D('',#52106,#29992,#29993);
#24849=AXIS2_PLACEMENT_3D('',#52107,#29994,#29995);
#24850=AXIS2_PLACEMENT_3D('',#52116,#30000,#30001);
#24851=AXIS2_PLACEMENT_3D('',#52118,#30002,#30003);
#24852=AXIS2_PLACEMENT_3D('',#52120,#30005,#30006);
#24853=AXIS2_PLACEMENT_3D('',#52124,#30009,#30010);
#24854=AXIS2_PLACEMENT_3D('',#52125,#30011,#30012);
#24855=AXIS2_PLACEMENT_3D('',#52126,#30013,#30014);
#24856=AXIS2_PLACEMENT_3D('',#52135,#30019,#30020);
#24857=AXIS2_PLACEMENT_3D('',#52137,#30021,#30022);
#24858=AXIS2_PLACEMENT_3D('',#52139,#30024,#30025);
#24859=AXIS2_PLACEMENT_3D('',#52143,#30028,#30029);
#24860=AXIS2_PLACEMENT_3D('',#52144,#30030,#30031);
#24861=AXIS2_PLACEMENT_3D('',#52145,#30032,#30033);
#24862=AXIS2_PLACEMENT_3D('',#52154,#30038,#30039);
#24863=AXIS2_PLACEMENT_3D('',#52156,#30040,#30041);
#24864=AXIS2_PLACEMENT_3D('',#52158,#30043,#30044);
#24865=AXIS2_PLACEMENT_3D('',#52162,#30047,#30048);
#24866=AXIS2_PLACEMENT_3D('',#52163,#30049,#30050);
#24867=AXIS2_PLACEMENT_3D('',#52164,#30051,#30052);
#24868=AXIS2_PLACEMENT_3D('',#52173,#30057,#30058);
#24869=AXIS2_PLACEMENT_3D('',#52175,#30059,#30060);
#24870=AXIS2_PLACEMENT_3D('',#52177,#30062,#30063);
#24871=AXIS2_PLACEMENT_3D('',#52181,#30066,#30067);
#24872=AXIS2_PLACEMENT_3D('',#52182,#30068,#30069);
#24873=AXIS2_PLACEMENT_3D('',#52183,#30070,#30071);
#24874=AXIS2_PLACEMENT_3D('',#52192,#30076,#30077);
#24875=AXIS2_PLACEMENT_3D('',#52194,#30078,#30079);
#24876=AXIS2_PLACEMENT_3D('',#52196,#30081,#30082);
#24877=AXIS2_PLACEMENT_3D('',#52200,#30085,#30086);
#24878=AXIS2_PLACEMENT_3D('',#52201,#30087,#30088);
#24879=AXIS2_PLACEMENT_3D('',#52202,#30089,#30090);
#24880=AXIS2_PLACEMENT_3D('',#52211,#30095,#30096);
#24881=AXIS2_PLACEMENT_3D('',#52213,#30097,#30098);
#24882=AXIS2_PLACEMENT_3D('',#52215,#30100,#30101);
#24883=AXIS2_PLACEMENT_3D('',#52219,#30104,#30105);
#24884=AXIS2_PLACEMENT_3D('',#52220,#30106,#30107);
#24885=AXIS2_PLACEMENT_3D('',#52221,#30108,#30109);
#24886=AXIS2_PLACEMENT_3D('',#52230,#30114,#30115);
#24887=AXIS2_PLACEMENT_3D('',#52232,#30116,#30117);
#24888=AXIS2_PLACEMENT_3D('',#52234,#30119,#30120);
#24889=AXIS2_PLACEMENT_3D('',#52238,#30123,#30124);
#24890=AXIS2_PLACEMENT_3D('',#52239,#30125,#30126);
#24891=AXIS2_PLACEMENT_3D('',#52240,#30127,#30128);
#24892=AXIS2_PLACEMENT_3D('',#52243,#30129,#30130);
#24893=AXIS2_PLACEMENT_3D('',#52247,#30133,#30134);
#24894=AXIS2_PLACEMENT_3D('',#52253,#30138,#30139);
#24895=AXIS2_PLACEMENT_3D('',#52257,#30142,#30143);
#24896=AXIS2_PLACEMENT_3D('',#52258,#30144,#30145);
#24897=AXIS2_PLACEMENT_3D('',#52259,#30146,#30147);
#24898=AXIS2_PLACEMENT_3D('',#52268,#30152,#30153);
#24899=AXIS2_PLACEMENT_3D('',#52270,#30154,#30155);
#24900=AXIS2_PLACEMENT_3D('',#52272,#30157,#30158);
#24901=AXIS2_PLACEMENT_3D('',#52276,#30161,#30162);
#24902=AXIS2_PLACEMENT_3D('',#52277,#30163,#30164);
#24903=AXIS2_PLACEMENT_3D('',#52278,#30165,#30166);
#24904=AXIS2_PLACEMENT_3D('',#52287,#30171,#30172);
#24905=AXIS2_PLACEMENT_3D('',#52289,#30173,#30174);
#24906=AXIS2_PLACEMENT_3D('',#52291,#30176,#30177);
#24907=AXIS2_PLACEMENT_3D('',#52295,#30180,#30181);
#24908=AXIS2_PLACEMENT_3D('',#52296,#30182,#30183);
#24909=AXIS2_PLACEMENT_3D('',#52297,#30184,#30185);
#24910=AXIS2_PLACEMENT_3D('',#52306,#30190,#30191);
#24911=AXIS2_PLACEMENT_3D('',#52308,#30192,#30193);
#24912=AXIS2_PLACEMENT_3D('',#52310,#30195,#30196);
#24913=AXIS2_PLACEMENT_3D('',#52314,#30199,#30200);
#24914=AXIS2_PLACEMENT_3D('',#52315,#30201,#30202);
#24915=AXIS2_PLACEMENT_3D('',#52316,#30203,#30204);
#24916=AXIS2_PLACEMENT_3D('',#52325,#30209,#30210);
#24917=AXIS2_PLACEMENT_3D('',#52327,#30211,#30212);
#24918=AXIS2_PLACEMENT_3D('',#52329,#30214,#30215);
#24919=AXIS2_PLACEMENT_3D('',#52333,#30218,#30219);
#24920=AXIS2_PLACEMENT_3D('',#52334,#30220,#30221);
#24921=AXIS2_PLACEMENT_3D('',#52335,#30222,#30223);
#24922=AXIS2_PLACEMENT_3D('',#52344,#30228,#30229);
#24923=AXIS2_PLACEMENT_3D('',#52346,#30230,#30231);
#24924=AXIS2_PLACEMENT_3D('',#52348,#30233,#30234);
#24925=AXIS2_PLACEMENT_3D('',#52352,#30237,#30238);
#24926=AXIS2_PLACEMENT_3D('',#52353,#30239,#30240);
#24927=AXIS2_PLACEMENT_3D('',#52354,#30241,#30242);
#24928=AXIS2_PLACEMENT_3D('',#52363,#30247,#30248);
#24929=AXIS2_PLACEMENT_3D('',#52365,#30249,#30250);
#24930=AXIS2_PLACEMENT_3D('',#52367,#30252,#30253);
#24931=AXIS2_PLACEMENT_3D('',#52371,#30256,#30257);
#24932=AXIS2_PLACEMENT_3D('',#52372,#30258,#30259);
#24933=AXIS2_PLACEMENT_3D('',#52373,#30260,#30261);
#24934=AXIS2_PLACEMENT_3D('',#52382,#30266,#30267);
#24935=AXIS2_PLACEMENT_3D('',#52384,#30268,#30269);
#24936=AXIS2_PLACEMENT_3D('',#52386,#30271,#30272);
#24937=AXIS2_PLACEMENT_3D('',#52390,#30275,#30276);
#24938=AXIS2_PLACEMENT_3D('',#52391,#30277,#30278);
#24939=AXIS2_PLACEMENT_3D('',#52392,#30279,#30280);
#24940=AXIS2_PLACEMENT_3D('',#52401,#30285,#30286);
#24941=AXIS2_PLACEMENT_3D('',#52403,#30287,#30288);
#24942=AXIS2_PLACEMENT_3D('',#52405,#30290,#30291);
#24943=AXIS2_PLACEMENT_3D('',#52409,#30294,#30295);
#24944=AXIS2_PLACEMENT_3D('',#52410,#30296,#30297);
#24945=AXIS2_PLACEMENT_3D('',#52411,#30298,#30299);
#24946=AXIS2_PLACEMENT_3D('',#52420,#30304,#30305);
#24947=AXIS2_PLACEMENT_3D('',#52422,#30306,#30307);
#24948=AXIS2_PLACEMENT_3D('',#52424,#30309,#30310);
#24949=AXIS2_PLACEMENT_3D('',#52428,#30313,#30314);
#24950=AXIS2_PLACEMENT_3D('',#52429,#30315,#30316);
#24951=AXIS2_PLACEMENT_3D('',#52430,#30317,#30318);
#24952=AXIS2_PLACEMENT_3D('',#52432,#30319,#30320);
#24953=AXIS2_PLACEMENT_3D('',#52433,#30321,#30322);
#24954=AXIS2_PLACEMENT_3D('',#52435,#30324,#30325);
#24955=AXIS2_PLACEMENT_3D('',#52437,#30326,#30327);
#24956=AXIS2_PLACEMENT_3D('',#52439,#30329,#30330);
#24957=AXIS2_PLACEMENT_3D('',#52440,#30331,#30332);
#24958=AXIS2_PLACEMENT_3D('',#52441,#30333,#30334);
#24959=AXIS2_PLACEMENT_3D('',#52442,#30335,#30336);
#24960=AXIS2_PLACEMENT_3D('',#52443,#30337,#30338);
#24961=AXIS2_PLACEMENT_3D('',#52444,#30339,#30340);
#24962=AXIS2_PLACEMENT_3D('',#52445,#30341,#30342);
#24963=AXIS2_PLACEMENT_3D('',#52446,#30343,#30344);
#24964=AXIS2_PLACEMENT_3D('',#52447,#30345,#30346);
#24965=AXIS2_PLACEMENT_3D('',#52448,#30347,#30348);
#24966=AXIS2_PLACEMENT_3D('',#52449,#30349,#30350);
#24967=AXIS2_PLACEMENT_3D('',#52450,#30351,#30352);
#24968=AXIS2_PLACEMENT_3D('',#52451,#30353,#30354);
#24969=AXIS2_PLACEMENT_3D('',#52452,#30355,#30356);
#24970=AXIS2_PLACEMENT_3D('',#52453,#30357,#30358);
#24971=AXIS2_PLACEMENT_3D('',#52454,#30359,#30360);
#24972=AXIS2_PLACEMENT_3D('',#52455,#30361,#30362);
#24973=AXIS2_PLACEMENT_3D('',#52457,#30364,#30365);
#24974=AXIS2_PLACEMENT_3D('',#52458,#30366,#30367);
#24975=AXIS2_PLACEMENT_3D('',#52459,#30368,#30369);
#24976=AXIS2_PLACEMENT_3D('',#52460,#30370,#30371);
#24977=AXIS2_PLACEMENT_3D('',#52461,#30372,#30373);
#24978=AXIS2_PLACEMENT_3D('',#52462,#30374,#30375);
#24979=AXIS2_PLACEMENT_3D('',#52463,#30376,#30377);
#24980=AXIS2_PLACEMENT_3D('',#52464,#30378,#30379);
#24981=AXIS2_PLACEMENT_3D('',#52465,#30380,#30381);
#24982=AXIS2_PLACEMENT_3D('',#52466,#30382,#30383);
#24983=AXIS2_PLACEMENT_3D('',#52467,#30384,#30385);
#24984=AXIS2_PLACEMENT_3D('',#52468,#30386,#30387);
#24985=AXIS2_PLACEMENT_3D('',#52469,#30388,#30389);
#24986=AXIS2_PLACEMENT_3D('',#52470,#30390,#30391);
#24987=AXIS2_PLACEMENT_3D('',#52471,#30392,#30393);
#24988=AXIS2_PLACEMENT_3D('',#52472,#30394,#30395);
#24989=AXIS2_PLACEMENT_3D('',#52473,#30396,#30397);
#24990=AXIS2_PLACEMENT_3D('',#52474,#30398,#30399);
#24991=AXIS2_PLACEMENT_3D('',#52475,#30400,#30401);
#24992=AXIS2_PLACEMENT_3D('',#52476,#30402,#30403);
#24993=AXIS2_PLACEMENT_3D('',#52477,#30404,#30405);
#24994=AXIS2_PLACEMENT_3D('',#52479,#30406,#30407);
#24995=AXIS2_PLACEMENT_3D('',#52481,#30409,#30410);
#24996=AXIS2_PLACEMENT_3D('',#52482,#30411,#30412);
#24997=AXIS2_PLACEMENT_3D('',#52483,#30413,#30414);
#24998=AXIS2_PLACEMENT_3D('',#52500,#30416,#30417);
#24999=AXIS2_PLACEMENT_3D('',#52511,#30418,#30419);
#25000=AXIS2_PLACEMENT_3D('',#52549,#30421,#30422);
#25001=AXIS2_PLACEMENT_3D('',#52587,#30424,#30425);
#25002=AXIS2_PLACEMENT_3D('',#52624,#30427,#30428);
#25003=AXIS2_PLACEMENT_3D('',#52661,#30430,#30431);
#25004=AXIS2_PLACEMENT_3D('',#52699,#30433,#30434);
#25005=AXIS2_PLACEMENT_3D('',#52737,#30436,#30437);
#25006=AXIS2_PLACEMENT_3D('',#52742,#30439,#30440);
#25007=AXIS2_PLACEMENT_3D('',#52776,#30441,#30442);
#25008=AXIS2_PLACEMENT_3D('',#52798,#30444,#30445);
#25009=AXIS2_PLACEMENT_3D('',#52809,#30446,#30447);
#25010=AXIS2_PLACEMENT_3D('',#52893,#30449,#30450);
#25011=AXIS2_PLACEMENT_3D('',#52983,#30452,#30453);
#25012=AXIS2_PLACEMENT_3D('',#53073,#30455,#30456);
#25013=AXIS2_PLACEMENT_3D('',#53157,#30458,#30459);
#25014=AXIS2_PLACEMENT_3D('',#53247,#30461,#30462);
#25015=AXIS2_PLACEMENT_3D('',#53337,#30464,#30465);
#25016=AXIS2_PLACEMENT_3D('',#53421,#30467,#30468);
#25017=AXIS2_PLACEMENT_3D('',#53511,#30470,#30471);
#25018=AXIS2_PLACEMENT_3D('',#53525,#30473,#30474);
#25019=AXIS2_PLACEMENT_3D('',#53531,#30475,#30476);
#25020=AXIS2_PLACEMENT_3D('',#53569,#30478,#30479);
#25021=AXIS2_PLACEMENT_3D('',#53606,#30481,#30482);
#25022=AXIS2_PLACEMENT_3D('',#53643,#30484,#30485);
#25023=AXIS2_PLACEMENT_3D('',#53681,#30487,#30488);
#25024=AXIS2_PLACEMENT_3D('',#53718,#30490,#30491);
#25025=AXIS2_PLACEMENT_3D('',#53755,#30493,#30494);
#25026=AXIS2_PLACEMENT_3D('',#53793,#30496,#30497);
#25027=AXIS2_PLACEMENT_3D('',#53830,#30499,#30500);
#25028=AXIS2_PLACEMENT_3D('',#53909,#30501,#30502);
#25029=AXIS2_PLACEMENT_3D('',#53911,#30503,#30504);
#25030=AXIS2_PLACEMENT_3D('',#54597,#30505,#30506);
#25031=AXIS2_PLACEMENT_3D('',#54599,#30507,#30508);
#25032=AXIS2_PLACEMENT_3D('',#55200,#30509,#30510);
#25033=AXIS2_PLACEMENT_3D('',#55201,#30511,#30512);
#25034=AXIS2_PLACEMENT_3D('',#57251,#30513,#30514);
#25035=AXIS2_PLACEMENT_3D('',#57253,#30515,#30516);
#25036=AXIS2_PLACEMENT_3D('',#57254,#30517,#30518);
#25037=AXIS2_PLACEMENT_3D('',#57320,#30519,#30520);
#25038=AXIS2_PLACEMENT_3D('',#57321,#30521,#30522);
#25039=AXIS2_PLACEMENT_3D('',#59003,#30523,#30524);
#25040=AXIS2_PLACEMENT_3D('',#59005,#30525,#30526);
#25041=AXIS2_PLACEMENT_3D('',#59035,#30528,#30529);
#25042=AXIS2_PLACEMENT_3D('',#59043,#30532,#30533);
#25043=AXIS2_PLACEMENT_3D('',#59049,#30535,#30536);
#25044=AXIS2_PLACEMENT_3D('',#59055,#30538,#30539);
#25045=AXIS2_PLACEMENT_3D('',#59066,#30541,#30542);
#25046=AXIS2_PLACEMENT_3D('',#59074,#30543,#30544);
#25047=AXIS2_PLACEMENT_3D('',#59076,#30546,#30547);
#25048=AXIS2_PLACEMENT_3D('',#59077,#30548,#30549);
#25049=AXIS2_PLACEMENT_3D('',#59079,#30550,#30551);
#25050=AXIS2_PLACEMENT_3D('',#59080,#30552,#30553);
#25051=AXIS2_PLACEMENT_3D('',#59082,#30554,#30555);
#25052=AXIS2_PLACEMENT_3D('',#59083,#30556,#30557);
#25053=AXIS2_PLACEMENT_3D('',#59085,#30558,#30559);
#25054=AXIS2_PLACEMENT_3D('',#59086,#30560,#30561);
#25055=AXIS2_PLACEMENT_3D('',#59088,#30563,#30564);
#25056=AXIS2_PLACEMENT_3D('',#59089,#30565,#30566);
#25057=AXIS2_PLACEMENT_3D('',#59092,#30568,#30569);
#25058=AXIS2_PLACEMENT_3D('',#59093,#30570,#30571);
#25059=AXIS2_PLACEMENT_3D('',#59095,#30572,#30573);
#25060=AXIS2_PLACEMENT_3D('',#59097,#30575,#30576);
#25061=AXIS2_PLACEMENT_3D('',#59099,#30577,#30578);
#25062=AXIS2_PLACEMENT_3D('',#59100,#30579,#30580);
#25063=AXIS2_PLACEMENT_3D('',#59102,#30582,#30583);
#25064=AXIS2_PLACEMENT_3D('',#59104,#30584,#30585);
#25065=AXIS2_PLACEMENT_3D('',#59105,#30586,#30587);
#25066=AXIS2_PLACEMENT_3D('',#59107,#30589,#30590);
#25067=AXIS2_PLACEMENT_3D('',#59109,#30591,#30592);
#25068=AXIS2_PLACEMENT_3D('',#59111,#30594,#30595);
#25069=AXIS2_PLACEMENT_3D('',#59113,#30596,#30597);
#25070=AXIS2_PLACEMENT_3D('',#59114,#30598,#30599);
#25071=AXIS2_PLACEMENT_3D('',#59116,#30601,#30602);
#25072=AXIS2_PLACEMENT_3D('',#59117,#30603,#30604);
#25073=AXIS2_PLACEMENT_3D('',#59118,#30605,#30606);
#25074=AXIS2_PLACEMENT_3D('',#59119,#30607,#30608);
#25075=AXIS2_PLACEMENT_3D('',#59120,#30609,#30610);
#25076=AXIS2_PLACEMENT_3D('',#59121,#30611,#30612);
#25077=AXIS2_PLACEMENT_3D('',#59122,#30613,#30614);
#25078=AXIS2_PLACEMENT_3D('',#59123,#30615,#30616);
#25079=AXIS2_PLACEMENT_3D('',#59124,#30617,#30618);
#25080=AXIS2_PLACEMENT_3D('',#59125,#30619,#30620);
#25081=AXIS2_PLACEMENT_3D('',#59126,#30621,#30622);
#25082=AXIS2_PLACEMENT_3D('',#59127,#30623,#30624);
#25083=AXIS2_PLACEMENT_3D('',#59128,#30625,#30626);
#25084=AXIS2_PLACEMENT_3D('',#59129,#30627,#30628);
#25085=AXIS2_PLACEMENT_3D('',#59130,#30629,#30630);
#25086=AXIS2_PLACEMENT_3D('',#59131,#30631,#30632);
#25087=AXIS2_PLACEMENT_3D('',#59132,#30633,#30634);
#25088=AXIS2_PLACEMENT_3D('',#59133,#30635,#30636);
#25089=AXIS2_PLACEMENT_3D('',#59134,#30637,#30638);
#25090=AXIS2_PLACEMENT_3D('',#59135,#30639,#30640);
#25091=AXIS2_PLACEMENT_3D('',#59136,#30641,#30642);
#25092=AXIS2_PLACEMENT_3D('',#59137,#30643,#30644);
#25093=AXIS2_PLACEMENT_3D('',#59138,#30645,#30646);
#25094=AXIS2_PLACEMENT_3D('',#59139,#30647,#30648);
#25095=AXIS2_PLACEMENT_3D('',#59140,#30649,#30650);
#25096=AXIS2_PLACEMENT_3D('',#59141,#30651,#30652);
#25097=AXIS2_PLACEMENT_3D('',#59142,#30653,#30654);
#25098=AXIS2_PLACEMENT_3D('',#59143,#30655,#30656);
#25099=AXIS2_PLACEMENT_3D('',#59144,#30657,#30658);
#25100=AXIS2_PLACEMENT_3D('',#59145,#30659,#30660);
#25101=AXIS2_PLACEMENT_3D('',#59146,#30661,#30662);
#25102=AXIS2_PLACEMENT_3D('',#59147,#30663,#30664);
#25103=AXIS2_PLACEMENT_3D('',#59148,#30665,#30666);
#25104=AXIS2_PLACEMENT_3D('',#59149,#30667,#30668);
#25105=AXIS2_PLACEMENT_3D('',#59150,#30669,#30670);
#25106=AXIS2_PLACEMENT_3D('',#59151,#30671,#30672);
#25107=AXIS2_PLACEMENT_3D('',#59152,#30673,#30674);
#25108=AXIS2_PLACEMENT_3D('',#59153,#30675,#30676);
#25109=AXIS2_PLACEMENT_3D('',#59154,#30677,#30678);
#25110=AXIS2_PLACEMENT_3D('',#59155,#30679,#30680);
#25111=AXIS2_PLACEMENT_3D('',#59156,#30681,#30682);
#25112=AXIS2_PLACEMENT_3D('',#59157,#30683,#30684);
#25113=AXIS2_PLACEMENT_3D('',#59158,#30685,#30686);
#25114=AXIS2_PLACEMENT_3D('',#59159,#30687,#30688);
#25115=AXIS2_PLACEMENT_3D('',#59160,#30689,#30690);
#25116=DIRECTION('axis',(0.,0.,1.));
#25117=DIRECTION('refdir',(1.,0.,0.));
#25118=DIRECTION('axis',(0.,0.,1.));
#25119=DIRECTION('refdir',(1.,0.,0.));
#25120=DIRECTION('center_axis',(0.,0.,-1.));
#25121=DIRECTION('ref_axis',(1.,0.,0.));
#25122=DIRECTION('center_axis',(0.,0.,-1.));
#25123=DIRECTION('ref_axis',(1.,0.,0.));
#25124=DIRECTION('',(0.707106781186545,-8.6595605623549E-17,0.70710678118655));
#25125=DIRECTION('center_axis',(0.,0.,1.));
#25126=DIRECTION('ref_axis',(1.,0.,0.));
#25127=DIRECTION('center_axis',(0.,0.,1.));
#25128=DIRECTION('ref_axis',(1.,0.,0.));
#25129=DIRECTION('',(0.,0.,1.));
#25130=DIRECTION('center_axis',(0.,0.,-1.));
#25131=DIRECTION('ref_axis',(1.,0.,0.));
#25132=DIRECTION('center_axis',(0.,0.,-1.));
#25133=DIRECTION('ref_axis',(-1.,0.,0.));
#25134=DIRECTION('center_axis',(0.,0.,1.));
#25135=DIRECTION('ref_axis',(1.,0.,0.));
#25136=DIRECTION('center_axis',(0.,0.,-1.));
#25137=DIRECTION('ref_axis',(1.,0.,0.));
#25138=DIRECTION('center_axis',(0.,0.,-1.));
#25139=DIRECTION('ref_axis',(1.,0.,0.));
#25140=DIRECTION('center_axis',(0.,0.,-1.));
#25141=DIRECTION('ref_axis',(1.,0.,0.));
#25142=DIRECTION('center_axis',(0.,0.,-1.));
#25143=DIRECTION('ref_axis',(1.,0.,0.));
#25144=DIRECTION('center_axis',(0.,0.,1.));
#25145=DIRECTION('ref_axis',(1.,0.,0.));
#25146=DIRECTION('center_axis',(0.,0.,-1.));
#25147=DIRECTION('ref_axis',(1.,0.,0.));
#25148=DIRECTION('center_axis',(0.,0.,-1.));
#25149=DIRECTION('ref_axis',(1.,0.,0.));
#25150=DIRECTION('center_axis',(0.,0.,-1.));
#25151=DIRECTION('ref_axis',(1.,0.,0.));
#25152=DIRECTION('center_axis',(0.,0.,-1.));
#25153=DIRECTION('ref_axis',(1.,0.,0.));
#25154=DIRECTION('center_axis',(0.,0.,1.));
#25155=DIRECTION('ref_axis',(1.,0.,0.));
#25156=DIRECTION('center_axis',(0.,0.,1.));
#25157=DIRECTION('ref_axis',(1.,0.,0.));
#25158=DIRECTION('',(0.707106781186545,8.6595605623549E-17,-0.70710678118655));
#25159=DIRECTION('center_axis',(0.,0.,1.));
#25160=DIRECTION('ref_axis',(1.,0.,0.));
#25161=DIRECTION('center_axis',(0.,0.,1.));
#25162=DIRECTION('ref_axis',(1.,0.,0.));
#25163=DIRECTION('center_axis',(0.,0.,1.));
#25164=DIRECTION('ref_axis',(1.,0.,0.));
#25165=DIRECTION('center_axis',(0.,0.,1.));
#25166=DIRECTION('ref_axis',(1.,0.,0.));
#25167=DIRECTION('center_axis',(0.,0.,1.));
#25168=DIRECTION('ref_axis',(1.,0.,0.));
#25169=DIRECTION('center_axis',(0.,0.,1.));
#25170=DIRECTION('ref_axis',(1.,0.,0.));
#25171=DIRECTION('center_axis',(0.,0.,1.));
#25172=DIRECTION('ref_axis',(1.,0.,0.));
#25173=DIRECTION('center_axis',(0.,0.,1.));
#25174=DIRECTION('ref_axis',(1.,0.,0.));
#25175=DIRECTION('center_axis',(0.,0.,1.));
#25176=DIRECTION('ref_axis',(1.,0.,0.));
#25177=DIRECTION('center_axis',(0.,0.,1.));
#25178=DIRECTION('ref_axis',(1.,0.,0.));
#25179=DIRECTION('center_axis',(0.,0.,1.));
#25180=DIRECTION('ref_axis',(1.,0.,0.));
#25181=DIRECTION('center_axis',(0.,0.,-1.));
#25182=DIRECTION('ref_axis',(1.,0.,0.));
#25183=DIRECTION('',(0.707106781186548,-8.65956056235493E-17,0.707106781186548));
#25184=DIRECTION('center_axis',(0.,0.,1.));
#25185=DIRECTION('ref_axis',(1.,0.,0.));
#25186=DIRECTION('center_axis',(0.,0.,1.));
#25187=DIRECTION('ref_axis',(1.,0.,0.));
#25188=DIRECTION('',(0.,0.,1.));
#25189=DIRECTION('center_axis',(0.,0.,-1.));
#25190=DIRECTION('ref_axis',(1.,0.,0.));
#25191=DIRECTION('center_axis',(0.,0.,1.));
#25192=DIRECTION('ref_axis',(1.,0.,0.));
#25193=DIRECTION('',(0.707106781186548,8.65956056235493E-17,-0.707106781186547));
#25194=DIRECTION('center_axis',(0.,0.,-1.));
#25195=DIRECTION('ref_axis',(1.,0.,0.));
#25196=DIRECTION('',(0.707106781186547,-8.65956056235493E-17,0.707106781186547));
#25197=DIRECTION('center_axis',(0.,0.,1.));
#25198=DIRECTION('ref_axis',(1.,0.,0.));
#25199=DIRECTION('center_axis',(0.,0.,1.));
#25200=DIRECTION('ref_axis',(1.,0.,0.));
#25201=DIRECTION('',(0.,0.,1.));
#25202=DIRECTION('center_axis',(0.,0.,-1.));
#25203=DIRECTION('ref_axis',(1.,0.,0.));
#25204=DIRECTION('center_axis',(0.,0.,1.));
#25205=DIRECTION('ref_axis',(1.,0.,0.));
#25206=DIRECTION('',(0.707106781186548,8.65956056235493E-17,-0.707106781186547));
#25207=DIRECTION('center_axis',(0.,0.,-1.));
#25208=DIRECTION('ref_axis',(1.,0.,0.));
#25209=DIRECTION('',(0.707106781186545,-8.6595605623549E-17,0.70710678118655));
#25210=DIRECTION('center_axis',(0.,0.,1.));
#25211=DIRECTION('ref_axis',(1.,0.,0.));
#25212=DIRECTION('center_axis',(0.,0.,1.));
#25213=DIRECTION('ref_axis',(1.,0.,0.));
#25214=DIRECTION('',(0.,0.,1.));
#25215=DIRECTION('center_axis',(0.,0.,-1.));
#25216=DIRECTION('ref_axis',(1.,0.,0.));
#25217=DIRECTION('center_axis',(0.,0.,1.));
#25218=DIRECTION('ref_axis',(1.,0.,0.));
#25219=DIRECTION('',(0.707106781186545,8.6595605623549E-17,-0.70710678118655));
#25220=DIRECTION('center_axis',(0.,0.,-1.));
#25221=DIRECTION('ref_axis',(1.,0.,0.));
#25222=DIRECTION('',(0.707106781186545,-8.6595605623549E-17,0.70710678118655));
#25223=DIRECTION('center_axis',(0.,0.,1.));
#25224=DIRECTION('ref_axis',(1.,0.,0.));
#25225=DIRECTION('center_axis',(0.,0.,1.));
#25226=DIRECTION('ref_axis',(1.,0.,0.));
#25227=DIRECTION('',(0.,0.,1.));
#25228=DIRECTION('center_axis',(0.,0.,-1.));
#25229=DIRECTION('ref_axis',(1.,0.,0.));
#25230=DIRECTION('center_axis',(0.,0.,1.));
#25231=DIRECTION('ref_axis',(1.,0.,0.));
#25232=DIRECTION('',(0.707106781186545,8.6595605623549E-17,-0.70710678118655));
#25233=DIRECTION('center_axis',(0.,0.,-1.));
#25234=DIRECTION('ref_axis',(1.,0.,0.));
#25235=DIRECTION('',(0.707106781186548,-8.65956056235493E-17,0.707106781186548));
#25236=DIRECTION('center_axis',(0.,0.,1.));
#25237=DIRECTION('ref_axis',(1.,0.,0.));
#25238=DIRECTION('center_axis',(0.,0.,1.));
#25239=DIRECTION('ref_axis',(1.,0.,0.));
#25240=DIRECTION('',(0.,0.,1.));
#25241=DIRECTION('center_axis',(0.,0.,-1.));
#25242=DIRECTION('ref_axis',(1.,0.,0.));
#25243=DIRECTION('center_axis',(0.,0.,1.));
#25244=DIRECTION('ref_axis',(1.,0.,0.));
#25245=DIRECTION('',(0.707106781186548,8.65956056235493E-17,-0.707106781186547));
#25246=DIRECTION('center_axis',(0.,0.,-1.));
#25247=DIRECTION('ref_axis',(1.,0.,0.));
#25248=DIRECTION('',(0.707106781186547,-8.65956056235493E-17,0.707106781186547));
#25249=DIRECTION('center_axis',(0.,0.,1.));
#25250=DIRECTION('ref_axis',(1.,0.,0.));
#25251=DIRECTION('center_axis',(0.,0.,1.));
#25252=DIRECTION('ref_axis',(1.,0.,0.));
#25253=DIRECTION('',(0.,0.,1.));
#25254=DIRECTION('center_axis',(0.,0.,-1.));
#25255=DIRECTION('ref_axis',(1.,0.,0.));
#25256=DIRECTION('center_axis',(0.,0.,1.));
#25257=DIRECTION('ref_axis',(1.,0.,0.));
#25258=DIRECTION('',(0.707106781186548,8.65956056235493E-17,-0.707106781186547));
#25259=DIRECTION('center_axis',(0.,0.,-1.));
#25260=DIRECTION('ref_axis',(1.,0.,0.));
#25261=DIRECTION('',(0.707106781186547,-8.65956056235493E-17,0.707106781186547));
#25262=DIRECTION('center_axis',(0.,0.,1.));
#25263=DIRECTION('ref_axis',(1.,0.,0.));
#25264=DIRECTION('center_axis',(0.,0.,1.));
#25265=DIRECTION('ref_axis',(1.,0.,0.));
#25266=DIRECTION('',(0.,0.,1.));
#25267=DIRECTION('center_axis',(0.,0.,-1.));
#25268=DIRECTION('ref_axis',(1.,0.,0.));
#25269=DIRECTION('center_axis',(0.,0.,1.));
#25270=DIRECTION('ref_axis',(1.,0.,0.));
#25271=DIRECTION('',(0.707106781186548,8.65956056235493E-17,-0.707106781186547));
#25272=DIRECTION('center_axis',(0.,0.,-1.));
#25273=DIRECTION('ref_axis',(1.,0.,0.));
#25274=DIRECTION('',(0.707106781186548,-8.65956056235493E-17,0.707106781186548));
#25275=DIRECTION('center_axis',(0.,0.,1.));
#25276=DIRECTION('ref_axis',(1.,0.,0.));
#25277=DIRECTION('center_axis',(0.,0.,1.));
#25278=DIRECTION('ref_axis',(1.,0.,0.));
#25279=DIRECTION('',(0.,0.,1.));
#25280=DIRECTION('center_axis',(0.,0.,-1.));
#25281=DIRECTION('ref_axis',(1.,0.,0.));
#25282=DIRECTION('center_axis',(0.,0.,1.));
#25283=DIRECTION('ref_axis',(1.,0.,0.));
#25284=DIRECTION('',(0.707106781186548,8.65956056235493E-17,-0.707106781186547));
#25285=DIRECTION('center_axis',(6.12323399573677E-17,0.,1.));
#25286=DIRECTION('ref_axis',(1.,0.,0.));
#25287=DIRECTION('center_axis',(1.22464679914735E-16,-1.,0.));
#25288=DIRECTION('ref_axis',(-1.,-1.22464679914735E-16,0.));
#25289=DIRECTION('center_axis',(0.,0.,1.));
#25290=DIRECTION('ref_axis',(1.,0.,0.));
#25291=DIRECTION('center_axis',(0.,0.,1.));
#25292=DIRECTION('ref_axis',(1.,0.,0.));
#25293=DIRECTION('',(0.707106781186549,8.65956056235496E-17,-0.707106781186546));
#25294=DIRECTION('center_axis',(0.,0.,1.));
#25295=DIRECTION('ref_axis',(1.,0.,0.));
#25296=DIRECTION('center_axis',(0.,0.,1.));
#25297=DIRECTION('ref_axis',(1.,0.,0.));
#25298=DIRECTION('',(0.,0.,-1.));
#25299=DIRECTION('center_axis',(0.,0.,-1.));
#25300=DIRECTION('ref_axis',(1.,0.,0.));
#25301=DIRECTION('',(-0.707106781186549,-8.65956056235496E-17,-0.707106781186546));
#25302=DIRECTION('axis',(0.,0.,1.));
#25303=DIRECTION('refdir',(1.,0.,0.));
#25304=DIRECTION('center_axis',(0.,0.,1.));
#25305=DIRECTION('ref_axis',(1.,0.,0.));
#25306=DIRECTION('center_axis',(0.,0.,1.));
#25307=DIRECTION('ref_axis',(1.,0.,0.));
#25308=DIRECTION('',(0.,0.,-1.));
#25309=DIRECTION('center_axis',(0.,0.,1.));
#25310=DIRECTION('ref_axis',(1.,0.,0.));
#25311=DIRECTION('center_axis',(0.,0.,-1.));
#25312=DIRECTION('ref_axis',(-1.,0.,0.));
#25313=DIRECTION('center_axis',(0.,0.,1.));
#25314=DIRECTION('ref_axis',(1.,0.,0.));
#25315=DIRECTION('center_axis',(0.,0.,1.));
#25316=DIRECTION('ref_axis',(1.,0.,0.));
#25317=DIRECTION('center_axis',(0.,0.,1.));
#25318=DIRECTION('ref_axis',(1.,0.,0.));
#25319=DIRECTION('',(0.707106781186545,8.65956056235491E-17,-0.707106781186549));
#25320=DIRECTION('center_axis',(0.,0.,1.));
#25321=DIRECTION('ref_axis',(1.,0.,0.));
#25322=DIRECTION('center_axis',(0.,0.,1.));
#25323=DIRECTION('ref_axis',(1.,0.,0.));
#25324=DIRECTION('',(0.,0.,-1.));
#25325=DIRECTION('center_axis',(0.,0.,1.));
#25326=DIRECTION('ref_axis',(1.,0.,0.));
#25327=DIRECTION('center_axis',(0.,0.,1.));
#25328=DIRECTION('ref_axis',(1.,0.,0.));
#25329=DIRECTION('center_axis',(0.,0.,1.));
#25330=DIRECTION('ref_axis',(1.,0.,0.));
#25331=DIRECTION('',(0.707106781186548,8.65956056235493E-17,-0.707106781186548));
#25332=DIRECTION('center_axis',(0.,0.,1.));
#25333=DIRECTION('ref_axis',(1.,0.,0.));
#25334=DIRECTION('center_axis',(0.,0.,1.));
#25335=DIRECTION('ref_axis',(1.,0.,0.));
#25336=DIRECTION('',(0.,0.,-1.));
#25337=DIRECTION('center_axis',(0.,0.,1.));
#25338=DIRECTION('ref_axis',(1.,0.,0.));
#25339=DIRECTION('center_axis',(0.,0.,-1.));
#25340=DIRECTION('ref_axis',(1.,0.,0.));
#25341=DIRECTION('',(-0.70710678118654,-8.65956056235484E-17,-0.707106781186555));
#25342=DIRECTION('center_axis',(0.,0.,1.));
#25343=DIRECTION('ref_axis',(1.,0.,0.));
#25344=DIRECTION('center_axis',(0.,0.,-1.));
#25345=DIRECTION('ref_axis',(-1.,0.,0.));
#25346=DIRECTION('center_axis',(0.,0.,1.));
#25347=DIRECTION('ref_axis',(1.,0.,0.));
#25348=DIRECTION('center_axis',(6.12323399573677E-17,0.,1.));
#25349=DIRECTION('ref_axis',(1.,0.,0.));
#25350=DIRECTION('center_axis',(1.22464679914735E-16,-1.,0.));
#25351=DIRECTION('ref_axis',(-1.,-1.22464679914735E-16,0.));
#25352=DIRECTION('axis',(0.,0.,1.));
#25353=DIRECTION('refdir',(1.,0.,0.));
#25354=DIRECTION('center_axis',(0.,-1.,0.));
#25355=DIRECTION('ref_axis',(1.,0.,0.));
#25356=DIRECTION('',(1.,0.,0.));
#25357=DIRECTION('',(0.,0.,1.));
#25358=DIRECTION('',(-0.965925826289068,0.,0.258819045102521));
#25359=DIRECTION('',(0.,0.,1.));
#25360=DIRECTION('',(-1.,0.,0.));
#25361=DIRECTION('',(-0.708118460127311,0.,0.706093652730943));
#25362=DIRECTION('',(0.,0.,1.));
#25363=DIRECTION('center_axis',(0.,1.,0.));
#25364=DIRECTION('ref_axis',(-1.,0.,0.));
#25365=DIRECTION('',(0.,0.,-1.));
#25366=DIRECTION('',(0.708118460127311,0.,-0.706093652730943));
#25367=DIRECTION('',(1.,0.,0.));
#25368=DIRECTION('',(0.,0.,-1.));
#25369=DIRECTION('',(0.965925826289068,0.,-0.258819045102521));
#25370=DIRECTION('',(0.,0.,1.));
#25371=DIRECTION('',(-1.,0.,0.));
#25372=DIRECTION('center_axis',(-1.,0.,0.));
#25373=DIRECTION('ref_axis',(0.,-1.,0.));
#25374=DIRECTION('',(0.,1.,0.));
#25375=DIRECTION('',(0.,-1.,0.));
#25376=DIRECTION('center_axis',(0.,0.,-1.));
#25377=DIRECTION('ref_axis',(-1.,0.,0.));
#25378=DIRECTION('center_axis',(0.,0.,1.));
#25379=DIRECTION('ref_axis',(1.,0.,0.));
#25380=DIRECTION('center_axis',(0.,0.,-1.));
#25381=DIRECTION('ref_axis',(-1.,0.,0.));
#25382=DIRECTION('center_axis',(0.,0.,1.));
#25383=DIRECTION('ref_axis',(-1.,1.22464679914735E-16,0.));
#25384=DIRECTION('center_axis',(0.,0.,1.));
#25385=DIRECTION('ref_axis',(1.,0.,0.));
#25386=DIRECTION('',(0.793353340291233,-9.91880824887135E-15,0.608761429008723));
#25387=DIRECTION('center_axis',(0.,0.,-1.));
#25388=DIRECTION('ref_axis',(-1.,0.,0.));
#25389=DIRECTION('',(-0.707106781186543,8.65956056235487E-17,0.707106781186552));
#25390=DIRECTION('center_axis',(0.,0.,1.));
#25391=DIRECTION('ref_axis',(-1.,0.,0.));
#25392=DIRECTION('center_axis',(0.,0.,1.));
#25393=DIRECTION('ref_axis',(-1.,0.,0.));
#25394=DIRECTION('center_axis',(0.,0.,1.));
#25395=DIRECTION('ref_axis',(1.,0.,0.));
#25396=DIRECTION('',(0.,0.,-1.));
#25397=DIRECTION('center_axis',(-0.258819045102521,0.,-0.965925826289068));
#25398=DIRECTION('ref_axis',(-0.965925826289068,0.,0.258819045102521));
#25399=DIRECTION('center_axis',(0.,0.,1.));
#25400=DIRECTION('ref_axis',(-1.,9.39371143512797E-13,0.));
#25401=DIRECTION('center_axis',(0.,0.,1.));
#25402=DIRECTION('ref_axis',(1.,0.,0.));
#25403=DIRECTION('',(-0.608761429008725,-7.99043500659679E-17,0.793353340291232));
#25404=DIRECTION('center_axis',(0.,0.,1.));
#25405=DIRECTION('ref_axis',(-1.,1.22464679914735E-16,0.));
#25406=DIRECTION('center_axis',(0.,0.,1.));
#25407=DIRECTION('ref_axis',(1.,0.,0.));
#25408=DIRECTION('center_axis',(0.,0.,-1.));
#25409=DIRECTION('ref_axis',(-1.,1.22464679914735E-16,0.));
#25410=DIRECTION('center_axis',(0.,0.,1.));
#25411=DIRECTION('ref_axis',(1.,0.,0.));
#25412=DIRECTION('center_axis',(0.,0.,1.));
#25413=DIRECTION('ref_axis',(1.,0.,0.));
#25414=DIRECTION('axis',(0.,0.,1.));
#25415=DIRECTION('refdir',(1.,0.,0.));
#25416=DIRECTION('center_axis',(0.,0.,1.));
#25417=DIRECTION('ref_axis',(1.,0.,0.));
#25418=DIRECTION('',(-0.999993517565735,0.00360067028606715,0.));
#25419=DIRECTION('center_axis',(-0.00359876467778075,-0.999464283900328,
0.0325298954870402));
#25420=DIRECTION('ref_axis',(0.99824685088558,-0.00166873393288522,0.0591645165963828));
#25421=DIRECTION('center_axis',(-0.00359876467778075,-0.999464283900328,
0.0325298954870402));
#25422=DIRECTION('ref_axis',(0.99824685088558,-0.00166873393288521,0.0591645165963828));
#25423=DIRECTION('center_axis',(-0.00359876467778075,-0.999464283900328,
0.0325298954870402));
#25424=DIRECTION('ref_axis',(0.99824685088558,-0.00166873393288521,0.0591645165963828));
#25425=DIRECTION('center_axis',(0.,0.,1.));
#25426=DIRECTION('ref_axis',(1.,0.,0.));
#25427=DIRECTION('',(0.999993517565781,0.00360067027305193,0.));
#25428=DIRECTION('center_axis',(-0.00359876466477833,0.999464283902014,
0.0325298954366743));
#25429=DIRECTION('ref_axis',(0.000117129427484697,-0.032529684563767,0.999470762905489));
#25430=DIRECTION('center_axis',(-0.00359876466477833,0.999464283902014,
0.0325298954366743));
#25431=DIRECTION('ref_axis',(0.000117129427484697,-0.032529684563767,0.999470762905488));
#25432=DIRECTION('axis',(0.,0.,1.));
#25433=DIRECTION('refdir',(1.,0.,0.));
#25434=DIRECTION('center_axis',(0.707106781186548,0.707106781186548,0.));
#25435=DIRECTION('ref_axis',(0.,0.,-1.));
#25436=DIRECTION('',(0.707106781186548,-0.707106781186548,0.));
#25437=DIRECTION('',(0.,0.,-1.));
#25438=DIRECTION('',(-0.707106781186548,0.707106781186548,0.));
#25439=DIRECTION('',(0.,0.,1.));
#25440=DIRECTION('center_axis',(-1.,0.,0.));
#25441=DIRECTION('ref_axis',(0.,1.,2.77555756156289E-16));
#25442=DIRECTION('',(0.707106781186548,0.707106781186548,0.));
#25443=DIRECTION('center_axis',(-1.,0.,0.));
#25444=DIRECTION('ref_axis',(0.,1.,2.77555756156289E-16));
#25445=DIRECTION('center_axis',(1.,0.,0.));
#25446=DIRECTION('ref_axis',(0.,1.,2.77555756156289E-16));
#25447=DIRECTION('center_axis',(0.707106781186548,-0.707106781186548,0.));
#25448=DIRECTION('ref_axis',(0.,0.,-1.));
#25449=DIRECTION('',(0.707106781186548,0.707106781186548,0.));
#25450=DIRECTION('',(0.,0.,1.));
#25451=DIRECTION('',(0.,0.,-1.));
#25452=DIRECTION('center_axis',(-1.,0.,0.));
#25453=DIRECTION('ref_axis',(0.,-1.,5.55111512312578E-16));
#25454=DIRECTION('center_axis',(-1.,0.,0.));
#25455=DIRECTION('ref_axis',(0.,-1.,5.55111512312578E-16));
#25456=DIRECTION('center_axis',(1.,0.,0.));
#25457=DIRECTION('ref_axis',(0.,-1.,5.55111512312578E-16));
#25458=DIRECTION('center_axis',(1.,0.,0.));
#25459=DIRECTION('ref_axis',(0.,1.,2.77555756156289E-16));
#25460=DIRECTION('',(1.,0.,0.));
#25461=DIRECTION('center_axis',(1.,0.,0.));
#25462=DIRECTION('ref_axis',(0.,1.,2.77555756156289E-16));
#25463=DIRECTION('',(1.,0.,0.));
#25464=DIRECTION('center_axis',(0.,1.,0.));
#25465=DIRECTION('ref_axis',(0.,0.,1.));
#25466=DIRECTION('',(1.,0.,0.));
#25467=DIRECTION('',(0.,0.,-1.));
#25468=DIRECTION('center_axis',(1.,0.,0.));
#25469=DIRECTION('ref_axis',(0.,0.,-1.));
#25470=DIRECTION('center_axis',(1.,0.,0.));
#25471=DIRECTION('ref_axis',(0.,-1.,5.55111512312578E-16));
#25472=DIRECTION('',(1.,0.,0.));
#25473=DIRECTION('center_axis',(1.,0.,0.));
#25474=DIRECTION('ref_axis',(0.,-1.,5.55111512312578E-16));
#25475=DIRECTION('center_axis',(0.,-1.,0.));
#25476=DIRECTION('ref_axis',(0.,0.,-1.));
#25477=DIRECTION('',(0.,0.,1.));
#25478=DIRECTION('center_axis',(1.,0.,0.));
#25479=DIRECTION('ref_axis',(0.,0.,-1.));
#25480=DIRECTION('axis',(0.,0.,1.));
#25481=DIRECTION('refdir',(1.,0.,0.));
#25482=DIRECTION('center_axis',(0.,0.,1.));
#25483=DIRECTION('ref_axis',(1.,0.,0.));
#25484=DIRECTION('center_axis',(0.,0.,1.));
#25485=DIRECTION('ref_axis',(1.,0.,0.));
#25486=DIRECTION('',(0.,0.,1.));
#25487=DIRECTION('center_axis',(0.,0.,-1.));
#25488=DIRECTION('ref_axis',(1.,0.,0.));
#25489=DIRECTION('center_axis',(0.,0.,1.));
#25490=DIRECTION('ref_axis',(1.,0.,0.));
#25491=DIRECTION('center_axis',(0.,0.,1.));
#25492=DIRECTION('ref_axis',(1.,0.,0.));
#25493=DIRECTION('',(0.,0.,1.));
#25494=DIRECTION('center_axis',(0.,0.,1.));
#25495=DIRECTION('ref_axis',(1.,0.,0.));
#25496=DIRECTION('center_axis',(0.,0.,-1.));
#25497=DIRECTION('ref_axis',(-1.,0.,0.));
#25498=DIRECTION('center_axis',(0.,0.,1.));
#25499=DIRECTION('ref_axis',(1.,0.,0.));
#25500=DIRECTION('center_axis',(0.,0.,1.));
#25501=DIRECTION('ref_axis',(1.,0.,0.));
#25502=DIRECTION('center_axis',(0.,0.,-1.));
#25503=DIRECTION('ref_axis',(-1.,0.,0.));
#25504=DIRECTION('center_axis',(0.,0.,-1.));
#25505=DIRECTION('ref_axis',(-1.,0.,0.));
#25506=DIRECTION('',(0.707106781186548,8.65956056235493E-17,-0.707106781186548));
#25507=DIRECTION('center_axis',(0.,0.,1.));
#25508=DIRECTION('ref_axis',(-1.,0.,0.));
#25509=DIRECTION('center_axis',(0.,0.,1.));
#25510=DIRECTION('ref_axis',(-1.,0.,0.));
#25511=DIRECTION('center_axis',(0.,0.,1.));
#25512=DIRECTION('ref_axis',(1.,0.,0.));
#25513=DIRECTION('',(0.,0.,-1.));
#25514=DIRECTION('center_axis',(0.,0.,-1.));
#25515=DIRECTION('ref_axis',(-1.,0.,0.));
#25516=DIRECTION('center_axis',(0.,0.,-1.));
#25517=DIRECTION('ref_axis',(-1.,0.,0.));
#25518=DIRECTION('center_axis',(0.,0.,1.));
#25519=DIRECTION('ref_axis',(1.,0.,0.));
#25520=DIRECTION('center_axis',(0.,0.,1.));
#25521=DIRECTION('ref_axis',(-1.,0.,0.));
#25522=DIRECTION('',(-0.707106781186548,-8.65956056235493E-17,-0.707106781186548));
#25523=DIRECTION('center_axis',(0.,0.,1.));
#25524=DIRECTION('ref_axis',(-1.,0.,0.));
#25525=DIRECTION('center_axis',(0.,0.,-1.));
#25526=DIRECTION('ref_axis',(-1.,0.,0.));
#25527=DIRECTION('center_axis',(0.,0.,1.));
#25528=DIRECTION('ref_axis',(1.,0.,0.));
#25529=DIRECTION('center_axis',(0.,0.,1.));
#25530=DIRECTION('ref_axis',(1.,0.,0.));
#25531=DIRECTION('center_axis',(0.,0.,1.));
#25532=DIRECTION('ref_axis',(1.,0.,0.));
#25533=DIRECTION('',(0.,0.,-1.));
#25534=DIRECTION('center_axis',(0.,0.,1.));
#25535=DIRECTION('ref_axis',(1.,0.,0.));
#25536=DIRECTION('',(0.,0.,-1.));
#25537=DIRECTION('center_axis',(0.,0.,1.));
#25538=DIRECTION('ref_axis',(1.,0.,0.));
#25539=DIRECTION('center_axis',(0.,0.,-1.));
#25540=DIRECTION('ref_axis',(1.,0.,0.));
#25541=DIRECTION('',(-0.906183139995265,-1.1097542818365E-16,-0.422885465331124));
#25542=DIRECTION('center_axis',(0.,0.,1.));
#25543=DIRECTION('ref_axis',(1.,0.,0.));
#25544=DIRECTION('center_axis',(0.,0.,1.));
#25545=DIRECTION('ref_axis',(1.,0.,0.));
#25546=DIRECTION('',(0.,0.,-1.));
#25547=DIRECTION('center_axis',(0.,0.,1.));
#25548=DIRECTION('ref_axis',(1.,0.,0.));
#25549=DIRECTION('center_axis',(0.,0.,1.));
#25550=DIRECTION('ref_axis',(1.,0.,0.));
#25551=DIRECTION('',(0.948683298050514,1.16180196436212E-16,-0.316227766016838));
#25552=DIRECTION('center_axis',(0.,0.,1.));
#25553=DIRECTION('ref_axis',(1.,0.,0.));
#25554=DIRECTION('center_axis',(0.,0.,1.));
#25555=DIRECTION('ref_axis',(1.,0.,0.));
#25556=DIRECTION('',(0.,0.,-1.));
#25557=DIRECTION('center_axis',(0.,0.,1.));
#25558=DIRECTION('ref_axis',(1.,0.,0.));
#25559=DIRECTION('center_axis',(0.,0.,-1.));
#25560=DIRECTION('ref_axis',(1.,0.,0.));
#25561=DIRECTION('',(-0.906183139995265,-1.1097542818365E-16,-0.422885465331124));
#25562=DIRECTION('center_axis',(0.,0.,1.));
#25563=DIRECTION('ref_axis',(1.,0.,0.));
#25564=DIRECTION('center_axis',(0.,0.,-1.));
#25565=DIRECTION('ref_axis',(-1.,0.,0.));
#25566=DIRECTION('axis',(0.,0.,1.));
#25567=DIRECTION('refdir',(1.,0.,0.));
#25568=DIRECTION('center_axis',(0.,0.,1.));
#25569=DIRECTION('ref_axis',(0.160995516601036,-0.986955137599661,0.));
#25570=DIRECTION('',(0.,0.,1.));
#25571=DIRECTION('center_axis',(0.,0.,1.));
#25572=DIRECTION('ref_axis',(1.,2.60858704573983E-14,0.));
#25573=DIRECTION('center_axis',(0.,0.,1.));
#25574=DIRECTION('ref_axis',(1.,2.60858704573983E-14,0.));
#25575=DIRECTION('',(0.,0.,1.));
#25576=DIRECTION('center_axis',(0.,0.,1.));
#25577=DIRECTION('ref_axis',(1.,2.60858704573983E-14,0.));
#25578=DIRECTION('',(0.,0.,1.));
#25579=DIRECTION('center_axis',(0.,0.,1.));
#25580=DIRECTION('ref_axis',(1.,2.60858704573983E-14,0.));
#25581=DIRECTION('',(0.,0.,1.));
#25582=DIRECTION('center_axis',(0.,0.,1.));
#25583=DIRECTION('ref_axis',(1.,2.60858704573983E-14,0.));
#25584=DIRECTION('',(0.,0.,1.));
#25585=DIRECTION('center_axis',(0.,0.,1.));
#25586=DIRECTION('ref_axis',(1.,2.60858704573983E-14,0.));
#25587=DIRECTION('',(0.,0.,1.));
#25588=DIRECTION('center_axis',(0.,0.,1.));
#25589=DIRECTION('ref_axis',(1.,2.60858704573983E-14,0.));
#25590=DIRECTION('',(0.,0.,1.));
#25591=DIRECTION('center_axis',(0.,0.,1.));
#25592=DIRECTION('ref_axis',(1.,2.60858704573983E-14,0.));
#25593=DIRECTION('',(0.,0.,1.));
#25594=DIRECTION('center_axis',(0.,0.,-1.));
#25595=DIRECTION('ref_axis',(1.,2.60858704573983E-14,0.));
#25596=DIRECTION('center_axis',(0.,0.,1.));
#25597=DIRECTION('ref_axis',(1.,0.,0.));
#25598=DIRECTION('center_axis',(0.,0.,1.));
#25599=DIRECTION('ref_axis',(1.,0.,0.));
#25600=DIRECTION('center_axis',(0.,0.,1.));
#25601=DIRECTION('ref_axis',(1.,0.,0.));
#25602=DIRECTION('center_axis',(0.,0.,-1.));
#25603=DIRECTION('ref_axis',(1.,2.60858704573983E-14,0.));
#25604=DIRECTION('center_axis',(0.,0.,1.));
#25605=DIRECTION('ref_axis',(-0.997062769070685,0.0765887363330732,0.));
#25606=DIRECTION('center_axis',(0.866025403784439,0.5,0.));
#25607=DIRECTION('ref_axis',(0.5,-0.866025403784439,0.));
#25608=DIRECTION('',(0.5,-0.866025403784439,0.));
#25609=DIRECTION('',(0.,0.,-1.));
#25610=DIRECTION('',(0.5,-0.866025403784439,0.));
#25611=DIRECTION('',(0.,0.,-1.));
#25612=DIRECTION('center_axis',(1.20185167898973E-16,1.,0.));
#25613=DIRECTION('ref_axis',(1.,-1.20185167898973E-16,0.));
#25614=DIRECTION('',(1.,-1.20185167898973E-16,0.));
#25615=DIRECTION('',(0.,0.,-1.));
#25616=DIRECTION('',(1.,-1.20185167898973E-16,0.));
#25617=DIRECTION('center_axis',(-0.866025403784439,0.5,0.));
#25618=DIRECTION('ref_axis',(0.5,0.866025403784439,0.));
#25619=DIRECTION('',(0.5,0.866025403784439,0.));
#25620=DIRECTION('',(0.,0.,-1.));
#25621=DIRECTION('',(0.5,0.866025403784439,0.));
#25622=DIRECTION('center_axis',(-0.866025403784439,-0.5,0.));
#25623=DIRECTION('ref_axis',(-0.5,0.866025403784439,0.));
#25624=DIRECTION('',(-0.5,0.866025403784439,0.));
#25625=DIRECTION('',(0.,0.,-1.));
#25626=DIRECTION('',(-0.5,0.866025403784439,0.));
#25627=DIRECTION('center_axis',(-2.40370335797945E-16,-1.,0.));
#25628=DIRECTION('ref_axis',(-1.,2.40370335797945E-16,0.));
#25629=DIRECTION('',(-1.,2.40370335797945E-16,0.));
#25630=DIRECTION('',(0.,0.,-1.));
#25631=DIRECTION('',(-1.,2.40370335797945E-16,0.));
#25632=DIRECTION('center_axis',(0.866025403784439,-0.5,0.));
#25633=DIRECTION('ref_axis',(-0.5,-0.866025403784439,0.));
#25634=DIRECTION('',(-0.5,-0.866025403784439,0.));
#25635=DIRECTION('',(-0.5,-0.866025403784439,0.));
#25636=DIRECTION('center_axis',(0.,0.,-1.));
#25637=DIRECTION('ref_axis',(-1.,0.,0.));
#25638=DIRECTION('center_axis',(-0.890221906442363,-0.455527120257538,0.));
#25639=DIRECTION('ref_axis',(-0.455527120257538,0.890221906442363,0.));
#25640=DIRECTION('',(0.,0.,1.));
#25641=DIRECTION('',(-0.455527120257538,0.890221906442363,0.));
#25642=DIRECTION('',(0.,0.,-1.));
#25643=DIRECTION('',(-0.455527120257538,0.890221906442363,0.));
#25644=DIRECTION('center_axis',(0.,0.,1.));
#25645=DIRECTION('ref_axis',(1.,0.,0.));
#25646=DIRECTION('center_axis',(0.,0.,1.));
#25647=DIRECTION('ref_axis',(1.,0.,0.));
#25648=DIRECTION('',(0.966370941490094,0.257152101767709,0.));
#25649=DIRECTION('center_axis',(-0.257152101767709,0.966370941490094,0.));
#25650=DIRECTION('ref_axis',(0.966370941490094,0.257152101767709,0.));
#25651=DIRECTION('',(0.,0.,-1.));
#25652=DIRECTION('',(0.966370941490094,0.257152101767709,0.));
#25653=DIRECTION('center_axis',(0.,0.,-1.));
#25654=DIRECTION('ref_axis',(-1.,0.,0.));
#25655=DIRECTION('center_axis',(0.,0.,-1.));
#25656=DIRECTION('ref_axis',(1.,0.,0.));
#25657=DIRECTION('center_axis',(-0.998537750647894,-0.0540588617253913,
0.));
#25658=DIRECTION('ref_axis',(-0.0540588617253913,0.998537750647894,0.));
#25659=DIRECTION('',(0.,0.,1.));
#25660=DIRECTION('',(-0.0540588617253913,0.998537750647894,0.));
#25661=DIRECTION('',(0.,0.,-1.));
#25662=DIRECTION('',(-0.0540588617253913,0.998537750647894,0.));
#25663=DIRECTION('center_axis',(0.,0.,1.));
#25664=DIRECTION('ref_axis',(1.,0.,0.));
#25665=DIRECTION('center_axis',(0.,0.,1.));
#25666=DIRECTION('ref_axis',(1.,0.,0.));
#25667=DIRECTION('',(0.987416966628963,-0.158138338214543,0.));
#25668=DIRECTION('center_axis',(0.158138338214543,0.987416966628963,0.));
#25669=DIRECTION('ref_axis',(0.987416966628963,-0.158138338214543,0.));
#25670=DIRECTION('',(0.,0.,-1.));
#25671=DIRECTION('',(0.987416966628963,-0.158138338214543,0.));
#25672=DIRECTION('center_axis',(0.,0.,-1.));
#25673=DIRECTION('ref_axis',(-1.,0.,0.));
#25674=DIRECTION('center_axis',(0.,0.,-1.));
#25675=DIRECTION('ref_axis',(1.,0.,0.));
#25676=DIRECTION('center_axis',(-0.934197346335725,0.356756665108433,0.));
#25677=DIRECTION('ref_axis',(0.356756665108433,0.934197346335725,0.));
#25678=DIRECTION('',(0.,0.,1.));
#25679=DIRECTION('',(0.356756665108433,0.934197346335725,0.));
#25680=DIRECTION('',(0.,0.,-1.));
#25681=DIRECTION('',(0.356756665108433,0.934197346335725,0.));
#25682=DIRECTION('center_axis',(0.,0.,1.));
#25683=DIRECTION('ref_axis',(1.,0.,0.));
#25684=DIRECTION('center_axis',(0.,0.,1.));
#25685=DIRECTION('ref_axis',(1.,0.,0.));
#25686=DIRECTION('',(0.837729627836157,-0.546085222877798,0.));
#25687=DIRECTION('center_axis',(0.546085222877798,0.837729627836157,0.));
#25688=DIRECTION('ref_axis',(0.837729627836157,-0.546085222877798,0.));
#25689=DIRECTION('',(0.,0.,-1.));
#25690=DIRECTION('',(0.837729627836157,-0.546085222877798,0.));
#25691=DIRECTION('center_axis',(0.,0.,-1.));
#25692=DIRECTION('ref_axis',(-1.,0.,0.));
#25693=DIRECTION('center_axis',(0.,0.,-1.));
#25694=DIRECTION('ref_axis',(1.,0.,0.));
#25695=DIRECTION('center_axis',(-0.708325733925652,0.705885723512444,0.));
#25696=DIRECTION('ref_axis',(0.705885723512444,0.708325733925652,0.));
#25697=DIRECTION('',(0.,0.,1.));
#25698=DIRECTION('',(0.705885723512444,0.708325733925652,0.));
#25699=DIRECTION('',(0.,0.,-1.));
#25700=DIRECTION('',(0.705885723512444,0.708325733925652,0.));
#25701=DIRECTION('center_axis',(0.,0.,1.));
#25702=DIRECTION('ref_axis',(1.,0.,0.));
#25703=DIRECTION('center_axis',(0.,0.,1.));
#25704=DIRECTION('ref_axis',(1.,0.,0.));
#25705=DIRECTION('',(0.543191225855731,-0.839609011476978,0.));
#25706=DIRECTION('center_axis',(0.839609011476978,0.543191225855731,0.));
#25707=DIRECTION('ref_axis',(0.543191225855731,-0.839609011476978,0.));
#25708=DIRECTION('',(0.,0.,-1.));
#25709=DIRECTION('',(0.543191225855731,-0.839609011476978,0.));
#25710=DIRECTION('center_axis',(0.,0.,-1.));
#25711=DIRECTION('ref_axis',(-1.,0.,0.));
#25712=DIRECTION('center_axis',(0.,0.,-1.));
#25713=DIRECTION('ref_axis',(1.,0.,0.));
#25714=DIRECTION('center_axis',(-0.359978167182565,0.932960727550673,0.));
#25715=DIRECTION('ref_axis',(0.932960727550673,0.359978167182565,0.));
#25716=DIRECTION('',(0.,0.,1.));
#25717=DIRECTION('',(0.932960727550673,0.359978167182565,0.));
#25718=DIRECTION('',(0.,0.,-1.));
#25719=DIRECTION('',(0.932960727550673,0.359978167182565,0.));
#25720=DIRECTION('center_axis',(0.,0.,1.));
#25721=DIRECTION('ref_axis',(1.,0.,0.));
#25722=DIRECTION('center_axis',(0.,0.,1.));
#25723=DIRECTION('ref_axis',(1.,0.,0.));
#25724=DIRECTION('',(0.154730126187482,-0.987956774383376,0.));
#25725=DIRECTION('center_axis',(0.987956774383376,0.154730126187482,0.));
#25726=DIRECTION('ref_axis',(0.154730126187482,-0.987956774383376,0.));
#25727=DIRECTION('',(0.,0.,-1.));
#25728=DIRECTION('',(0.154730126187482,-0.987956774383376,0.));
#25729=DIRECTION('center_axis',(0.,0.,-1.));
#25730=DIRECTION('ref_axis',(-1.,0.,0.));
#25731=DIRECTION('center_axis',(0.,0.,-1.));
#25732=DIRECTION('ref_axis',(1.,0.,0.));
#25733=DIRECTION('center_axis',(0.0506128949653782,0.998718346113269,0.));
#25734=DIRECTION('ref_axis',(0.998718346113269,-0.0506128949653782,0.));
#25735=DIRECTION('',(0.,0.,1.));
#25736=DIRECTION('',(0.998718346113269,-0.0506128949653782,0.));
#25737=DIRECTION('',(0.,0.,-1.));
#25738=DIRECTION('',(0.998718346113269,-0.0506128949653782,0.));
#25739=DIRECTION('center_axis',(0.,0.,1.));
#25740=DIRECTION('ref_axis',(1.,0.,0.));
#25741=DIRECTION('center_axis',(0.,0.,1.));
#25742=DIRECTION('ref_axis',(1.,0.,0.));
#25743=DIRECTION('',(-0.260485217977654,-0.96547783569336,0.));
#25744=DIRECTION('center_axis',(0.96547783569336,-0.260485217977654,0.));
#25745=DIRECTION('ref_axis',(-0.260485217977654,-0.96547783569336,0.));
#25746=DIRECTION('',(0.,0.,-1.));
#25747=DIRECTION('',(-0.260485217977654,-0.96547783569336,0.));
#25748=DIRECTION('center_axis',(0.,0.,-1.));
#25749=DIRECTION('ref_axis',(-1.,0.,0.));
#25750=DIRECTION('center_axis',(0.,0.,-1.));
#25751=DIRECTION('ref_axis',(1.,0.,0.));
#25752=DIRECTION('center_axis',(0.452452527770092,0.891788489561541,0.));
#25753=DIRECTION('ref_axis',(0.891788489561541,-0.452452527770092,0.));
#25754=DIRECTION('',(0.,0.,1.));
#25755=DIRECTION('',(0.891788489561541,-0.452452527770092,0.));
#25756=DIRECTION('',(0.,0.,-1.));
#25757=DIRECTION('',(0.891788489561541,-0.452452527770092,0.));
#25758=DIRECTION('center_axis',(0.,0.,1.));
#25759=DIRECTION('ref_axis',(1.,0.,0.));
#25760=DIRECTION('center_axis',(0.,0.,1.));
#25761=DIRECTION('ref_axis',(1.,0.,0.));
#25762=DIRECTION('',(-0.630660301520536,-0.776059008121178,0.));
#25763=DIRECTION('center_axis',(0.776059008121178,-0.630660301520536,0.));
#25764=DIRECTION('ref_axis',(-0.630660301520536,-0.776059008121178,0.));
#25765=DIRECTION('',(0.,0.,-1.));
#25766=DIRECTION('',(-0.630660301520536,-0.776059008121178,0.));
#25767=DIRECTION('center_axis',(0.,0.,-1.));
#25768=DIRECTION('ref_axis',(-1.,0.,0.));
#25769=DIRECTION('center_axis',(0.,0.,-1.));
#25770=DIRECTION('ref_axis',(1.,0.,0.));
#25771=DIRECTION('center_axis',(0.,0.,1.));
#25772=DIRECTION('ref_axis',(1.,0.,0.));
#25773=DIRECTION('center_axis',(0.,0.,1.));
#25774=DIRECTION('ref_axis',(1.,0.,0.));
#25775=DIRECTION('',(-0.778230601363197,0.627978607200816,0.));
#25776=DIRECTION('',(0.778230601363197,0.627978607200816,0.));
#25777=DIRECTION('center_axis',(-0.627978607200816,-0.778230601363197,0.));
#25778=DIRECTION('ref_axis',(-0.778230601363197,0.627978607200816,0.));
#25779=DIRECTION('',(0.,0.,1.));
#25780=DIRECTION('',(-0.778230601363197,0.627978607200816,0.));
#25781=DIRECTION('',(0.,0.,-1.));
#25782=DIRECTION('center_axis',(-0.627978607200816,0.778230601363197,0.));
#25783=DIRECTION('ref_axis',(0.778230601363197,0.627978607200816,0.));
#25784=DIRECTION('',(0.,0.,-1.));
#25785=DIRECTION('',(0.778230601363197,0.627978607200816,0.));
#25786=DIRECTION('center_axis',(0.,0.,-1.));
#25787=DIRECTION('ref_axis',(-1.,0.,0.));
#25788=DIRECTION('center_axis',(0.,0.,-1.));
#25789=DIRECTION('ref_axis',(1.,0.,0.));
#25790=DIRECTION('center_axis',(0.89022190644236,0.455527120257544,0.));
#25791=DIRECTION('ref_axis',(0.455527120257544,-0.89022190644236,0.));
#25792=DIRECTION('',(0.,0.,1.));
#25793=DIRECTION('',(0.455527120257544,-0.89022190644236,0.));
#25794=DIRECTION('',(0.,0.,-1.));
#25795=DIRECTION('',(0.455527120257544,-0.89022190644236,0.));
#25796=DIRECTION('center_axis',(0.,0.,1.));
#25797=DIRECTION('ref_axis',(1.,0.,0.));
#25798=DIRECTION('center_axis',(0.,0.,1.));
#25799=DIRECTION('ref_axis',(1.,0.,0.));
#25800=DIRECTION('',(-0.966370941490095,-0.257152101767705,0.));
#25801=DIRECTION('center_axis',(0.257152101767705,-0.966370941490095,0.));
#25802=DIRECTION('ref_axis',(-0.966370941490095,-0.257152101767705,0.));
#25803=DIRECTION('',(0.,0.,-1.));
#25804=DIRECTION('',(-0.966370941490095,-0.257152101767705,0.));
#25805=DIRECTION('center_axis',(0.,0.,-1.));
#25806=DIRECTION('ref_axis',(-1.,0.,0.));
#25807=DIRECTION('center_axis',(0.,0.,-1.));
#25808=DIRECTION('ref_axis',(1.,0.,0.));
#25809=DIRECTION('center_axis',(0.998537750647894,0.0540588617253865,0.));
#25810=DIRECTION('ref_axis',(0.0540588617253865,-0.998537750647894,0.));
#25811=DIRECTION('',(0.,0.,1.));
#25812=DIRECTION('',(0.0540588617253865,-0.998537750647894,0.));
#25813=DIRECTION('',(0.,0.,-1.));
#25814=DIRECTION('',(0.0540588617253865,-0.998537750647894,0.));
#25815=DIRECTION('center_axis',(0.,0.,1.));
#25816=DIRECTION('ref_axis',(1.,0.,0.));
#25817=DIRECTION('center_axis',(0.,0.,1.));
#25818=DIRECTION('ref_axis',(1.,0.,0.));
#25819=DIRECTION('',(-0.987416966628962,0.15813833821455,0.));
#25820=DIRECTION('center_axis',(-0.15813833821455,-0.987416966628962,0.));
#25821=DIRECTION('ref_axis',(-0.987416966628962,0.15813833821455,0.));
#25822=DIRECTION('',(0.,0.,-1.));
#25823=DIRECTION('',(-0.987416966628962,0.15813833821455,0.));
#25824=DIRECTION('center_axis',(0.,0.,-1.));
#25825=DIRECTION('ref_axis',(-1.,0.,0.));
#25826=DIRECTION('center_axis',(0.,0.,-1.));
#25827=DIRECTION('ref_axis',(1.,0.,0.));
#25828=DIRECTION('center_axis',(0.934197346335727,-0.356756665108427,0.));
#25829=DIRECTION('ref_axis',(-0.356756665108427,-0.934197346335727,0.));
#25830=DIRECTION('',(0.,0.,1.));
#25831=DIRECTION('',(-0.356756665108427,-0.934197346335727,0.));
#25832=DIRECTION('',(0.,0.,-1.));
#25833=DIRECTION('',(-0.356756665108427,-0.934197346335727,0.));
#25834=DIRECTION('center_axis',(0.,0.,1.));
#25835=DIRECTION('ref_axis',(1.,0.,0.));
#25836=DIRECTION('center_axis',(0.,0.,1.));
#25837=DIRECTION('ref_axis',(1.,0.,0.));
#25838=DIRECTION('',(-0.837729627836154,0.546085222877803,0.));
#25839=DIRECTION('center_axis',(-0.546085222877803,-0.837729627836154,0.));
#25840=DIRECTION('ref_axis',(-0.837729627836154,0.546085222877803,0.));
#25841=DIRECTION('',(0.,0.,-1.));
#25842=DIRECTION('',(-0.837729627836154,0.546085222877803,0.));
#25843=DIRECTION('center_axis',(0.,0.,-1.));
#25844=DIRECTION('ref_axis',(-1.,0.,0.));
#25845=DIRECTION('center_axis',(0.,0.,-1.));
#25846=DIRECTION('ref_axis',(1.,0.,0.));
#25847=DIRECTION('center_axis',(0.708325733925657,-0.70588572351244,0.));
#25848=DIRECTION('ref_axis',(-0.70588572351244,-0.708325733925657,0.));
#25849=DIRECTION('',(0.,0.,1.));
#25850=DIRECTION('',(-0.70588572351244,-0.708325733925657,0.));
#25851=DIRECTION('',(0.,0.,-1.));
#25852=DIRECTION('',(-0.70588572351244,-0.708325733925657,0.));
#25853=DIRECTION('center_axis',(0.,0.,1.));
#25854=DIRECTION('ref_axis',(1.,0.,0.));
#25855=DIRECTION('center_axis',(0.,0.,1.));
#25856=DIRECTION('ref_axis',(1.,0.,0.));
#25857=DIRECTION('',(-0.543191225855725,0.839609011476982,0.));
#25858=DIRECTION('center_axis',(-0.839609011476982,-0.543191225855725,0.));
#25859=DIRECTION('ref_axis',(-0.543191225855725,0.839609011476982,0.));
#25860=DIRECTION('',(0.,0.,-1.));
#25861=DIRECTION('',(-0.543191225855725,0.839609011476982,0.));
#25862=DIRECTION('center_axis',(0.,0.,-1.));
#25863=DIRECTION('ref_axis',(-1.,0.,0.));
#25864=DIRECTION('center_axis',(0.,0.,-1.));
#25865=DIRECTION('ref_axis',(1.,0.,0.));
#25866=DIRECTION('center_axis',(0.359978167182562,-0.932960727550674,0.));
#25867=DIRECTION('ref_axis',(-0.932960727550674,-0.359978167182562,0.));
#25868=DIRECTION('',(0.,0.,1.));
#25869=DIRECTION('',(-0.932960727550674,-0.359978167182562,0.));
#25870=DIRECTION('',(0.,0.,-1.));
#25871=DIRECTION('',(-0.932960727550674,-0.359978167182562,0.));
#25872=DIRECTION('center_axis',(0.,0.,1.));
#25873=DIRECTION('ref_axis',(1.,0.,0.));
#25874=DIRECTION('center_axis',(0.,0.,1.));
#25875=DIRECTION('ref_axis',(1.,0.,0.));
#25876=DIRECTION('',(-0.154730126187479,0.987956774383377,0.));
#25877=DIRECTION('center_axis',(-0.987956774383377,-0.154730126187479,0.));
#25878=DIRECTION('ref_axis',(-0.154730126187479,0.987956774383377,0.));
#25879=DIRECTION('',(0.,0.,-1.));
#25880=DIRECTION('',(-0.154730126187479,0.987956774383377,0.));
#25881=DIRECTION('center_axis',(0.,0.,-1.));
#25882=DIRECTION('ref_axis',(-1.,0.,0.));
#25883=DIRECTION('center_axis',(0.,0.,-1.));
#25884=DIRECTION('ref_axis',(1.,0.,0.));
#25885=DIRECTION('center_axis',(-0.0506128949653805,-0.998718346113269,
0.));
#25886=DIRECTION('ref_axis',(-0.998718346113269,0.0506128949653805,0.));
#25887=DIRECTION('',(0.,0.,1.));
#25888=DIRECTION('',(-0.998718346113269,0.0506128949653805,0.));
#25889=DIRECTION('',(0.,0.,-1.));
#25890=DIRECTION('',(-0.998718346113269,0.0506128949653805,0.));
#25891=DIRECTION('center_axis',(0.,0.,1.));
#25892=DIRECTION('ref_axis',(1.,0.,0.));
#25893=DIRECTION('center_axis',(0.,0.,1.));
#25894=DIRECTION('ref_axis',(1.,0.,0.));
#25895=DIRECTION('',(0.260485217977653,0.96547783569336,0.));
#25896=DIRECTION('center_axis',(-0.96547783569336,0.260485217977653,0.));
#25897=DIRECTION('ref_axis',(0.260485217977653,0.96547783569336,0.));
#25898=DIRECTION('',(0.,0.,-1.));
#25899=DIRECTION('',(0.260485217977653,0.96547783569336,0.));
#25900=DIRECTION('center_axis',(0.,0.,-1.));
#25901=DIRECTION('ref_axis',(-1.,0.,0.));
#25902=DIRECTION('center_axis',(0.,0.,-1.));
#25903=DIRECTION('ref_axis',(1.,0.,0.));
#25904=DIRECTION('center_axis',(-0.452452527770092,-0.891788489561541,0.));
#25905=DIRECTION('ref_axis',(-0.891788489561541,0.452452527770092,0.));
#25906=DIRECTION('',(0.,0.,1.));
#25907=DIRECTION('',(-0.891788489561541,0.452452527770092,0.));
#25908=DIRECTION('',(0.,0.,-1.));
#25909=DIRECTION('',(-0.891788489561541,0.452452527770092,0.));
#25910=DIRECTION('center_axis',(0.,0.,1.));
#25911=DIRECTION('ref_axis',(1.,0.,0.));
#25912=DIRECTION('center_axis',(0.,0.,1.));
#25913=DIRECTION('ref_axis',(1.,0.,0.));
#25914=DIRECTION('',(0.630660301520534,0.77605900812118,0.));
#25915=DIRECTION('center_axis',(-0.77605900812118,0.630660301520534,0.));
#25916=DIRECTION('ref_axis',(0.630660301520534,0.77605900812118,0.));
#25917=DIRECTION('',(0.,0.,-1.));
#25918=DIRECTION('',(0.630660301520534,0.77605900812118,0.));
#25919=DIRECTION('center_axis',(0.,0.,-1.));
#25920=DIRECTION('ref_axis',(-1.,0.,0.));
#25921=DIRECTION('center_axis',(0.,0.,-1.));
#25922=DIRECTION('ref_axis',(1.,0.,0.));
#25923=DIRECTION('center_axis',(-0.257152101767705,-0.966370941490095,0.));
#25924=DIRECTION('ref_axis',(-0.966370941490095,0.257152101767705,0.));
#25925=DIRECTION('',(0.,0.,1.));
#25926=DIRECTION('',(-0.966370941490095,0.257152101767705,0.));
#25927=DIRECTION('',(0.,0.,-1.));
#25928=DIRECTION('',(-0.966370941490095,0.257152101767705,0.));
#25929=DIRECTION('center_axis',(0.,0.,1.));
#25930=DIRECTION('ref_axis',(1.,0.,0.));
#25931=DIRECTION('center_axis',(0.,0.,1.));
#25932=DIRECTION('ref_axis',(1.,0.,0.));
#25933=DIRECTION('',(0.455527120257543,0.89022190644236,0.));
#25934=DIRECTION('center_axis',(-0.89022190644236,0.455527120257543,0.));
#25935=DIRECTION('ref_axis',(0.455527120257543,0.89022190644236,0.));
#25936=DIRECTION('',(0.,0.,-1.));
#25937=DIRECTION('',(0.455527120257543,0.89022190644236,0.));
#25938=DIRECTION('center_axis',(0.,0.,-1.));
#25939=DIRECTION('ref_axis',(-1.,0.,0.));
#25940=DIRECTION('center_axis',(0.,0.,-1.));
#25941=DIRECTION('ref_axis',(1.,0.,0.));
#25942=DIRECTION('center_axis',(0.158138338214546,-0.987416966628963,0.));
#25943=DIRECTION('ref_axis',(-0.987416966628963,-0.158138338214546,0.));
#25944=DIRECTION('',(0.,0.,1.));
#25945=DIRECTION('',(-0.987416966628963,-0.158138338214546,0.));
#25946=DIRECTION('',(0.,0.,-1.));
#25947=DIRECTION('',(-0.987416966628963,-0.158138338214546,0.));
#25948=DIRECTION('center_axis',(0.,0.,1.));
#25949=DIRECTION('ref_axis',(1.,0.,0.));
#25950=DIRECTION('center_axis',(0.,0.,1.));
#25951=DIRECTION('ref_axis',(1.,0.,0.));
#25952=DIRECTION('',(0.0540588617253865,0.998537750647894,0.));
#25953=DIRECTION('center_axis',(-0.998537750647894,0.0540588617253865,0.));
#25954=DIRECTION('ref_axis',(0.0540588617253865,0.998537750647894,0.));
#25955=DIRECTION('',(0.,0.,-1.));
#25956=DIRECTION('',(0.0540588617253865,0.998537750647894,0.));
#25957=DIRECTION('center_axis',(0.,0.,-1.));
#25958=DIRECTION('ref_axis',(-1.,0.,0.));
#25959=DIRECTION('center_axis',(0.,0.,-1.));
#25960=DIRECTION('ref_axis',(1.,0.,0.));
#25961=DIRECTION('center_axis',(0.546085222877805,-0.837729627836152,0.));
#25962=DIRECTION('ref_axis',(-0.837729627836152,-0.546085222877805,0.));
#25963=DIRECTION('',(0.,0.,1.));
#25964=DIRECTION('',(-0.837729627836152,-0.546085222877805,0.));
#25965=DIRECTION('',(0.,0.,-1.));
#25966=DIRECTION('',(-0.837729627836152,-0.546085222877805,0.));
#25967=DIRECTION('center_axis',(0.,0.,1.));
#25968=DIRECTION('ref_axis',(1.,0.,0.));
#25969=DIRECTION('center_axis',(0.,0.,1.));
#25970=DIRECTION('ref_axis',(1.,0.,0.));
#25971=DIRECTION('',(-0.356756665108427,0.934197346335727,0.));
#25972=DIRECTION('center_axis',(-0.934197346335727,-0.356756665108427,0.));
#25973=DIRECTION('ref_axis',(-0.356756665108427,0.934197346335727,0.));
#25974=DIRECTION('',(0.,0.,-1.));
#25975=DIRECTION('',(-0.356756665108427,0.934197346335727,0.));
#25976=DIRECTION('center_axis',(0.,0.,-1.));
#25977=DIRECTION('ref_axis',(-1.,0.,0.));
#25978=DIRECTION('center_axis',(0.,0.,-1.));
#25979=DIRECTION('ref_axis',(1.,0.,0.));
#25980=DIRECTION('center_axis',(0.839609011476981,-0.543191225855727,0.));
#25981=DIRECTION('ref_axis',(-0.543191225855727,-0.839609011476981,0.));
#25982=DIRECTION('',(0.,0.,1.));
#25983=DIRECTION('',(-0.543191225855727,-0.839609011476981,0.));
#25984=DIRECTION('',(0.,0.,-1.));
#25985=DIRECTION('',(-0.543191225855727,-0.839609011476981,0.));
#25986=DIRECTION('center_axis',(0.,0.,1.));
#25987=DIRECTION('ref_axis',(1.,0.,0.));
#25988=DIRECTION('center_axis',(0.,0.,1.));
#25989=DIRECTION('ref_axis',(1.,0.,0.));
#25990=DIRECTION('',(-0.70588572351244,0.708325733925656,0.));
#25991=DIRECTION('center_axis',(-0.708325733925656,-0.70588572351244,0.));
#25992=DIRECTION('ref_axis',(-0.70588572351244,0.708325733925656,0.));
#25993=DIRECTION('',(0.,0.,-1.));
#25994=DIRECTION('',(-0.70588572351244,0.708325733925656,0.));
#25995=DIRECTION('center_axis',(0.,0.,-1.));
#25996=DIRECTION('ref_axis',(-1.,0.,0.));
#25997=DIRECTION('center_axis',(0.,0.,-1.));
#25998=DIRECTION('ref_axis',(1.,0.,0.));
#25999=DIRECTION('center_axis',(0.987956774383378,-0.154730126187475,0.));
#26000=DIRECTION('ref_axis',(-0.154730126187475,-0.987956774383378,0.));
#26001=DIRECTION('',(0.,0.,1.));
#26002=DIRECTION('',(-0.154730126187475,-0.987956774383378,0.));
#26003=DIRECTION('',(0.,0.,-1.));
#26004=DIRECTION('',(-0.154730126187475,-0.987956774383378,0.));
#26005=DIRECTION('center_axis',(0.,0.,1.));
#26006=DIRECTION('ref_axis',(1.,0.,0.));
#26007=DIRECTION('center_axis',(0.,0.,1.));
#26008=DIRECTION('ref_axis',(1.,0.,0.));
#26009=DIRECTION('',(-0.932960727550675,0.359978167182561,0.));
#26010=DIRECTION('center_axis',(-0.359978167182561,-0.932960727550675,0.));
#26011=DIRECTION('ref_axis',(-0.932960727550675,0.359978167182561,0.));
#26012=DIRECTION('',(0.,0.,-1.));
#26013=DIRECTION('',(-0.932960727550675,0.359978167182561,0.));
#26014=DIRECTION('center_axis',(0.,0.,-1.));
#26015=DIRECTION('ref_axis',(-1.,0.,0.));
#26016=DIRECTION('center_axis',(0.,0.,-1.));
#26017=DIRECTION('ref_axis',(1.,0.,0.));
#26018=DIRECTION('center_axis',(0.965477835693359,0.260485217977657,0.));
#26019=DIRECTION('ref_axis',(0.260485217977657,-0.965477835693359,0.));
#26020=DIRECTION('',(0.,0.,1.));
#26021=DIRECTION('',(0.260485217977657,-0.965477835693359,0.));
#26022=DIRECTION('',(0.,0.,-1.));
#26023=DIRECTION('',(0.260485217977657,-0.965477835693359,0.));
#26024=DIRECTION('center_axis',(0.,0.,1.));
#26025=DIRECTION('ref_axis',(1.,0.,0.));
#26026=DIRECTION('center_axis',(0.,0.,1.));
#26027=DIRECTION('ref_axis',(1.,0.,0.));
#26028=DIRECTION('',(-0.998718346113269,-0.0506128949653804,0.));
#26029=DIRECTION('center_axis',(0.0506128949653804,-0.998718346113269,0.));
#26030=DIRECTION('ref_axis',(-0.998718346113269,-0.0506128949653804,0.));
#26031=DIRECTION('',(0.,0.,-1.));
#26032=DIRECTION('',(-0.998718346113269,-0.0506128949653804,0.));
#26033=DIRECTION('center_axis',(0.,0.,-1.));
#26034=DIRECTION('ref_axis',(-1.,0.,0.));
#26035=DIRECTION('center_axis',(0.,0.,-1.));
#26036=DIRECTION('ref_axis',(1.,0.,0.));
#26037=DIRECTION('center_axis',(0.77605900812118,0.630660301520534,0.));
#26038=DIRECTION('ref_axis',(0.630660301520534,-0.77605900812118,0.));
#26039=DIRECTION('',(0.,0.,1.));
#26040=DIRECTION('',(0.630660301520534,-0.77605900812118,0.));
#26041=DIRECTION('',(0.,0.,-1.));
#26042=DIRECTION('',(0.630660301520534,-0.77605900812118,0.));
#26043=DIRECTION('center_axis',(0.,0.,1.));
#26044=DIRECTION('ref_axis',(1.,0.,0.));
#26045=DIRECTION('center_axis',(0.,0.,1.));
#26046=DIRECTION('ref_axis',(1.,0.,0.));
#26047=DIRECTION('',(-0.891788489561542,-0.452452527770089,0.));
#26048=DIRECTION('center_axis',(0.452452527770089,-0.891788489561542,0.));
#26049=DIRECTION('ref_axis',(-0.891788489561542,-0.452452527770089,0.));
#26050=DIRECTION('',(0.,0.,-1.));
#26051=DIRECTION('',(-0.891788489561542,-0.452452527770089,0.));
#26052=DIRECTION('center_axis',(0.,0.,-1.));
#26053=DIRECTION('ref_axis',(-1.,0.,0.));
#26054=DIRECTION('center_axis',(0.,0.,-1.));
#26055=DIRECTION('ref_axis',(1.,0.,0.));
#26056=DIRECTION('center_axis',(0.627978607200814,0.778230601363199,0.));
#26057=DIRECTION('ref_axis',(0.778230601363199,-0.627978607200814,0.));
#26058=DIRECTION('',(0.,0.,1.));
#26059=DIRECTION('',(0.778230601363199,-0.627978607200814,0.));
#26060=DIRECTION('',(0.,0.,-1.));
#26061=DIRECTION('',(0.778230601363199,-0.627978607200814,0.));
#26062=DIRECTION('center_axis',(0.,0.,1.));
#26063=DIRECTION('ref_axis',(1.,0.,0.));
#26064=DIRECTION('center_axis',(0.,0.,1.));
#26065=DIRECTION('ref_axis',(1.,0.,0.));
#26066=DIRECTION('',(-0.778230601363197,-0.627978607200817,0.));
#26067=DIRECTION('center_axis',(0.,0.,1.));
#26068=DIRECTION('ref_axis',(1.,0.,0.));
#26069=DIRECTION('center_axis',(0.627978607200817,-0.778230601363197,0.));
#26070=DIRECTION('ref_axis',(-0.778230601363197,-0.627978607200817,0.));
#26071=DIRECTION('',(0.,0.,-1.));
#26072=DIRECTION('',(-0.778230601363197,-0.627978607200817,0.));
#26073=DIRECTION('center_axis',(0.,0.,-1.));
#26074=DIRECTION('ref_axis',(-1.,0.,0.));
#26075=DIRECTION('center_axis',(0.,0.,-1.));
#26076=DIRECTION('ref_axis',(1.,0.,0.));
#26077=DIRECTION('center_axis',(0.,0.,-1.));
#26078=DIRECTION('ref_axis',(1.,0.,0.));
#26079=DIRECTION('center_axis',(0.257152101767705,0.966370941490095,0.));
#26080=DIRECTION('ref_axis',(0.966370941490095,-0.257152101767705,0.));
#26081=DIRECTION('',(0.,0.,1.));
#26082=DIRECTION('',(0.966370941490095,-0.257152101767705,0.));
#26083=DIRECTION('',(0.,0.,-1.));
#26084=DIRECTION('',(0.966370941490095,-0.257152101767705,0.));
#26085=DIRECTION('center_axis',(0.,0.,1.));
#26086=DIRECTION('ref_axis',(1.,0.,0.));
#26087=DIRECTION('center_axis',(0.,0.,1.));
#26088=DIRECTION('ref_axis',(1.,0.,0.));
#26089=DIRECTION('',(-0.455527120257545,-0.890221906442359,0.));
#26090=DIRECTION('center_axis',(0.890221906442359,-0.455527120257545,0.));
#26091=DIRECTION('ref_axis',(-0.455527120257545,-0.890221906442359,0.));
#26092=DIRECTION('',(0.,0.,-1.));
#26093=DIRECTION('',(-0.455527120257545,-0.890221906442359,0.));
#26094=DIRECTION('center_axis',(0.,0.,-1.));
#26095=DIRECTION('ref_axis',(-1.,0.,0.));
#26096=DIRECTION('center_axis',(0.,0.,-1.));
#26097=DIRECTION('ref_axis',(1.,0.,0.));
#26098=DIRECTION('center_axis',(-0.158138338214545,0.987416966628963,0.));
#26099=DIRECTION('ref_axis',(0.987416966628963,0.158138338214545,0.));
#26100=DIRECTION('',(0.,0.,1.));
#26101=DIRECTION('',(0.987416966628963,0.158138338214545,0.));
#26102=DIRECTION('',(0.,0.,-1.));
#26103=DIRECTION('',(0.987416966628963,0.158138338214545,0.));
#26104=DIRECTION('center_axis',(0.,0.,1.));
#26105=DIRECTION('ref_axis',(1.,0.,0.));
#26106=DIRECTION('center_axis',(0.,0.,1.));
#26107=DIRECTION('ref_axis',(1.,0.,0.));
#26108=DIRECTION('',(-0.054058861725389,-0.998537750647894,0.));
#26109=DIRECTION('center_axis',(0.998537750647894,-0.054058861725389,0.));
#26110=DIRECTION('ref_axis',(-0.054058861725389,-0.998537750647894,0.));
#26111=DIRECTION('',(0.,0.,-1.));
#26112=DIRECTION('',(-0.054058861725389,-0.998537750647894,0.));
#26113=DIRECTION('center_axis',(0.,0.,-1.));
#26114=DIRECTION('ref_axis',(-1.,0.,0.));
#26115=DIRECTION('center_axis',(0.,0.,-1.));
#26116=DIRECTION('ref_axis',(1.,0.,0.));
#26117=DIRECTION('center_axis',(-0.546085222877805,0.837729627836152,0.));
#26118=DIRECTION('ref_axis',(0.837729627836152,0.546085222877805,0.));
#26119=DIRECTION('',(0.,0.,1.));
#26120=DIRECTION('',(0.837729627836152,0.546085222877805,0.));
#26121=DIRECTION('',(0.,0.,-1.));
#26122=DIRECTION('',(0.837729627836152,0.546085222877805,0.));
#26123=DIRECTION('center_axis',(0.,0.,1.));
#26124=DIRECTION('ref_axis',(1.,0.,0.));
#26125=DIRECTION('center_axis',(0.,0.,1.));
#26126=DIRECTION('ref_axis',(1.,0.,0.));
#26127=DIRECTION('',(0.356756665108425,-0.934197346335727,0.));
#26128=DIRECTION('center_axis',(0.934197346335727,0.356756665108425,0.));
#26129=DIRECTION('ref_axis',(0.356756665108425,-0.934197346335727,0.));
#26130=DIRECTION('',(0.,0.,-1.));
#26131=DIRECTION('',(0.356756665108425,-0.934197346335727,0.));
#26132=DIRECTION('center_axis',(0.,0.,-1.));
#26133=DIRECTION('ref_axis',(-1.,0.,0.));
#26134=DIRECTION('center_axis',(0.,0.,-1.));
#26135=DIRECTION('ref_axis',(1.,0.,0.));
#26136=DIRECTION('center_axis',(-0.839609011476982,0.543191225855725,0.));
#26137=DIRECTION('ref_axis',(0.543191225855725,0.839609011476982,0.));
#26138=DIRECTION('',(0.,0.,1.));
#26139=DIRECTION('',(0.543191225855725,0.839609011476982,0.));
#26140=DIRECTION('',(0.,0.,-1.));
#26141=DIRECTION('',(0.543191225855725,0.839609011476982,0.));
#26142=DIRECTION('center_axis',(0.,0.,1.));
#26143=DIRECTION('ref_axis',(1.,0.,0.));
#26144=DIRECTION('center_axis',(0.,0.,1.));
#26145=DIRECTION('ref_axis',(1.,0.,0.));
#26146=DIRECTION('',(0.705885723512444,-0.708325733925652,0.));
#26147=DIRECTION('center_axis',(0.708325733925652,0.705885723512444,0.));
#26148=DIRECTION('ref_axis',(0.705885723512444,-0.708325733925652,0.));
#26149=DIRECTION('',(0.,0.,-1.));
#26150=DIRECTION('',(0.705885723512444,-0.708325733925652,0.));
#26151=DIRECTION('center_axis',(0.,0.,-1.));
#26152=DIRECTION('ref_axis',(-1.,0.,0.));
#26153=DIRECTION('center_axis',(0.,0.,-1.));
#26154=DIRECTION('ref_axis',(1.,0.,0.));
#26155=DIRECTION('center_axis',(-0.987956774383376,0.154730126187482,0.));
#26156=DIRECTION('ref_axis',(0.154730126187482,0.987956774383376,0.));
#26157=DIRECTION('',(0.,0.,1.));
#26158=DIRECTION('',(0.154730126187482,0.987956774383376,0.));
#26159=DIRECTION('',(0.,0.,-1.));
#26160=DIRECTION('',(0.154730126187482,0.987956774383376,0.));
#26161=DIRECTION('center_axis',(0.,0.,1.));
#26162=DIRECTION('ref_axis',(1.,0.,0.));
#26163=DIRECTION('center_axis',(0.,0.,1.));
#26164=DIRECTION('ref_axis',(1.,0.,0.));
#26165=DIRECTION('',(0.932960727550677,-0.359978167182556,0.));
#26166=DIRECTION('center_axis',(0.359978167182556,0.932960727550677,0.));
#26167=DIRECTION('ref_axis',(0.932960727550677,-0.359978167182556,0.));
#26168=DIRECTION('',(0.,0.,-1.));
#26169=DIRECTION('',(0.932960727550677,-0.359978167182556,0.));
#26170=DIRECTION('center_axis',(0.,0.,-1.));
#26171=DIRECTION('ref_axis',(-1.,0.,0.));
#26172=DIRECTION('center_axis',(0.,0.,-1.));
#26173=DIRECTION('ref_axis',(1.,0.,0.));
#26174=DIRECTION('center_axis',(-0.965477835693361,-0.260485217977651,0.));
#26175=DIRECTION('ref_axis',(-0.260485217977651,0.965477835693361,0.));
#26176=DIRECTION('',(0.,0.,1.));
#26177=DIRECTION('',(-0.260485217977651,0.965477835693361,0.));
#26178=DIRECTION('',(0.,0.,-1.));
#26179=DIRECTION('',(-0.260485217977651,0.965477835693361,0.));
#26180=DIRECTION('center_axis',(0.,0.,1.));
#26181=DIRECTION('ref_axis',(1.,0.,0.));
#26182=DIRECTION('center_axis',(0.,0.,1.));
#26183=DIRECTION('ref_axis',(1.,0.,0.));
#26184=DIRECTION('',(0.998718346113269,0.0506128949653851,0.));
#26185=DIRECTION('center_axis',(-0.0506128949653851,0.998718346113269,0.));
#26186=DIRECTION('ref_axis',(0.998718346113269,0.0506128949653851,0.));
#26187=DIRECTION('',(0.,0.,-1.));
#26188=DIRECTION('',(0.998718346113269,0.0506128949653851,0.));
#26189=DIRECTION('center_axis',(0.,0.,-1.));
#26190=DIRECTION('ref_axis',(-1.,0.,0.));
#26191=DIRECTION('center_axis',(0.,0.,-1.));
#26192=DIRECTION('ref_axis',(1.,0.,0.));
#26193=DIRECTION('center_axis',(-0.776059008121178,-0.630660301520536,0.));
#26194=DIRECTION('ref_axis',(-0.630660301520536,0.776059008121178,0.));
#26195=DIRECTION('',(0.,0.,1.));
#26196=DIRECTION('',(-0.630660301520536,0.776059008121178,0.));
#26197=DIRECTION('',(0.,0.,-1.));
#26198=DIRECTION('',(-0.630660301520536,0.776059008121178,0.));
#26199=DIRECTION('center_axis',(0.,0.,1.));
#26200=DIRECTION('ref_axis',(1.,0.,0.));
#26201=DIRECTION('center_axis',(0.,0.,1.));
#26202=DIRECTION('ref_axis',(1.,0.,0.));
#26203=DIRECTION('',(0.891788489561539,0.452452527770095,0.));
#26204=DIRECTION('center_axis',(-0.452452527770095,0.891788489561539,0.));
#26205=DIRECTION('ref_axis',(0.891788489561539,0.452452527770095,0.));
#26206=DIRECTION('',(0.,0.,-1.));
#26207=DIRECTION('',(0.891788489561539,0.452452527770095,0.));
#26208=DIRECTION('center_axis',(0.,0.,-1.));
#26209=DIRECTION('ref_axis',(-1.,0.,0.));
#26210=DIRECTION('center_axis',(0.,0.,-1.));
#26211=DIRECTION('ref_axis',(1.,0.,0.));
#26212=DIRECTION('center_axis',(0.,0.,1.));
#26213=DIRECTION('ref_axis',(1.,0.,0.));
#26214=DIRECTION('center_axis',(0.,0.,-1.));
#26215=DIRECTION('ref_axis',(1.,0.,0.));
#26216=DIRECTION('',(-0.866025403784439,-1.06057523872491E-16,0.5));
#26217=DIRECTION('center_axis',(0.5,-0.866025403784439,0.));
#26218=DIRECTION('ref_axis',(0.866025403784439,0.5,0.));
#26219=DIRECTION('',(0.,0.,1.));
#26220=DIRECTION('',(0.,0.,1.));
#26221=DIRECTION('center_axis',(1.,-3.49629579342466E-16,0.));
#26222=DIRECTION('ref_axis',(3.49629579342466E-16,1.,0.));
#26223=DIRECTION('',(0.,0.,1.));
#26224=DIRECTION('center_axis',(0.5,0.866025403784439,0.));
#26225=DIRECTION('ref_axis',(-0.866025403784439,0.5,0.));
#26226=DIRECTION('',(0.,0.,1.));
#26227=DIRECTION('center_axis',(0.,0.,-1.));
#26228=DIRECTION('ref_axis',(1.,0.,0.));
#26229=DIRECTION('',(0.866025403784439,1.06057523872491E-16,0.5));
#26230=DIRECTION('center_axis',(0.,0.,1.));
#26231=DIRECTION('ref_axis',(1.,0.,0.));
#26232=DIRECTION('center_axis',(-0.5,0.866025403784439,0.));
#26233=DIRECTION('ref_axis',(-0.866025403784439,-0.5,0.));
#26234=DIRECTION('',(0.,0.,1.));
#26235=DIRECTION('center_axis',(0.,0.,1.));
#26236=DIRECTION('ref_axis',(1.,0.,0.));
#26237=DIRECTION('center_axis',(0.,0.,1.));
#26238=DIRECTION('ref_axis',(1.,0.,0.));
#26239=DIRECTION('center_axis',(0.,0.,1.));
#26240=DIRECTION('ref_axis',(1.,0.,0.));
#26241=DIRECTION('center_axis',(0.,0.,-1.));
#26242=DIRECTION('ref_axis',(1.,0.,0.));
#26243=DIRECTION('center_axis',(-0.5,-0.866025403784439,0.));
#26244=DIRECTION('ref_axis',(0.866025403784439,-0.5,0.));
#26245=DIRECTION('',(0.,0.,1.));
#26246=DIRECTION('center_axis',(-1.,0.,0.));
#26247=DIRECTION('ref_axis',(0.,-1.,0.));
#26248=DIRECTION('center_axis',(0.,0.,1.));
#26249=DIRECTION('ref_axis',(1.,0.,0.));
#26250=DIRECTION('center_axis',(0.,0.,1.));
#26251=DIRECTION('ref_axis',(1.,0.,0.));
#26252=DIRECTION('',(0.,0.,1.));
#26253=DIRECTION('center_axis',(0.,0.,1.));
#26254=DIRECTION('ref_axis',(1.,0.,0.));
#26255=DIRECTION('center_axis',(0.,0.,-1.));
#26256=DIRECTION('ref_axis',(1.,0.,0.));
#26257=DIRECTION('',(0.832050294337844,1.01896772969045E-16,0.554700196225229));
#26258=DIRECTION('center_axis',(0.,0.,-1.));
#26259=DIRECTION('ref_axis',(-1.,0.,0.));
#26260=DIRECTION('center_axis',(0.,0.,1.));
#26261=DIRECTION('ref_axis',(1.,0.,0.));
#26262=DIRECTION('center_axis',(0.,0.,1.));
#26263=DIRECTION('ref_axis',(1.,0.,0.));
#26264=DIRECTION('',(0.707106781186547,8.65956056235493E-17,-0.707106781186548));
#26265=DIRECTION('center_axis',(0.,0.,1.));
#26266=DIRECTION('ref_axis',(1.,0.,0.));
#26267=DIRECTION('center_axis',(0.,0.,1.));
#26268=DIRECTION('ref_axis',(1.,0.,0.));
#26269=DIRECTION('center_axis',(0.,0.,1.));
#26270=DIRECTION('ref_axis',(1.,0.,0.));
#26271=DIRECTION('',(0.,0.,-1.));
#26272=DIRECTION('center_axis',(0.,0.,1.));
#26273=DIRECTION('ref_axis',(1.,0.,0.));
#26274=DIRECTION('center_axis',(0.,0.,1.));
#26275=DIRECTION('ref_axis',(1.,0.,0.));
#26276=DIRECTION('center_axis',(0.,0.,1.));
#26277=DIRECTION('ref_axis',(1.,0.,0.));
#26278=DIRECTION('center_axis',(0.,0.,1.));
#26279=DIRECTION('ref_axis',(1.,0.,0.));
#26280=DIRECTION('center_axis',(0.,0.,1.));
#26281=DIRECTION('ref_axis',(1.,0.,0.));
#26282=DIRECTION('center_axis',(0.,0.,1.));
#26283=DIRECTION('ref_axis',(1.,0.,0.));
#26284=DIRECTION('center_axis',(0.,0.,1.));
#26285=DIRECTION('ref_axis',(1.,0.,0.));
#26286=DIRECTION('center_axis',(0.,0.,1.));
#26287=DIRECTION('ref_axis',(1.,0.,0.));
#26288=DIRECTION('center_axis',(0.,0.,1.));
#26289=DIRECTION('ref_axis',(1.,0.,0.));
#26290=DIRECTION('center_axis',(0.,0.,1.));
#26291=DIRECTION('ref_axis',(1.,0.,0.));
#26292=DIRECTION('center_axis',(0.,0.,1.));
#26293=DIRECTION('ref_axis',(1.,0.,0.));
#26294=DIRECTION('center_axis',(0.,0.,1.));
#26295=DIRECTION('ref_axis',(1.,0.,0.));
#26296=DIRECTION('center_axis',(0.,0.,1.));
#26297=DIRECTION('ref_axis',(1.,0.,0.));
#26298=DIRECTION('center_axis',(0.,0.,1.));
#26299=DIRECTION('ref_axis',(1.,0.,0.));
#26300=DIRECTION('',(0.,0.,-1.));
#26301=DIRECTION('center_axis',(0.,0.,1.));
#26302=DIRECTION('ref_axis',(1.,0.,0.));
#26303=DIRECTION('center_axis',(0.,0.,1.));
#26304=DIRECTION('ref_axis',(1.,0.,0.));
#26305=DIRECTION('center_axis',(0.,0.,1.));
#26306=DIRECTION('ref_axis',(1.,0.,0.));
#26307=DIRECTION('center_axis',(0.,0.,1.));
#26308=DIRECTION('ref_axis',(1.,0.,0.));
#26309=DIRECTION('center_axis',(0.,0.,1.));
#26310=DIRECTION('ref_axis',(1.,0.,0.));
#26311=DIRECTION('center_axis',(0.,0.,1.));
#26312=DIRECTION('ref_axis',(1.,0.,0.));
#26313=DIRECTION('center_axis',(0.,0.,1.));
#26314=DIRECTION('ref_axis',(1.,0.,0.));
#26315=DIRECTION('center_axis',(0.,0.,1.));
#26316=DIRECTION('ref_axis',(1.,0.,0.));
#26317=DIRECTION('center_axis',(0.,0.,1.));
#26318=DIRECTION('ref_axis',(1.,0.,0.));
#26319=DIRECTION('center_axis',(0.,0.,1.));
#26320=DIRECTION('ref_axis',(1.,0.,0.));
#26321=DIRECTION('center_axis',(0.,0.,1.));
#26322=DIRECTION('ref_axis',(1.,0.,0.));
#26323=DIRECTION('center_axis',(0.,0.,1.));
#26324=DIRECTION('ref_axis',(1.,0.,0.));
#26325=DIRECTION('center_axis',(0.,0.,1.));
#26326=DIRECTION('ref_axis',(1.,0.,0.));
#26327=DIRECTION('center_axis',(0.,0.,1.));
#26328=DIRECTION('ref_axis',(1.,0.,0.));
#26329=DIRECTION('center_axis',(0.,0.,1.));
#26330=DIRECTION('ref_axis',(1.,0.,0.));
#26331=DIRECTION('center_axis',(0.,0.,1.));
#26332=DIRECTION('ref_axis',(1.,0.,0.));
#26333=DIRECTION('center_axis',(0.,0.,1.));
#26334=DIRECTION('ref_axis',(1.,0.,0.));
#26335=DIRECTION('center_axis',(0.,0.,-1.));
#26336=DIRECTION('ref_axis',(1.,0.,0.));
#26337=DIRECTION('center_axis',(0.,0.,1.));
#26338=DIRECTION('ref_axis',(1.,0.,0.));
#26339=DIRECTION('',(-0.707106781186547,-8.65956056235492E-17,-0.707106781186548));
#26340=DIRECTION('center_axis',(0.,0.,1.));
#26341=DIRECTION('ref_axis',(1.,0.,0.));
#26342=DIRECTION('axis',(0.,0.,1.));
#26343=DIRECTION('refdir',(1.,0.,0.));
#26344=DIRECTION('center_axis',(0.,0.,1.));
#26345=DIRECTION('ref_axis',(0.185354282886115,-0.982671760974016,0.));
#26346=DIRECTION('',(0.,0.,1.));
#26347=DIRECTION('center_axis',(0.,0.,1.));
#26348=DIRECTION('ref_axis',(1.,-1.15782485934285E-14,0.));
#26349=DIRECTION('center_axis',(0.,0.,1.));
#26350=DIRECTION('ref_axis',(1.,-1.15782485934285E-14,0.));
#26351=DIRECTION('',(0.,0.,1.));
#26352=DIRECTION('center_axis',(0.,0.,1.));
#26353=DIRECTION('ref_axis',(1.,-1.15782485934285E-14,0.));
#26354=DIRECTION('',(0.,0.,1.));
#26355=DIRECTION('center_axis',(0.,0.,1.));
#26356=DIRECTION('ref_axis',(1.,-1.15782485934285E-14,0.));
#26357=DIRECTION('',(0.,0.,1.));
#26358=DIRECTION('center_axis',(0.,0.,1.));
#26359=DIRECTION('ref_axis',(1.,-1.15782485934285E-14,0.));
#26360=DIRECTION('',(0.,0.,1.));
#26361=DIRECTION('center_axis',(0.,0.,-1.));
#26362=DIRECTION('ref_axis',(1.,-1.15782485934285E-14,0.));
#26363=DIRECTION('center_axis',(0.,0.,1.));
#26364=DIRECTION('ref_axis',(1.,0.,0.));
#26365=DIRECTION('',(0.,0.,-1.));
#26366=DIRECTION('center_axis',(0.,0.,-1.));
#26367=DIRECTION('ref_axis',(1.,0.,0.));
#26368=DIRECTION('center_axis',(0.,0.,1.));
#26369=DIRECTION('ref_axis',(1.,0.,0.));
#26370=DIRECTION('',(0.,0.,-1.));
#26371=DIRECTION('center_axis',(0.,0.,1.));
#26372=DIRECTION('ref_axis',(1.,0.,0.));
#26373=DIRECTION('',(0.,0.,-1.));
#26374=DIRECTION('center_axis',(0.,0.,1.));
#26375=DIRECTION('ref_axis',(1.,0.,0.));
#26376=DIRECTION('',(0.,0.,-1.));
#26377=DIRECTION('center_axis',(0.,0.,1.));
#26378=DIRECTION('ref_axis',(1.,0.,0.));
#26379=DIRECTION('',(0.,0.,-1.));
#26380=DIRECTION('center_axis',(0.,0.,1.));
#26381=DIRECTION('ref_axis',(1.,0.,0.));
#26382=DIRECTION('',(0.,0.,-1.));
#26383=DIRECTION('center_axis',(0.,0.,1.));
#26384=DIRECTION('ref_axis',(1.,0.,0.));
#26385=DIRECTION('',(0.,0.,-1.));
#26386=DIRECTION('center_axis',(0.,0.,1.));
#26387=DIRECTION('ref_axis',(-0.503961761468012,-0.863725965210065,0.));
#26388=DIRECTION('',(0.,0.,1.));
#26389=DIRECTION('center_axis',(0.,0.,1.));
#26390=DIRECTION('ref_axis',(1.,2.05501931194342E-14,0.));
#26391=DIRECTION('center_axis',(0.,0.,1.));
#26392=DIRECTION('ref_axis',(1.,2.05501931194342E-14,0.));
#26393=DIRECTION('',(0.,0.,1.));
#26394=DIRECTION('center_axis',(0.,0.,1.));
#26395=DIRECTION('ref_axis',(1.,2.05501931194342E-14,0.));
#26396=DIRECTION('',(0.,0.,1.));
#26397=DIRECTION('center_axis',(0.,0.,1.));
#26398=DIRECTION('ref_axis',(1.,2.05501931194342E-14,0.));
#26399=DIRECTION('',(0.,0.,1.));
#26400=DIRECTION('center_axis',(0.,0.,1.));
#26401=DIRECTION('ref_axis',(1.,2.05501931194342E-14,0.));
#26402=DIRECTION('',(0.,0.,1.));
#26403=DIRECTION('center_axis',(0.,0.,1.));
#26404=DIRECTION('ref_axis',(1.,2.05501931194342E-14,0.));
#26405=DIRECTION('',(0.,0.,1.));
#26406=DIRECTION('center_axis',(0.,0.,1.));
#26407=DIRECTION('ref_axis',(1.,2.05501931194342E-14,0.));
#26408=DIRECTION('',(0.,0.,1.));
#26409=DIRECTION('center_axis',(0.,0.,1.));
#26410=DIRECTION('ref_axis',(1.,0.,0.));
#26411=DIRECTION('center_axis',(0.,0.,-1.));
#26412=DIRECTION('ref_axis',(1.,0.,0.));
#26413=DIRECTION('center_axis',(0.,0.,-1.));
#26414=DIRECTION('ref_axis',(1.,0.,0.));
#26415=DIRECTION('center_axis',(0.,0.,1.));
#26416=DIRECTION('ref_axis',(0.888916624476397,0.458069028345607,0.));
#26417=DIRECTION('center_axis',(0.,0.,-1.));
#26418=DIRECTION('ref_axis',(1.,2.05501931194342E-14,0.));
#26419=DIRECTION('center_axis',(0.,0.,1.));
#26420=DIRECTION('ref_axis',(1.,0.,0.));
#26421=DIRECTION('center_axis',(0.,0.,-1.));
#26422=DIRECTION('ref_axis',(1.,0.,0.));
#26423=DIRECTION('center_axis',(0.,0.,1.));
#26424=DIRECTION('ref_axis',(1.,0.,0.));
#26425=DIRECTION('center_axis',(0.,0.,1.));
#26426=DIRECTION('ref_axis',(1.,0.,0.));
#26427=DIRECTION('center_axis',(0.,0.,1.));
#26428=DIRECTION('ref_axis',(1.,0.,0.));
#26429=DIRECTION('center_axis',(0.,0.,-1.));
#26430=DIRECTION('ref_axis',(1.,-1.15782485934285E-14,0.));
#26431=DIRECTION('center_axis',(0.,0.,1.));
#26432=DIRECTION('ref_axis',(-0.997062746034551,0.0765890362260817,0.));
#26433=DIRECTION('center_axis',(0.,0.,1.));
#26434=DIRECTION('ref_axis',(1.,0.,0.));
#26435=DIRECTION('center_axis',(0.,0.,-1.));
#26436=DIRECTION('ref_axis',(1.,0.,0.));
#26437=DIRECTION('',(-0.866025403784439,-1.06057523872491E-16,0.5));
#26438=DIRECTION('center_axis',(0.5,-0.866025403784439,0.));
#26439=DIRECTION('ref_axis',(0.866025403784439,0.5,0.));
#26440=DIRECTION('',(0.,0.,1.));
#26441=DIRECTION('',(0.,0.,1.));
#26442=DIRECTION('center_axis',(1.,-3.03625687323721E-16,0.));
#26443=DIRECTION('ref_axis',(3.03625687323721E-16,1.,0.));
#26444=DIRECTION('',(0.,0.,1.));
#26445=DIRECTION('center_axis',(0.5,0.866025403784439,0.));
#26446=DIRECTION('ref_axis',(-0.866025403784439,0.5,0.));
#26447=DIRECTION('',(0.,0.,1.));
#26448=DIRECTION('center_axis',(0.,0.,-1.));
#26449=DIRECTION('ref_axis',(1.,0.,0.));
#26450=DIRECTION('',(0.866025403784439,1.06057523872491E-16,0.5));
#26451=DIRECTION('center_axis',(0.,0.,1.));
#26452=DIRECTION('ref_axis',(1.,0.,0.));
#26453=DIRECTION('center_axis',(-0.5,0.866025403784439,0.));
#26454=DIRECTION('ref_axis',(-0.866025403784439,-0.5,0.));
#26455=DIRECTION('',(0.,0.,1.));
#26456=DIRECTION('center_axis',(0.,0.,1.));
#26457=DIRECTION('ref_axis',(1.,0.,0.));
#26458=DIRECTION('center_axis',(0.,0.,1.));
#26459=DIRECTION('ref_axis',(1.,0.,0.));
#26460=DIRECTION('center_axis',(0.,0.,-1.));
#26461=DIRECTION('ref_axis',(1.,0.,0.));
#26462=DIRECTION('center_axis',(0.,0.,1.));
#26463=DIRECTION('ref_axis',(1.,0.,0.));
#26464=DIRECTION('center_axis',(0.,0.,-1.));
#26465=DIRECTION('ref_axis',(1.,0.,0.));
#26466=DIRECTION('center_axis',(0.,0.,1.));
#26467=DIRECTION('ref_axis',(1.,0.,0.));
#26468=DIRECTION('center_axis',(0.,0.,1.));
#26469=DIRECTION('ref_axis',(1.,0.,0.));
#26470=DIRECTION('center_axis',(-0.5,-0.866025403784439,0.));
#26471=DIRECTION('ref_axis',(0.866025403784439,-0.5,0.));
#26472=DIRECTION('',(0.,0.,1.));
#26473=DIRECTION('center_axis',(-1.,-2.0241712488248E-16,0.));
#26474=DIRECTION('ref_axis',(2.0241712488248E-16,-1.,0.));
#26475=DIRECTION('center_axis',(0.,0.,1.));
#26476=DIRECTION('ref_axis',(1.,0.,0.));
#26477=DIRECTION('',(0.,0.,-1.));
#26478=DIRECTION('center_axis',(0.,0.,1.));
#26479=DIRECTION('ref_axis',(1.,0.,0.));
#26480=DIRECTION('center_axis',(0.,0.,1.));
#26481=DIRECTION('ref_axis',(1.,0.,0.));
#26482=DIRECTION('center_axis',(0.,0.,1.));
#26483=DIRECTION('ref_axis',(1.,0.,0.));
#26484=DIRECTION('',(0.,0.,-1.));
#26485=DIRECTION('center_axis',(0.,0.,-1.));
#26486=DIRECTION('ref_axis',(-1.,0.,0.));
#26487=DIRECTION('center_axis',(0.,0.,1.));
#26488=DIRECTION('ref_axis',(1.,0.,0.));
#26489=DIRECTION('center_axis',(0.,0.,1.));
#26490=DIRECTION('ref_axis',(1.,0.,0.));
#26491=DIRECTION('',(0.707106781186548,8.65956056235493E-17,-0.707106781186548));
#26492=DIRECTION('center_axis',(0.,0.,1.));
#26493=DIRECTION('ref_axis',(1.,0.,0.));
#26494=DIRECTION('center_axis',(0.,0.,1.));
#26495=DIRECTION('ref_axis',(1.,0.,0.));
#26496=DIRECTION('center_axis',(0.,0.,1.));
#26497=DIRECTION('ref_axis',(1.,0.,0.));
#26498=DIRECTION('',(0.,0.,-1.));
#26499=DIRECTION('center_axis',(0.,0.,-1.));
#26500=DIRECTION('ref_axis',(1.,0.,0.));
#26501=DIRECTION('center_axis',(0.,0.,1.));
#26502=DIRECTION('ref_axis',(1.,0.,0.));
#26503=DIRECTION('',(-0.707106781186546,-8.65956056235491E-17,-0.707106781186549));
#26504=DIRECTION('center_axis',(0.,0.,1.));
#26505=DIRECTION('ref_axis',(1.,0.,0.));
#26506=DIRECTION('center_axis',(0.,0.,1.));
#26507=DIRECTION('ref_axis',(1.,0.,0.));
#26508=DIRECTION('center_axis',(0.,0.,1.));
#26509=DIRECTION('ref_axis',(1.,0.,0.));
#26510=DIRECTION('',(0.207911690817759,2.54618386665283E-17,-0.978147600733806));
#26511=DIRECTION('axis',(0.,0.,1.));
#26512=DIRECTION('refdir',(1.,0.,0.));
#26513=DIRECTION('center_axis',(0.,0.,-1.));
#26514=DIRECTION('ref_axis',(1.,0.,0.));
#26515=DIRECTION('center_axis',(0.,0.,1.));
#26516=DIRECTION('ref_axis',(1.,0.,0.));
#26517=DIRECTION('',(0.511483859767681,6.26387071680024E-17,0.859292884409708));
#26518=DIRECTION('center_axis',(0.,0.,1.));
#26519=DIRECTION('ref_axis',(1.,0.,0.));
#26520=DIRECTION('center_axis',(0.,0.,-1.));
#26521=DIRECTION('ref_axis',(1.,0.,0.));
#26522=DIRECTION('',(0.857492925712546,1.05012596676537E-16,0.514495755427523));
#26523=DIRECTION('center_axis',(0.,-1.,0.));
#26524=DIRECTION('ref_axis',(0.,0.,-1.));
#26525=DIRECTION('',(0.,0.,1.));
#26526=DIRECTION('',(1.,0.,0.));
#26527=DIRECTION('',(0.,0.,1.));
#26528=DIRECTION('',(1.,0.,0.));
#26529=DIRECTION('center_axis',(1.,0.,0.));
#26530=DIRECTION('ref_axis',(0.,1.,0.));
#26531=DIRECTION('center_axis',(1.,0.,0.));
#26532=DIRECTION('ref_axis',(0.,1.,0.));
#26533=DIRECTION('',(1.,0.,0.));
#26534=DIRECTION('center_axis',(0.,1.,0.));
#26535=DIRECTION('ref_axis',(0.,0.,1.));
#26536=DIRECTION('',(0.,0.,-1.));
#26537=DIRECTION('',(0.,0.,-1.));
#26538=DIRECTION('',(1.,0.,0.));
#26539=DIRECTION('center_axis',(1.,0.,0.));
#26540=DIRECTION('ref_axis',(0.,-1.,0.));
#26541=DIRECTION('center_axis',(1.,0.,0.));
#26542=DIRECTION('ref_axis',(0.,-1.,0.));
#26543=DIRECTION('center_axis',(1.,0.,0.));
#26544=DIRECTION('ref_axis',(0.,0.,-1.));
#26545=DIRECTION('center_axis',(0.,-1.,0.));
#26546=DIRECTION('ref_axis',(0.,0.,-1.));
#26547=DIRECTION('',(0.,0.,1.));
#26548=DIRECTION('',(1.,0.,0.));
#26549=DIRECTION('',(0.,0.,1.));
#26550=DIRECTION('',(1.,0.,0.));
#26551=DIRECTION('center_axis',(1.,0.,0.));
#26552=DIRECTION('ref_axis',(0.,1.,2.77555756156289E-16));
#26553=DIRECTION('center_axis',(1.,0.,0.));
#26554=DIRECTION('ref_axis',(0.,1.,2.77555756156289E-16));
#26555=DIRECTION('',(1.,0.,0.));
#26556=DIRECTION('center_axis',(0.,1.,0.));
#26557=DIRECTION('ref_axis',(0.,0.,1.));
#26558=DIRECTION('',(0.,0.,-1.));
#26559=DIRECTION('',(0.,0.,-1.));
#26560=DIRECTION('',(1.,0.,0.));
#26561=DIRECTION('center_axis',(1.,0.,0.));
#26562=DIRECTION('ref_axis',(0.,-1.,5.55111512312578E-16));
#26563=DIRECTION('center_axis',(1.,0.,0.));
#26564=DIRECTION('ref_axis',(0.,-1.,5.55111512312578E-16));
#26565=DIRECTION('center_axis',(1.,0.,0.));
#26566=DIRECTION('ref_axis',(0.,0.,-1.));
#26567=DIRECTION('center_axis',(0.,0.,-1.));
#26568=DIRECTION('ref_axis',(-1.,0.,0.));
#26569=DIRECTION('center_axis',(0.,0.,1.));
#26570=DIRECTION('ref_axis',(1.,0.,0.));
#26571=DIRECTION('center_axis',(0.,0.,1.));
#26572=DIRECTION('ref_axis',(1.,0.,0.));
#26573=DIRECTION('center_axis',(0.,0.,1.));
#26574=DIRECTION('ref_axis',(1.,0.,0.));
#26575=DIRECTION('',(0.707106781186543,8.65956056235488E-17,-0.707106781186552));
#26576=DIRECTION('center_axis',(0.,0.,1.));
#26577=DIRECTION('ref_axis',(1.,0.,0.));
#26578=DIRECTION('center_axis',(0.,0.,1.));
#26579=DIRECTION('ref_axis',(1.,0.,0.));
#26580=DIRECTION('',(0.,0.,-1.));
#26581=DIRECTION('center_axis',(0.,0.,-1.));
#26582=DIRECTION('ref_axis',(-1.,0.,0.));
#26583=DIRECTION('center_axis',(0.,0.,1.));
#26584=DIRECTION('ref_axis',(1.,0.,0.));
#26585=DIRECTION('center_axis',(0.,0.,1.));
#26586=DIRECTION('ref_axis',(1.,0.,0.));
#26587=DIRECTION('center_axis',(0.,0.,1.));
#26588=DIRECTION('ref_axis',(1.,0.,0.));
#26589=DIRECTION('',(0.707106781186543,8.65956056235488E-17,-0.707106781186552));
#26590=DIRECTION('center_axis',(0.,0.,1.));
#26591=DIRECTION('ref_axis',(1.,0.,0.));
#26592=DIRECTION('center_axis',(0.,0.,1.));
#26593=DIRECTION('ref_axis',(1.,0.,0.));
#26594=DIRECTION('',(0.,0.,-1.));
#26595=DIRECTION('center_axis',(0.,0.,1.));
#26596=DIRECTION('ref_axis',(1.,0.,0.));
#26597=DIRECTION('center_axis',(0.,0.,1.));
#26598=DIRECTION('ref_axis',(1.,0.,0.));
#26599=DIRECTION('center_axis',(0.,0.,1.));
#26600=DIRECTION('ref_axis',(1.,0.,0.));
#26601=DIRECTION('center_axis',(0.,0.,1.));
#26602=DIRECTION('ref_axis',(1.,0.,0.));
#26603=DIRECTION('',(0.,0.,-1.));
#26604=DIRECTION('center_axis',(0.,0.,-1.));
#26605=DIRECTION('ref_axis',(-1.,0.,0.));
#26606=DIRECTION('center_axis',(0.,0.,1.));
#26607=DIRECTION('ref_axis',(1.,0.,0.));
#26608=DIRECTION('center_axis',(0.,0.,1.));
#26609=DIRECTION('ref_axis',(1.,0.,0.));
#26610=DIRECTION('center_axis',(0.,0.,1.));
#26611=DIRECTION('ref_axis',(1.,0.,0.));
#26612=DIRECTION('',(0.,0.,-1.));
#26613=DIRECTION('center_axis',(0.,0.,1.));
#26614=DIRECTION('ref_axis',(1.,0.,0.));
#26615=DIRECTION('center_axis',(0.,0.,1.));
#26616=DIRECTION('ref_axis',(1.,0.,0.));
#26617=DIRECTION('center_axis',(0.,0.,1.));
#26618=DIRECTION('ref_axis',(1.,0.,0.));
#26619=DIRECTION('center_axis',(0.,0.,1.));
#26620=DIRECTION('ref_axis',(1.,0.,0.));
#26621=DIRECTION('',(0.,0.,-1.));
#26622=DIRECTION('center_axis',(0.,0.,-1.));
#26623=DIRECTION('ref_axis',(-1.,0.,0.));
#26624=DIRECTION('center_axis',(0.,0.,1.));
#26625=DIRECTION('ref_axis',(1.,0.,0.));
#26626=DIRECTION('center_axis',(0.,0.,1.));
#26627=DIRECTION('ref_axis',(1.,0.,0.));
#26628=DIRECTION('center_axis',(0.,0.,1.));
#26629=DIRECTION('ref_axis',(1.,0.,0.));
#26630=DIRECTION('',(0.,0.,-1.));
#26631=DIRECTION('center_axis',(0.,0.,-1.));
#26632=DIRECTION('ref_axis',(1.,0.,0.));
#26633=DIRECTION('center_axis',(0.,0.,1.));
#26634=DIRECTION('ref_axis',(1.,0.,0.));
#26635=DIRECTION('',(-0.707106781186546,-8.65956056235491E-17,-0.707106781186549));
#26636=DIRECTION('center_axis',(0.,0.,1.));
#26637=DIRECTION('ref_axis',(1.,0.,0.));
#26638=DIRECTION('axis',(0.,0.,1.));
#26639=DIRECTION('refdir',(1.,0.,0.));
#26640=DIRECTION('center_axis',(0.,0.,1.));
#26641=DIRECTION('ref_axis',(1.,0.,0.));
#26642=DIRECTION('center_axis',(0.,0.,1.));
#26643=DIRECTION('ref_axis',(1.,0.,0.));
#26644=DIRECTION('center_axis',(0.,0.,1.));
#26645=DIRECTION('ref_axis',(1.,0.,0.));
#26646=DIRECTION('center_axis',(0.,0.,1.));
#26647=DIRECTION('ref_axis',(1.,0.,0.));
#26648=DIRECTION('center_axis',(0.,0.,1.));
#26649=DIRECTION('ref_axis',(1.,0.,0.));
#26650=DIRECTION('',(0.,0.,1.));
#26651=DIRECTION('center_axis',(0.,0.,-1.));
#26652=DIRECTION('ref_axis',(-1.,0.,0.));
#26653=DIRECTION('center_axis',(0.,0.,-1.));
#26654=DIRECTION('ref_axis',(1.,0.,0.));
#26655=DIRECTION('center_axis',(0.,0.,1.));
#26656=DIRECTION('ref_axis',(1.,0.,0.));
#26657=DIRECTION('',(0.,0.,-1.));
#26658=DIRECTION('center_axis',(0.,0.,1.));
#26659=DIRECTION('ref_axis',(1.,0.,0.));
#26660=DIRECTION('center_axis',(0.,1.,0.));
#26661=DIRECTION('ref_axis',(-1.,0.,0.));
#26662=DIRECTION('',(0.,0.,1.));
#26663=DIRECTION('',(-1.,0.,0.));
#26664=DIRECTION('',(0.,0.,1.));
#26665=DIRECTION('',(1.,0.,0.));
#26666=DIRECTION('center_axis',(1.,0.,0.));
#26667=DIRECTION('ref_axis',(0.,1.,0.));
#26668=DIRECTION('',(0.,-1.,0.));
#26669=DIRECTION('',(0.,1.,0.));
#26670=DIRECTION('',(0.,0.,1.));
#26671=DIRECTION('center_axis',(0.,-1.,0.));
#26672=DIRECTION('ref_axis',(1.,0.,0.));
#26673=DIRECTION('',(0.,0.,-1.));
#26674=DIRECTION('',(-1.,0.,0.));
#26675=DIRECTION('',(1.,0.,0.));
#26676=DIRECTION('center_axis',(0.,0.,-1.));
#26677=DIRECTION('ref_axis',(-1.,0.,0.));
#26678=DIRECTION('center_axis',(0.,0.,1.));
#26679=DIRECTION('ref_axis',(1.,0.,0.));
#26680=DIRECTION('center_axis',(0.,0.,1.));
#26681=DIRECTION('ref_axis',(1.,0.,0.));
#26682=DIRECTION('center_axis',(0.,0.,1.));
#26683=DIRECTION('ref_axis',(1.,0.,0.));
#26684=DIRECTION('center_axis',(0.,0.,1.));
#26685=DIRECTION('ref_axis',(1.,0.,0.));
#26686=DIRECTION('',(0.,0.,1.));
#26687=DIRECTION('center_axis',(0.,0.,-1.));
#26688=DIRECTION('ref_axis',(1.,0.,0.));
#26689=DIRECTION('center_axis',(0.,0.,1.));
#26690=DIRECTION('ref_axis',(1.,0.,0.));
#26691=DIRECTION('center_axis',(0.,0.,1.));
#26692=DIRECTION('ref_axis',(1.,0.,0.));
#26693=DIRECTION('',(0.,0.,1.));
#26694=DIRECTION('center_axis',(0.,0.,-1.));
#26695=DIRECTION('ref_axis',(1.,0.,0.));
#26696=DIRECTION('center_axis',(0.,0.,1.));
#26697=DIRECTION('ref_axis',(1.,0.,0.));
#26698=DIRECTION('center_axis',(0.,0.,1.));
#26699=DIRECTION('ref_axis',(1.,0.,0.));
#26700=DIRECTION('',(0.,0.,1.));
#26701=DIRECTION('center_axis',(0.,0.,-1.));
#26702=DIRECTION('ref_axis',(1.,0.,0.));
#26703=DIRECTION('center_axis',(0.,0.,1.));
#26704=DIRECTION('ref_axis',(1.,0.,0.));
#26705=DIRECTION('center_axis',(0.,0.,1.));
#26706=DIRECTION('ref_axis',(1.,0.,0.));
#26707=DIRECTION('',(0.,0.,1.));
#26708=DIRECTION('center_axis',(0.,0.,-1.));
#26709=DIRECTION('ref_axis',(1.,0.,0.));
#26710=DIRECTION('center_axis',(0.,0.,1.));
#26711=DIRECTION('ref_axis',(1.,0.,0.));
#26712=DIRECTION('center_axis',(0.,0.,1.));
#26713=DIRECTION('ref_axis',(1.,0.,0.));
#26714=DIRECTION('',(0.,0.,1.));
#26715=DIRECTION('center_axis',(0.,0.,-1.));
#26716=DIRECTION('ref_axis',(1.,0.,0.));
#26717=DIRECTION('center_axis',(0.,0.,1.));
#26718=DIRECTION('ref_axis',(1.,0.,0.));
#26719=DIRECTION('center_axis',(0.,0.,1.));
#26720=DIRECTION('ref_axis',(1.,0.,0.));
#26721=DIRECTION('',(0.,0.,1.));
#26722=DIRECTION('center_axis',(0.,0.,-1.));
#26723=DIRECTION('ref_axis',(1.,0.,0.));
#26724=DIRECTION('center_axis',(0.,0.,1.));
#26725=DIRECTION('ref_axis',(1.,0.,0.));
#26726=DIRECTION('center_axis',(0.,0.,1.));
#26727=DIRECTION('ref_axis',(1.,0.,0.));
#26728=DIRECTION('',(0.,0.,1.));
#26729=DIRECTION('center_axis',(0.,0.,-1.));
#26730=DIRECTION('ref_axis',(1.,0.,0.));
#26731=DIRECTION('center_axis',(0.,0.,1.));
#26732=DIRECTION('ref_axis',(1.,0.,0.));
#26733=DIRECTION('center_axis',(0.,0.,1.));
#26734=DIRECTION('ref_axis',(1.,0.,0.));
#26735=DIRECTION('',(0.,0.,1.));
#26736=DIRECTION('center_axis',(0.,0.,-1.));
#26737=DIRECTION('ref_axis',(1.,0.,0.));
#26738=DIRECTION('center_axis',(0.,0.,1.));
#26739=DIRECTION('ref_axis',(1.,0.,0.));
#26740=DIRECTION('center_axis',(0.,0.,1.));
#26741=DIRECTION('ref_axis',(1.,0.,0.));
#26742=DIRECTION('',(0.,0.,1.));
#26743=DIRECTION('center_axis',(0.,0.,-1.));
#26744=DIRECTION('ref_axis',(1.,0.,0.));
#26745=DIRECTION('center_axis',(0.,0.,1.));
#26746=DIRECTION('ref_axis',(1.,0.,0.));
#26747=DIRECTION('center_axis',(0.,0.,1.));
#26748=DIRECTION('ref_axis',(1.,0.,0.));
#26749=DIRECTION('',(0.,0.,1.));
#26750=DIRECTION('center_axis',(0.,0.,1.));
#26751=DIRECTION('ref_axis',(1.,0.,0.));
#26752=DIRECTION('center_axis',(0.,0.,1.));
#26753=DIRECTION('ref_axis',(1.,0.,0.));
#26754=DIRECTION('center_axis',(0.,0.,1.));
#26755=DIRECTION('ref_axis',(1.,0.,0.));
#26756=DIRECTION('center_axis',(0.,0.,1.));
#26757=DIRECTION('ref_axis',(1.,0.,0.));
#26758=DIRECTION('center_axis',(0.,0.,1.));
#26759=DIRECTION('ref_axis',(1.,0.,0.));
#26760=DIRECTION('',(0.,0.,1.));
#26761=DIRECTION('center_axis',(0.,0.,1.));
#26762=DIRECTION('ref_axis',(1.,0.,0.));
#26763=DIRECTION('center_axis',(0.,0.,1.));
#26764=DIRECTION('ref_axis',(1.,0.,0.));
#26765=DIRECTION('center_axis',(0.,0.,1.));
#26766=DIRECTION('ref_axis',(1.,0.,0.));
#26767=DIRECTION('center_axis',(0.,0.,1.));
#26768=DIRECTION('ref_axis',(1.,0.,0.));
#26769=DIRECTION('center_axis',(0.,0.,1.));
#26770=DIRECTION('ref_axis',(1.,0.,0.));
#26771=DIRECTION('',(0.,0.,1.));
#26772=DIRECTION('center_axis',(0.,0.,1.));
#26773=DIRECTION('ref_axis',(1.,0.,0.));
#26774=DIRECTION('center_axis',(0.,0.,1.));
#26775=DIRECTION('ref_axis',(1.,0.,0.));
#26776=DIRECTION('center_axis',(0.,0.,1.));
#26777=DIRECTION('ref_axis',(1.,0.,0.));
#26778=DIRECTION('center_axis',(0.,0.,1.));
#26779=DIRECTION('ref_axis',(1.,0.,0.));
#26780=DIRECTION('center_axis',(0.,0.,1.));
#26781=DIRECTION('ref_axis',(1.,0.,0.));
#26782=DIRECTION('',(0.,0.,1.));
#26783=DIRECTION('center_axis',(0.,0.,1.));
#26784=DIRECTION('ref_axis',(1.,0.,0.));
#26785=DIRECTION('center_axis',(0.,0.,1.));
#26786=DIRECTION('ref_axis',(1.,0.,0.));
#26787=DIRECTION('center_axis',(0.,0.,1.));
#26788=DIRECTION('ref_axis',(1.,0.,0.));
#26789=DIRECTION('center_axis',(0.,0.,1.));
#26790=DIRECTION('ref_axis',(1.,0.,0.));
#26791=DIRECTION('center_axis',(0.,0.,1.));
#26792=DIRECTION('ref_axis',(1.,0.,0.));
#26793=DIRECTION('',(0.,0.,1.));
#26794=DIRECTION('center_axis',(0.,0.,1.));
#26795=DIRECTION('ref_axis',(1.,0.,0.));
#26796=DIRECTION('center_axis',(0.,0.,1.));
#26797=DIRECTION('ref_axis',(1.,0.,0.));
#26798=DIRECTION('center_axis',(0.,0.,1.));
#26799=DIRECTION('ref_axis',(1.,0.,0.));
#26800=DIRECTION('center_axis',(0.,0.,1.));
#26801=DIRECTION('ref_axis',(1.,0.,0.));
#26802=DIRECTION('center_axis',(0.,0.,1.));
#26803=DIRECTION('ref_axis',(1.,0.,0.));
#26804=DIRECTION('',(0.,0.,1.));
#26805=DIRECTION('center_axis',(0.,0.,1.));
#26806=DIRECTION('ref_axis',(1.,0.,0.));
#26807=DIRECTION('center_axis',(0.,0.,1.));
#26808=DIRECTION('ref_axis',(1.,0.,0.));
#26809=DIRECTION('center_axis',(0.,0.,1.));
#26810=DIRECTION('ref_axis',(1.,0.,0.));
#26811=DIRECTION('center_axis',(0.,0.,1.));
#26812=DIRECTION('ref_axis',(1.,0.,0.));
#26813=DIRECTION('center_axis',(0.,0.,1.));
#26814=DIRECTION('ref_axis',(1.,0.,0.));
#26815=DIRECTION('',(0.,0.,1.));
#26816=DIRECTION('center_axis',(0.,0.,1.));
#26817=DIRECTION('ref_axis',(1.,0.,0.));
#26818=DIRECTION('center_axis',(0.,0.,1.));
#26819=DIRECTION('ref_axis',(1.,0.,0.));
#26820=DIRECTION('center_axis',(0.,0.,1.));
#26821=DIRECTION('ref_axis',(1.,0.,0.));
#26822=DIRECTION('center_axis',(0.,0.,1.));
#26823=DIRECTION('ref_axis',(1.,0.,0.));
#26824=DIRECTION('center_axis',(0.,0.,1.));
#26825=DIRECTION('ref_axis',(1.,0.,0.));
#26826=DIRECTION('',(0.,0.,1.));
#26827=DIRECTION('center_axis',(0.,0.,1.));
#26828=DIRECTION('ref_axis',(1.,0.,0.));
#26829=DIRECTION('center_axis',(0.,0.,1.));
#26830=DIRECTION('ref_axis',(1.,0.,0.));
#26831=DIRECTION('center_axis',(0.,0.,1.));
#26832=DIRECTION('ref_axis',(1.,0.,0.));
#26833=DIRECTION('center_axis',(0.,0.,1.));
#26834=DIRECTION('ref_axis',(1.,0.,0.));
#26835=DIRECTION('center_axis',(0.,0.,1.));
#26836=DIRECTION('ref_axis',(1.,0.,0.));
#26837=DIRECTION('',(0.,0.,1.));
#26838=DIRECTION('center_axis',(0.,0.,1.));
#26839=DIRECTION('ref_axis',(1.,0.,0.));
#26840=DIRECTION('center_axis',(0.,0.,1.));
#26841=DIRECTION('ref_axis',(1.,0.,0.));
#26842=DIRECTION('center_axis',(0.,0.,1.));
#26843=DIRECTION('ref_axis',(1.,0.,0.));
#26844=DIRECTION('center_axis',(0.,0.,-1.));
#26845=DIRECTION('ref_axis',(-1.,0.,0.));
#26846=DIRECTION('center_axis',(0.,0.,1.));
#26847=DIRECTION('ref_axis',(1.,0.,0.));
#26848=DIRECTION('center_axis',(0.,0.,1.));
#26849=DIRECTION('ref_axis',(1.,0.,0.));
#26850=DIRECTION('center_axis',(0.,0.,1.));
#26851=DIRECTION('ref_axis',(1.,0.,0.));
#26852=DIRECTION('center_axis',(0.,0.,1.));
#26853=DIRECTION('ref_axis',(1.,0.,0.));
#26854=DIRECTION('center_axis',(0.,0.,1.));
#26855=DIRECTION('ref_axis',(1.,0.,0.));
#26856=DIRECTION('center_axis',(0.,0.,1.));
#26857=DIRECTION('ref_axis',(1.,0.,0.));
#26858=DIRECTION('center_axis',(0.,0.,1.));
#26859=DIRECTION('ref_axis',(1.,0.,0.));
#26860=DIRECTION('center_axis',(0.,0.,1.));
#26861=DIRECTION('ref_axis',(1.,0.,0.));
#26862=DIRECTION('center_axis',(0.,0.,1.));
#26863=DIRECTION('ref_axis',(1.,0.,0.));
#26864=DIRECTION('center_axis',(0.,0.,1.));
#26865=DIRECTION('ref_axis',(1.,0.,0.));
#26866=DIRECTION('center_axis',(0.,0.,1.));
#26867=DIRECTION('ref_axis',(1.,0.,0.));
#26868=DIRECTION('center_axis',(0.,0.,1.));
#26869=DIRECTION('ref_axis',(1.,0.,0.));
#26870=DIRECTION('',(0.,0.,-1.));
#26871=DIRECTION('center_axis',(0.,0.,1.));
#26872=DIRECTION('ref_axis',(1.,0.,0.));
#26873=DIRECTION('center_axis',(0.,0.,-1.));
#26874=DIRECTION('ref_axis',(1.,0.,0.));
#26875=DIRECTION('',(-0.707106781186546,-8.65956056235492E-17,-0.707106781186549));
#26876=DIRECTION('center_axis',(0.,0.,1.));
#26877=DIRECTION('ref_axis',(1.,0.,0.));
#26878=DIRECTION('',(0.707106781186548,8.65956056235494E-17,-0.707106781186548));
#26879=DIRECTION('center_axis',(0.,0.,1.));
#26880=DIRECTION('ref_axis',(1.,0.,0.));
#26881=DIRECTION('center_axis',(0.,0.,1.));
#26882=DIRECTION('ref_axis',(1.,0.,0.));
#26883=DIRECTION('',(0.,0.,-1.));
#26884=DIRECTION('center_axis',(0.,0.,-1.));
#26885=DIRECTION('ref_axis',(1.,0.,0.));
#26886=DIRECTION('center_axis',(0.,0.,1.));
#26887=DIRECTION('ref_axis',(1.,0.,0.));
#26888=DIRECTION('',(-0.707106781186548,-8.65956056235494E-17,-0.707106781186547));
#26889=DIRECTION('center_axis',(0.,0.,1.));
#26890=DIRECTION('ref_axis',(1.,0.,0.));
#26891=DIRECTION('center_axis',(0.,0.,1.));
#26892=DIRECTION('ref_axis',(1.,0.,0.));
#26893=DIRECTION('center_axis',(0.,0.,1.));
#26894=DIRECTION('ref_axis',(-1.,-1.22464679914735E-16,0.));
#26895=DIRECTION('axis',(0.,0.,1.));
#26896=DIRECTION('refdir',(1.,0.,0.));
#26897=DIRECTION('center_axis',(-0.707106781186548,0.707106781186548,0.));
#26898=DIRECTION('ref_axis',(-0.707106781186548,-0.707106781186548,0.));
#26899=DIRECTION('',(-0.707106781186548,-0.707106781186548,0.));
#26900=DIRECTION('',(0.,0.,1.));
#26901=DIRECTION('',(-0.707106781186548,-0.707106781186548,0.));
#26902=DIRECTION('',(0.,0.,1.));
#26903=DIRECTION('center_axis',(0.977766079918218,0.20969857644095,0.));
#26904=DIRECTION('ref_axis',(-0.20969857644095,0.977766079918218,0.));
#26905=DIRECTION('',(-0.20969857644095,0.977766079918218,0.));
#26906=DIRECTION('',(0.,0.,1.));
#26907=DIRECTION('',(-0.20969857644095,0.977766079918218,0.));
#26908=DIRECTION('center_axis',(-0.407020185134245,-0.913419163852656,0.));
#26909=DIRECTION('ref_axis',(0.913419163852656,-0.407020185134245,0.));
#26910=DIRECTION('',(0.913419163852656,-0.407020185134245,0.));
#26911=DIRECTION('',(0.,0.,1.));
#26912=DIRECTION('',(0.913419163852656,-0.407020185134245,0.));
#26913=DIRECTION('center_axis',(-0.707106781186548,0.707106781186548,0.));
#26914=DIRECTION('ref_axis',(-0.707106781186548,-0.707106781186548,0.));
#26915=DIRECTION('',(-0.707106781186548,-0.707106781186548,0.));
#26916=DIRECTION('',(0.,0.,1.));
#26917=DIRECTION('',(-0.707106781186548,-0.707106781186548,0.));
#26918=DIRECTION('center_axis',(0.,0.,1.));
#26919=DIRECTION('ref_axis',(0.707106781186547,0.707106781186548,0.));
#26920=DIRECTION('center_axis',(0.,0.,-1.));
#26921=DIRECTION('ref_axis',(0.707106781186547,0.707106781186548,0.));
#26922=DIRECTION('',(0.,0.,1.));
#26923=DIRECTION('center_axis',(0.,0.,-1.));
#26924=DIRECTION('ref_axis',(0.707106781186547,0.707106781186548,0.));
#26925=DIRECTION('center_axis',(-0.707106781186547,-0.707106781186548,0.));
#26926=DIRECTION('ref_axis',(0.707106781186548,-0.707106781186547,0.));
#26927=DIRECTION('',(0.707106781186548,-0.707106781186547,0.));
#26928=DIRECTION('',(0.,0.,1.));
#26929=DIRECTION('',(0.707106781186548,-0.707106781186547,0.));
#26930=DIRECTION('center_axis',(0.,0.,1.));
#26931=DIRECTION('ref_axis',(0.707106781186548,0.707106781186547,0.));
#26932=DIRECTION('center_axis',(0.,0.,1.));
#26933=DIRECTION('ref_axis',(0.707106781186548,0.707106781186547,0.));
#26934=DIRECTION('center_axis',(0.,0.,1.));
#26935=DIRECTION('ref_axis',(0.707106781186548,0.707106781186547,0.));
#26936=DIRECTION('center_axis',(0.,0.,1.));
#26937=DIRECTION('ref_axis',(1.,0.,0.));
#26938=DIRECTION('center_axis',(0.,0.,-1.));
#26939=DIRECTION('ref_axis',(-1.,0.,0.));
#26940=DIRECTION('center_axis',(0.,0.,-1.));
#26941=DIRECTION('ref_axis',(-1.,0.,0.));
#26942=DIRECTION('',(-0.707106781186552,8.65956056235499E-17,0.707106781186543));
#26943=DIRECTION('center_axis',(0.,0.,1.));
#26944=DIRECTION('ref_axis',(-1.,0.,0.));
#26945=DIRECTION('center_axis',(0.,0.,1.));
#26946=DIRECTION('ref_axis',(-1.,0.,0.));
#26947=DIRECTION('center_axis',(0.,0.,1.));
#26948=DIRECTION('ref_axis',(1.,0.,0.));
#26949=DIRECTION('center_axis',(0.,0.,1.));
#26950=DIRECTION('ref_axis',(1.,0.,0.));
#26951=DIRECTION('center_axis',(0.,0.,1.));
#26952=DIRECTION('ref_axis',(1.,0.,0.));
#26953=DIRECTION('',(0.,0.,1.));
#26954=DIRECTION('center_axis',(0.,0.,-1.));
#26955=DIRECTION('ref_axis',(1.,0.,0.));
#26956=DIRECTION('center_axis',(0.,0.,-1.));
#26957=DIRECTION('ref_axis',(-1.,0.,0.));
#26958=DIRECTION('center_axis',(0.,0.,-1.));
#26959=DIRECTION('ref_axis',(-1.,0.,0.));
#26960=DIRECTION('',(-0.707106781186546,8.65956056235491E-17,0.707106781186549));
#26961=DIRECTION('center_axis',(0.,0.,1.));
#26962=DIRECTION('ref_axis',(-1.,0.,0.));
#26963=DIRECTION('center_axis',(0.,0.,1.));
#26964=DIRECTION('ref_axis',(-1.,0.,0.));
#26965=DIRECTION('center_axis',(0.,0.,1.));
#26966=DIRECTION('ref_axis',(1.,0.,0.));
#26967=DIRECTION('center_axis',(0.,0.,1.));
#26968=DIRECTION('ref_axis',(1.,0.,0.));
#26969=DIRECTION('center_axis',(0.,0.,1.));
#26970=DIRECTION('ref_axis',(1.,0.,0.));
#26971=DIRECTION('',(0.,0.,1.));
#26972=DIRECTION('center_axis',(0.,0.,-1.));
#26973=DIRECTION('ref_axis',(1.,0.,0.));
#26974=DIRECTION('center_axis',(0.,0.,-1.));
#26975=DIRECTION('ref_axis',(-1.,0.,0.));
#26976=DIRECTION('center_axis',(0.,0.,-1.));
#26977=DIRECTION('ref_axis',(-1.,0.,0.));
#26978=DIRECTION('',(-0.707106781186546,8.65956056235491E-17,0.707106781186549));
#26979=DIRECTION('center_axis',(0.,0.,1.));
#26980=DIRECTION('ref_axis',(-1.,0.,0.));
#26981=DIRECTION('center_axis',(0.,0.,1.));
#26982=DIRECTION('ref_axis',(-1.,0.,0.));
#26983=DIRECTION('center_axis',(0.,0.,1.));
#26984=DIRECTION('ref_axis',(1.,0.,0.));
#26985=DIRECTION('center_axis',(0.,0.,1.));
#26986=DIRECTION('ref_axis',(1.,0.,0.));
#26987=DIRECTION('center_axis',(0.,0.,1.));
#26988=DIRECTION('ref_axis',(1.,0.,0.));
#26989=DIRECTION('',(0.,0.,1.));
#26990=DIRECTION('center_axis',(0.,0.,-1.));
#26991=DIRECTION('ref_axis',(1.,0.,0.));
#26992=DIRECTION('center_axis',(0.,0.,-1.));
#26993=DIRECTION('ref_axis',(-1.,0.,0.));
#26994=DIRECTION('center_axis',(0.,0.,-1.));
#26995=DIRECTION('ref_axis',(-1.,0.,0.));
#26996=DIRECTION('',(-0.707106781186552,8.65956056235499E-17,0.707106781186543));
#26997=DIRECTION('center_axis',(0.,0.,1.));
#26998=DIRECTION('ref_axis',(-1.,0.,0.));
#26999=DIRECTION('center_axis',(0.,0.,1.));
#27000=DIRECTION('ref_axis',(-1.,0.,0.));
#27001=DIRECTION('center_axis',(0.,0.,1.));
#27002=DIRECTION('ref_axis',(1.,0.,0.));
#27003=DIRECTION('center_axis',(0.,0.,1.));
#27004=DIRECTION('ref_axis',(1.,0.,0.));
#27005=DIRECTION('center_axis',(0.,0.,1.));
#27006=DIRECTION('ref_axis',(1.,0.,0.));
#27007=DIRECTION('',(0.,0.,1.));
#27008=DIRECTION('center_axis',(0.,0.,-1.));
#27009=DIRECTION('ref_axis',(1.,0.,0.));
#27010=DIRECTION('center_axis',(0.,0.,-1.));
#27011=DIRECTION('ref_axis',(-1.,0.,0.));
#27012=DIRECTION('center_axis',(0.,0.,-1.));
#27013=DIRECTION('ref_axis',(-1.,0.,0.));
#27014=DIRECTION('',(-0.707106781186546,8.65956056235491E-17,0.707106781186549));
#27015=DIRECTION('center_axis',(0.,0.,1.));
#27016=DIRECTION('ref_axis',(-1.,0.,0.));
#27017=DIRECTION('center_axis',(0.,0.,1.));
#27018=DIRECTION('ref_axis',(-1.,0.,0.));
#27019=DIRECTION('center_axis',(0.,0.,1.));
#27020=DIRECTION('ref_axis',(1.,0.,0.));
#27021=DIRECTION('center_axis',(0.,0.,1.));
#27022=DIRECTION('ref_axis',(1.,0.,0.));
#27023=DIRECTION('center_axis',(0.,0.,1.));
#27024=DIRECTION('ref_axis',(1.,0.,0.));
#27025=DIRECTION('',(0.,0.,1.));
#27026=DIRECTION('center_axis',(0.,0.,-1.));
#27027=DIRECTION('ref_axis',(1.,0.,0.));
#27028=DIRECTION('center_axis',(0.,0.,-1.));
#27029=DIRECTION('ref_axis',(-1.,0.,0.));
#27030=DIRECTION('center_axis',(0.,0.,-1.));
#27031=DIRECTION('ref_axis',(-1.,0.,0.));
#27032=DIRECTION('',(-0.707106781186546,8.65956056235491E-17,0.707106781186549));
#27033=DIRECTION('center_axis',(0.,0.,1.));
#27034=DIRECTION('ref_axis',(-1.,0.,0.));
#27035=DIRECTION('center_axis',(0.,0.,1.));
#27036=DIRECTION('ref_axis',(-1.,0.,0.));
#27037=DIRECTION('center_axis',(0.,0.,1.));
#27038=DIRECTION('ref_axis',(1.,0.,0.));
#27039=DIRECTION('center_axis',(0.,0.,1.));
#27040=DIRECTION('ref_axis',(1.,0.,0.));
#27041=DIRECTION('center_axis',(0.,0.,1.));
#27042=DIRECTION('ref_axis',(1.,0.,0.));
#27043=DIRECTION('',(0.,0.,1.));
#27044=DIRECTION('center_axis',(0.,0.,-1.));
#27045=DIRECTION('ref_axis',(1.,0.,0.));
#27046=DIRECTION('center_axis',(0.,0.,1.));
#27047=DIRECTION('ref_axis',(1.,0.,0.));
#27048=DIRECTION('center_axis',(0.,0.,1.));
#27049=DIRECTION('ref_axis',(1.,0.,0.));
#27050=DIRECTION('center_axis',(0.,0.,1.));
#27051=DIRECTION('ref_axis',(1.,0.,0.));
#27052=DIRECTION('',(0.,0.,1.));
#27053=DIRECTION('center_axis',(0.,0.,1.));
#27054=DIRECTION('ref_axis',(1.,0.,0.));
#27055=DIRECTION('center_axis',(0.,0.,1.));
#27056=DIRECTION('ref_axis',(-1.,1.22464679914735E-16,0.));
#27057=DIRECTION('center_axis',(1.22464679914735E-16,-1.,0.));
#27058=DIRECTION('ref_axis',(-1.,-1.22464679914735E-16,0.));
#27059=DIRECTION('center_axis',(0.,0.,-1.));
#27060=DIRECTION('ref_axis',(-1.,1.22464679914735E-16,0.));
#27061=DIRECTION('center_axis',(0.,0.,-1.));
#27062=DIRECTION('ref_axis',(-1.,1.22464679914735E-16,0.));
#27063=DIRECTION('center_axis',(0.,0.,-1.));
#27064=DIRECTION('ref_axis',(-1.,1.22464679914735E-16,0.));
#27065=DIRECTION('center_axis',(0.,0.,-1.));
#27066=DIRECTION('ref_axis',(-1.,1.22464679914735E-16,0.));
#27067=DIRECTION('center_axis',(0.,0.,-1.));
#27068=DIRECTION('ref_axis',(-1.,1.22464679914735E-16,0.));
#27069=DIRECTION('center_axis',(0.,0.,-1.));
#27070=DIRECTION('ref_axis',(-1.,1.22464679914735E-16,0.));
#27071=DIRECTION('center_axis',(0.,0.,1.));
#27072=DIRECTION('ref_axis',(1.,0.,0.));
#27073=DIRECTION('center_axis',(0.,0.,1.));
#27074=DIRECTION('ref_axis',(1.,0.,0.));
#27075=DIRECTION('',(0.,0.,1.));
#27076=DIRECTION('center_axis',(0.,0.,1.));
#27077=DIRECTION('ref_axis',(1.,0.,0.));
#27078=DIRECTION('center_axis',(0.,0.,-1.));
#27079=DIRECTION('ref_axis',(-1.,0.,0.));
#27080=DIRECTION('center_axis',(0.,0.,1.));
#27081=DIRECTION('ref_axis',(1.,0.,0.));
#27082=DIRECTION('center_axis',(0.,0.,1.));
#27083=DIRECTION('ref_axis',(1.,0.,0.));
#27084=DIRECTION('center_axis',(0.,0.,1.));
#27085=DIRECTION('ref_axis',(1.,0.,0.));
#27086=DIRECTION('center_axis',(0.,0.,1.));
#27087=DIRECTION('ref_axis',(1.,0.,0.));
#27088=DIRECTION('center_axis',(0.,0.,1.));
#27089=DIRECTION('ref_axis',(1.,0.,0.));
#27090=DIRECTION('center_axis',(0.,0.,1.));
#27091=DIRECTION('ref_axis',(1.,0.,0.));
#27092=DIRECTION('center_axis',(0.,0.,1.));
#27093=DIRECTION('ref_axis',(1.,0.,0.));
#27094=DIRECTION('center_axis',(0.,0.,1.));
#27095=DIRECTION('ref_axis',(1.,0.,0.));
#27096=DIRECTION('center_axis',(0.,0.,1.));
#27097=DIRECTION('ref_axis',(1.,0.,0.));
#27098=DIRECTION('',(0.,0.,1.));
#27099=DIRECTION('center_axis',(0.,0.,1.));
#27100=DIRECTION('ref_axis',(1.,0.,0.));
#27101=DIRECTION('',(0.,0.,1.));
#27102=DIRECTION('center_axis',(0.,0.,1.));
#27103=DIRECTION('ref_axis',(1.,0.,0.));
#27104=DIRECTION('',(0.,0.,1.));
#27105=DIRECTION('center_axis',(0.,0.,1.));
#27106=DIRECTION('ref_axis',(1.,0.,0.));
#27107=DIRECTION('',(0.,0.,1.));
#27108=DIRECTION('center_axis',(1.,0.,0.));
#27109=DIRECTION('ref_axis',(0.,0.,1.));
#27110=DIRECTION('center_axis',(1.,0.,0.));
#27111=DIRECTION('ref_axis',(0.,0.,1.));
#27112=DIRECTION('',(-0.707106781186547,-8.65956056235493E-17,0.707106781186547));
#27113=DIRECTION('center_axis',(-1.,0.,0.));
#27114=DIRECTION('ref_axis',(0.,0.,1.));
#27115=DIRECTION('center_axis',(-1.,0.,0.));
#27116=DIRECTION('ref_axis',(0.,0.,1.));
#27117=DIRECTION('',(-1.,0.,0.));
#27118=DIRECTION('center_axis',(1.,0.,0.));
#27119=DIRECTION('ref_axis',(0.,0.,-1.));
#27120=DIRECTION('center_axis',(-1.,0.,0.));
#27121=DIRECTION('ref_axis',(0.,0.,-1.));
#27122=DIRECTION('center_axis',(-1.,0.,0.));
#27123=DIRECTION('ref_axis',(0.,0.,-1.));
#27124=DIRECTION('',(-0.707106781186548,-8.65956056235493E-17,0.707106781186548));
#27125=DIRECTION('center_axis',(1.,0.,0.));
#27126=DIRECTION('ref_axis',(0.,0.,-1.));
#27127=DIRECTION('center_axis',(1.,0.,0.));
#27128=DIRECTION('ref_axis',(0.,0.,-1.));
#27129=DIRECTION('',(-1.,0.,0.));
#27130=DIRECTION('center_axis',(0.,0.,1.));
#27131=DIRECTION('ref_axis',(-1.,0.,0.));
#27132=DIRECTION('center_axis',(0.,0.,-1.));
#27133=DIRECTION('ref_axis',(-1.,0.,0.));
#27134=DIRECTION('center_axis',(0.,0.,-1.));
#27135=DIRECTION('ref_axis',(-1.,0.,0.));
#27136=DIRECTION('',(0.707106781186547,-8.65956056235493E-17,0.707106781186547));
#27137=DIRECTION('center_axis',(0.,0.,1.));
#27138=DIRECTION('ref_axis',(-1.,0.,0.));
#27139=DIRECTION('center_axis',(0.,0.,1.));
#27140=DIRECTION('ref_axis',(1.,0.,0.));
#27141=DIRECTION('center_axis',(0.,0.,1.));
#27142=DIRECTION('ref_axis',(1.,0.,0.));
#27143=DIRECTION('center_axis',(0.,0.,1.));
#27144=DIRECTION('ref_axis',(1.,0.,0.));
#27145=DIRECTION('',(0.,0.,-1.));
#27146=DIRECTION('center_axis',(0.,0.,1.));
#27147=DIRECTION('ref_axis',(1.,0.,0.));
#27148=DIRECTION('center_axis',(0.,0.,-1.));
#27149=DIRECTION('ref_axis',(-1.,0.,0.));
#27150=DIRECTION('center_axis',(0.,0.,-1.));
#27151=DIRECTION('ref_axis',(-1.,0.,0.));
#27152=DIRECTION('',(-0.707106781186549,8.65956056235495E-17,0.707106781186546));
#27153=DIRECTION('center_axis',(0.,0.,1.));
#27154=DIRECTION('ref_axis',(-1.,0.,0.));
#27155=DIRECTION('center_axis',(0.,0.,1.));
#27156=DIRECTION('ref_axis',(-1.,0.,0.));
#27157=DIRECTION('center_axis',(0.,0.,1.));
#27158=DIRECTION('ref_axis',(1.,0.,0.));
#27159=DIRECTION('center_axis',(0.,0.,1.));
#27160=DIRECTION('ref_axis',(1.,0.,0.));
#27161=DIRECTION('',(0.,0.,-1.));
#27162=DIRECTION('center_axis',(0.,0.,-1.));
#27163=DIRECTION('ref_axis',(-1.,0.,0.));
#27164=DIRECTION('center_axis',(0.,0.,1.));
#27165=DIRECTION('ref_axis',(1.,0.,0.));
#27166=DIRECTION('center_axis',(0.,0.,1.));
#27167=DIRECTION('ref_axis',(1.,0.,0.));
#27168=DIRECTION('center_axis',(0.,0.,-1.));
#27169=DIRECTION('ref_axis',(-1.,1.22464679914735E-16,0.));
#27170=DIRECTION('center_axis',(1.22464679914735E-16,-1.,0.));
#27171=DIRECTION('ref_axis',(-1.,-1.22464679914735E-16,0.));
#27172=DIRECTION('center_axis',(0.,0.,1.));
#27173=DIRECTION('ref_axis',(-1.,0.,0.));
#27174=DIRECTION('center_axis',(0.,0.,1.));
#27175=DIRECTION('ref_axis',(1.,0.,0.));
#27176=DIRECTION('',(0.,0.,-1.));
#27177=DIRECTION('center_axis',(0.,0.,1.));
#27178=DIRECTION('ref_axis',(1.,0.,0.));
#27179=DIRECTION('',(0.821369965673296,1.00588809937757E-16,-0.570395809495344));
#27180=DIRECTION('center_axis',(0.,0.,1.));
#27181=DIRECTION('ref_axis',(1.,0.,0.));
#27182=DIRECTION('center_axis',(0.,0.,1.));
#27183=DIRECTION('ref_axis',(1.,0.,0.));
#27184=DIRECTION('center_axis',(0.,0.,1.));
#27185=DIRECTION('ref_axis',(1.,0.,0.));
#27186=DIRECTION('',(0.707106781186549,8.65956056235495E-17,-0.707106781186546));
#27187=DIRECTION('center_axis',(0.,0.,1.));
#27188=DIRECTION('ref_axis',(1.,0.,0.));
#27189=DIRECTION('',(0.,0.,-1.));
#27190=DIRECTION('center_axis',(0.,0.,1.));
#27191=DIRECTION('ref_axis',(1.,0.,0.));
#27192=DIRECTION('center_axis',(0.,0.,1.));
#27193=DIRECTION('ref_axis',(1.,0.,0.));
#27194=DIRECTION('',(0.707106781186547,8.65956056235492E-17,-0.707106781186548));
#27195=DIRECTION('center_axis',(0.,0.,1.));
#27196=DIRECTION('ref_axis',(1.,0.,0.));
#27197=DIRECTION('center_axis',(0.,0.,1.));
#27198=DIRECTION('ref_axis',(1.,0.,0.));
#27199=DIRECTION('',(0.,0.,-1.));
#27200=DIRECTION('center_axis',(0.,0.,-1.));
#27201=DIRECTION('ref_axis',(1.,0.,0.));
#27202=DIRECTION('',(-0.447213595499957,-5.47678698264201E-17,-0.894427190999917));
#27203=DIRECTION('center_axis',(0.,0.,1.));
#27204=DIRECTION('ref_axis',(1.,0.,0.));
#27205=DIRECTION('center_axis',(0.,0.,1.));
#27206=DIRECTION('ref_axis',(1.,0.,0.));
#27207=DIRECTION('center_axis',(0.,0.,1.));
#27208=DIRECTION('ref_axis',(1.,0.,0.));
#27209=DIRECTION('',(0.,0.,-1.));
#27210=DIRECTION('center_axis',(0.,0.,1.));
#27211=DIRECTION('ref_axis',(1.,0.,0.));
#27212=DIRECTION('center_axis',(0.,0.,1.));
#27213=DIRECTION('ref_axis',(1.,0.,0.));
#27214=DIRECTION('center_axis',(0.,0.,1.));
#27215=DIRECTION('ref_axis',(1.,0.,0.));
#27216=DIRECTION('center_axis',(0.,0.,1.));
#27217=DIRECTION('ref_axis',(1.,0.,0.));
#27218=DIRECTION('',(0.,0.,-1.));
#27219=DIRECTION('center_axis',(0.,0.,1.));
#27220=DIRECTION('ref_axis',(1.,0.,0.));
#27221=DIRECTION('center_axis',(0.,0.,-1.));
#27222=DIRECTION('ref_axis',(-1.,0.,0.));
#27223=DIRECTION('center_axis',(0.,0.,1.));
#27224=DIRECTION('ref_axis',(1.,0.,0.));
#27225=DIRECTION('center_axis',(0.,0.,1.));
#27226=DIRECTION('ref_axis',(1.,0.,0.));
#27227=DIRECTION('',(0.,0.,-1.));
#27228=DIRECTION('center_axis',(0.,0.,1.));
#27229=DIRECTION('ref_axis',(1.,0.,0.));
#27230=DIRECTION('center_axis',(0.,0.,1.));
#27231=DIRECTION('ref_axis',(1.,0.,0.));
#27232=DIRECTION('center_axis',(0.,0.,1.));
#27233=DIRECTION('ref_axis',(1.,0.,0.));
#27234=DIRECTION('center_axis',(0.,0.,1.));
#27235=DIRECTION('ref_axis',(1.,0.,0.));
#27236=DIRECTION('',(0.,0.,-1.));
#27237=DIRECTION('center_axis',(0.,0.,1.));
#27238=DIRECTION('ref_axis',(1.,0.,0.));
#27239=DIRECTION('center_axis',(0.,0.,1.));
#27240=DIRECTION('ref_axis',(1.,0.,0.));
#27241=DIRECTION('axis',(0.,0.,1.));
#27242=DIRECTION('refdir',(1.,0.,0.));
#27243=DIRECTION('center_axis',(0.,0.,1.));
#27244=DIRECTION('ref_axis',(1.,0.,0.));
#27245=DIRECTION('center_axis',(0.,0.,1.));
#27246=DIRECTION('ref_axis',(1.,0.,0.));
#27247=DIRECTION('',(0.707106781186553,8.659560562355E-17,-0.707106781186542));
#27248=DIRECTION('center_axis',(0.,0.,-1.));
#27249=DIRECTION('ref_axis',(1.,0.,0.));
#27250=DIRECTION('center_axis',(0.,0.,1.));
#27251=DIRECTION('ref_axis',(1.,0.,0.));
#27252=DIRECTION('center_axis',(0.,0.,1.));
#27253=DIRECTION('ref_axis',(1.,0.,0.));
#27254=DIRECTION('',(0.,0.,1.));
#27255=DIRECTION('center_axis',(0.,0.,1.));
#27256=DIRECTION('ref_axis',(1.,0.,0.));
#27257=DIRECTION('',(1.,0.,0.));
#27258=DIRECTION('center_axis',(0.,0.,1.));
#27259=DIRECTION('ref_axis',(1.,0.,0.));
#27260=DIRECTION('',(-1.,0.,0.));
#27261=DIRECTION('center_axis',(0.,0.,1.));
#27262=DIRECTION('ref_axis',(1.,0.,0.));
#27263=DIRECTION('center_axis',(0.,0.,1.));
#27264=DIRECTION('ref_axis',(1.,0.,0.));
#27265=DIRECTION('center_axis',(0.,0.,1.));
#27266=DIRECTION('ref_axis',(1.,0.,0.));
#27267=DIRECTION('center_axis',(0.,0.,1.));
#27268=DIRECTION('ref_axis',(1.,0.,0.));
#27269=DIRECTION('center_axis',(0.,0.,1.));
#27270=DIRECTION('ref_axis',(-1.,0.,0.));
#27271=DIRECTION('center_axis',(0.,0.,-1.));
#27272=DIRECTION('ref_axis',(1.,0.,0.));
#27273=DIRECTION('center_axis',(0.,0.,1.));
#27274=DIRECTION('ref_axis',(1.,0.,0.));
#27275=DIRECTION('center_axis',(0.,0.,1.));
#27276=DIRECTION('ref_axis',(1.,0.,0.));
#27277=DIRECTION('center_axis',(0.,0.,-1.));
#27278=DIRECTION('ref_axis',(1.,0.,0.));
#27279=DIRECTION('center_axis',(0.,0.,-1.));
#27280=DIRECTION('ref_axis',(1.,0.,0.));
#27281=DIRECTION('',(0.70710678118655,-8.65956056235496E-17,0.707106781186545));
#27282=DIRECTION('center_axis',(0.,0.,-1.));
#27283=DIRECTION('ref_axis',(-1.,0.,0.));
#27284=DIRECTION('',(-1.,0.,0.));
#27285=DIRECTION('center_axis',(0.,0.,1.));
#27286=DIRECTION('ref_axis',(1.,0.,0.));
#27287=DIRECTION('',(1.,0.,0.));
#27288=DIRECTION('center_axis',(0.,0.,1.));
#27289=DIRECTION('ref_axis',(1.,0.,0.));
#27290=DIRECTION('center_axis',(0.,0.,-1.));
#27291=DIRECTION('ref_axis',(1.,0.,0.));
#27292=DIRECTION('center_axis',(0.,0.,-1.));
#27293=DIRECTION('ref_axis',(1.,0.,0.));
#27294=DIRECTION('center_axis',(0.,0.,-1.));
#27295=DIRECTION('ref_axis',(1.,0.,0.));
#27296=DIRECTION('center_axis',(0.,0.,-1.));
#27297=DIRECTION('ref_axis',(0.819152044288992,0.573576436351046,0.));
#27298=DIRECTION('center_axis',(0.,0.,1.));
#27299=DIRECTION('ref_axis',(-0.819152044288992,-0.573576436351046,0.));
#27300=DIRECTION('center_axis',(0.,0.,1.));
#27301=DIRECTION('ref_axis',(0.819152044288992,0.573576436351046,0.));
#27302=DIRECTION('center_axis',(0.,0.,1.));
#27303=DIRECTION('ref_axis',(-0.819152044288991,0.573576436351046,0.));
#27304=DIRECTION('center_axis',(0.,0.,-1.));
#27305=DIRECTION('ref_axis',(-0.819152044288992,-0.573576436351046,0.));
#27306=DIRECTION('center_axis',(0.,0.,1.));
#27307=DIRECTION('ref_axis',(0.819152044288991,0.573576436351047,0.));
#27308=DIRECTION('center_axis',(0.,0.,1.));
#27309=DIRECTION('ref_axis',(-0.819152044288992,-0.573576436351046,0.));
#27310=DIRECTION('center_axis',(0.,0.,1.));
#27311=DIRECTION('ref_axis',(0.819152044288992,-0.573576436351046,0.));
#27312=DIRECTION('center_axis',(0.,0.,-1.));
#27313=DIRECTION('ref_axis',(-1.,0.,0.));
#27314=DIRECTION('center_axis',(0.,0.,-1.));
#27315=DIRECTION('ref_axis',(1.,0.,0.));
#27316=DIRECTION('center_axis',(0.,0.,-1.));
#27317=DIRECTION('ref_axis',(1.,0.,0.));
#27318=DIRECTION('center_axis',(0.,0.,1.));
#27319=DIRECTION('ref_axis',(1.,0.,0.));
#27320=DIRECTION('',(0.707106781186547,8.65956056235493E-17,-0.707106781186547));
#27321=DIRECTION('center_axis',(0.,0.,-1.));
#27322=DIRECTION('ref_axis',(1.,0.,0.));
#27323=DIRECTION('center_axis',(0.,0.,1.));
#27324=DIRECTION('ref_axis',(1.,0.,0.));
#27325=DIRECTION('center_axis',(0.,0.,1.));
#27326=DIRECTION('ref_axis',(1.,0.,0.));
#27327=DIRECTION('',(0.,0.,1.));
#27328=DIRECTION('center_axis',(0.,0.,-1.));
#27329=DIRECTION('ref_axis',(1.,0.,0.));
#27330=DIRECTION('',(0.707106781186545,-8.6595605623549E-17,0.70710678118655));
#27331=DIRECTION('center_axis',(0.,0.,1.));
#27332=DIRECTION('ref_axis',(1.,0.,0.));
#27333=DIRECTION('',(0.707106781186548,8.65956056235493E-17,-0.707106781186548));
#27334=DIRECTION('center_axis',(0.,0.,-1.));
#27335=DIRECTION('ref_axis',(1.,0.,0.));
#27336=DIRECTION('center_axis',(0.,0.,1.));
#27337=DIRECTION('ref_axis',(1.,0.,0.));
#27338=DIRECTION('center_axis',(0.,0.,1.));
#27339=DIRECTION('ref_axis',(1.,0.,0.));
#27340=DIRECTION('',(0.,0.,1.));
#27341=DIRECTION('center_axis',(0.,0.,-1.));
#27342=DIRECTION('ref_axis',(1.,0.,0.));
#27343=DIRECTION('',(0.707106781186545,-8.6595605623549E-17,0.70710678118655));
#27344=DIRECTION('center_axis',(0.,0.,1.));
#27345=DIRECTION('ref_axis',(1.,0.,0.));
#27346=DIRECTION('',(0.707106781186553,8.659560562355E-17,-0.707106781186542));
#27347=DIRECTION('center_axis',(0.,0.,-1.));
#27348=DIRECTION('ref_axis',(1.,0.,0.));
#27349=DIRECTION('center_axis',(0.,0.,1.));
#27350=DIRECTION('ref_axis',(1.,0.,0.));
#27351=DIRECTION('center_axis',(0.,0.,1.));
#27352=DIRECTION('ref_axis',(1.,0.,0.));
#27353=DIRECTION('',(0.,0.,1.));
#27354=DIRECTION('center_axis',(0.,0.,-1.));
#27355=DIRECTION('ref_axis',(1.,0.,0.));
#27356=DIRECTION('',(0.70710678118655,-8.65956056235496E-17,0.707106781186545));
#27357=DIRECTION('center_axis',(0.,0.,1.));
#27358=DIRECTION('ref_axis',(1.,0.,0.));
#27359=DIRECTION('',(0.707106781186547,8.65956056235493E-17,-0.707106781186547));
#27360=DIRECTION('center_axis',(0.,0.,-1.));
#27361=DIRECTION('ref_axis',(1.,0.,0.));
#27362=DIRECTION('center_axis',(0.,0.,1.));
#27363=DIRECTION('ref_axis',(1.,0.,0.));
#27364=DIRECTION('center_axis',(0.,0.,1.));
#27365=DIRECTION('ref_axis',(1.,0.,0.));
#27366=DIRECTION('',(0.,0.,1.));
#27367=DIRECTION('center_axis',(0.,0.,-1.));
#27368=DIRECTION('ref_axis',(1.,0.,0.));
#27369=DIRECTION('',(0.707106781186545,-8.6595605623549E-17,0.70710678118655));
#27370=DIRECTION('center_axis',(0.,0.,1.));
#27371=DIRECTION('ref_axis',(1.,0.,0.));
#27372=DIRECTION('',(0.707106781186547,8.65956056235493E-17,-0.707106781186547));
#27373=DIRECTION('center_axis',(0.,0.,-1.));
#27374=DIRECTION('ref_axis',(1.,0.,0.));
#27375=DIRECTION('center_axis',(0.,0.,1.));
#27376=DIRECTION('ref_axis',(1.,0.,0.));
#27377=DIRECTION('center_axis',(0.,0.,1.));
#27378=DIRECTION('ref_axis',(1.,0.,0.));
#27379=DIRECTION('',(0.,0.,1.));
#27380=DIRECTION('center_axis',(0.,0.,-1.));
#27381=DIRECTION('ref_axis',(1.,0.,0.));
#27382=DIRECTION('',(0.707106781186545,-8.6595605623549E-17,0.70710678118655));
#27383=DIRECTION('center_axis',(0.,0.,1.));
#27384=DIRECTION('ref_axis',(1.,0.,0.));
#27385=DIRECTION('',(0.,0.,1.));
#27386=DIRECTION('center_axis',(0.,1.,0.));
#27387=DIRECTION('ref_axis',(0.,0.,1.));
#27388=DIRECTION('center_axis',(0.,1.,0.));
#27389=DIRECTION('ref_axis',(0.,0.,1.));
#27390=DIRECTION('',(8.65956056235493E-17,-0.707106781186547,0.707106781186547));
#27391=DIRECTION('center_axis',(0.,-1.,0.));
#27392=DIRECTION('ref_axis',(0.,0.,1.));
#27393=DIRECTION('center_axis',(0.,1.,0.));
#27394=DIRECTION('ref_axis',(0.,0.,1.));
#27395=DIRECTION('center_axis',(0.,1.,0.));
#27396=DIRECTION('ref_axis',(1.,0.,0.));
#27397=DIRECTION('',(0.,1.,0.));
#27398=DIRECTION('center_axis',(0.,1.,0.));
#27399=DIRECTION('ref_axis',(1.,0.,0.));
#27400=DIRECTION('',(0.,0.,1.));
#27401=DIRECTION('',(0.,0.,-1.));
#27402=DIRECTION('center_axis',(0.,-1.,0.));
#27403=DIRECTION('ref_axis',(0.,0.,1.));
#27404=DIRECTION('center_axis',(0.,-1.,0.));
#27405=DIRECTION('ref_axis',(0.,0.,1.));
#27406=DIRECTION('',(-8.65956056235493E-17,0.707106781186547,0.707106781186547));
#27407=DIRECTION('center_axis',(0.,1.,0.));
#27408=DIRECTION('ref_axis',(0.,0.,1.));
#27409=DIRECTION('center_axis',(0.,1.,0.));
#27410=DIRECTION('ref_axis',(0.,0.,1.));
#27411=DIRECTION('',(0.,1.,0.));
#27412=DIRECTION('center_axis',(0.,1.,0.));
#27413=DIRECTION('ref_axis',(1.,0.,0.));
#27414=DIRECTION('center_axis',(0.,1.,0.));
#27415=DIRECTION('ref_axis',(1.,0.,0.));
#27416=DIRECTION('',(0.,0.,1.));
#27417=DIRECTION('',(0.,0.,-1.));
#27418=DIRECTION('center_axis',(0.,1.,0.));
#27419=DIRECTION('ref_axis',(0.,0.,1.));
#27420=DIRECTION('center_axis',(0.,1.,0.));
#27421=DIRECTION('ref_axis',(1.,0.,0.));
#27422=DIRECTION('',(0.,1.,0.));
#27423=DIRECTION('',(0.,-1.,0.));
#27424=DIRECTION('center_axis',(0.,1.,0.));
#27425=DIRECTION('ref_axis',(1.,0.,0.));
#27426=DIRECTION('',(0.,1.,0.));
#27427=DIRECTION('center_axis',(0.,1.,0.));
#27428=DIRECTION('ref_axis',(-1.22464679914735E-16,0.,-1.));
#27429=DIRECTION('center_axis',(0.,1.,0.));
#27430=DIRECTION('ref_axis',(1.,0.,0.));
#27431=DIRECTION('center_axis',(0.,1.,0.));
#27432=DIRECTION('ref_axis',(1.,0.,0.));
#27433=DIRECTION('center_axis',(0.,1.,0.));
#27434=DIRECTION('ref_axis',(0.,0.,1.));
#27435=DIRECTION('center_axis',(0.,-1.,0.));
#27436=DIRECTION('ref_axis',(0.,0.,1.));
#27437=DIRECTION('',(1.04972719113862E-16,0.515038074910055,0.857167300702112));
#27438=DIRECTION('center_axis',(0.,0.,1.));
#27439=DIRECTION('ref_axis',(-0.819152044288992,-0.573576436351046,0.));
#27440=DIRECTION('center_axis',(0.,0.,-1.));
#27441=DIRECTION('ref_axis',(-0.819152044288992,-0.573576436351046,0.));
#27442=DIRECTION('',(0.,0.,1.));
#27443=DIRECTION('',(0.,0.,1.));
#27444=DIRECTION('center_axis',(0.,0.,-1.));
#27445=DIRECTION('ref_axis',(-0.819152044288992,-0.573576436351046,0.));
#27446=DIRECTION('center_axis',(0.,0.,1.));
#27447=DIRECTION('ref_axis',(1.,0.,0.));
#27448=DIRECTION('center_axis',(0.,0.,1.));
#27449=DIRECTION('ref_axis',(-0.819152044288992,-0.573576436351046,0.));
#27450=DIRECTION('center_axis',(0.,0.,1.));
#27451=DIRECTION('ref_axis',(0.819152044288991,0.573576436351047,0.));
#27452=DIRECTION('center_axis',(0.,0.,1.));
#27453=DIRECTION('ref_axis',(-1.,-1.22464679914735E-16,0.));
#27454=DIRECTION('center_axis',(0.,0.,1.));
#27455=DIRECTION('ref_axis',(1.,0.,0.));
#27456=DIRECTION('center_axis',(0.,0.,1.));
#27457=DIRECTION('ref_axis',(-1.,-1.22464679914735E-16,0.));
#27458=DIRECTION('center_axis',(0.,0.,1.));
#27459=DIRECTION('ref_axis',(1.,0.,0.));
#27460=DIRECTION('center_axis',(0.,0.,-1.));
#27461=DIRECTION('ref_axis',(-1.,-1.22464679914735E-16,0.));
#27462=DIRECTION('center_axis',(0.,1.,0.));
#27463=DIRECTION('ref_axis',(0.,0.,1.));
#27464=DIRECTION('',(0.,-1.,0.));
#27465=DIRECTION('',(0.,1.,0.));
#27466=DIRECTION('center_axis',(0.,1.,0.));
#27467=DIRECTION('ref_axis',(1.,0.,0.));
#27468=DIRECTION('',(0.,1.,0.));
#27469=DIRECTION('center_axis',(0.,1.,0.));
#27470=DIRECTION('ref_axis',(1.,0.,0.));
#27471=DIRECTION('center_axis',(0.,1.,0.));
#27472=DIRECTION('ref_axis',(-7.6571373978539E-16,0.,-1.));
#27473=DIRECTION('center_axis',(0.,1.,0.));
#27474=DIRECTION('ref_axis',(1.,0.,0.));
#27475=DIRECTION('center_axis',(0.,1.,0.));
#27476=DIRECTION('ref_axis',(1.,0.,0.));
#27477=DIRECTION('center_axis',(0.,1.,0.));
#27478=DIRECTION('ref_axis',(0.,0.,1.));
#27479=DIRECTION('',(-1.04972719113862E-16,0.515038074910055,-0.857167300702112));
#27480=DIRECTION('center_axis',(0.,-1.,0.));
#27481=DIRECTION('ref_axis',(0.,0.,-1.));
#27482=DIRECTION('center_axis',(0.,0.,1.));
#27483=DIRECTION('ref_axis',(0.819152044288992,0.573576436351046,0.));
#27484=DIRECTION('center_axis',(0.,0.,-1.));
#27485=DIRECTION('ref_axis',(0.819152044288992,0.573576436351046,0.));
#27486=DIRECTION('',(0.,0.,1.));
#27487=DIRECTION('',(0.,0.,1.));
#27488=DIRECTION('center_axis',(0.,0.,-1.));
#27489=DIRECTION('ref_axis',(0.819152044288992,0.573576436351046,0.));
#27490=DIRECTION('center_axis',(0.,0.,1.));
#27491=DIRECTION('ref_axis',(1.,0.,0.));
#27492=DIRECTION('center_axis',(0.,0.,1.));
#27493=DIRECTION('ref_axis',(0.819152044288992,0.573576436351046,0.));
#27494=DIRECTION('center_axis',(0.,0.,1.));
#27495=DIRECTION('ref_axis',(-0.819152044288992,-0.573576436351046,0.));
#27496=DIRECTION('center_axis',(0.,0.,1.));
#27497=DIRECTION('ref_axis',(-0.819152044288991,0.573576436351046,0.));
#27498=DIRECTION('',(0.,0.,1.));
#27499=DIRECTION('center_axis',(0.,0.,1.));
#27500=DIRECTION('ref_axis',(-0.819152044288991,0.573576436351046,0.));
#27501=DIRECTION('center_axis',(0.,0.,1.));
#27502=DIRECTION('ref_axis',(0.819152044288992,0.573576436351046,0.));
#27503=DIRECTION('center_axis',(0.,0.,1.));
#27504=DIRECTION('ref_axis',(0.819152044288992,0.573576436351046,0.));
#27505=DIRECTION('',(0.,0.,1.));
#27506=DIRECTION('center_axis',(0.,0.,1.));
#27507=DIRECTION('ref_axis',(-0.819152044288992,-0.573576436351046,0.));
#27508=DIRECTION('center_axis',(0.,0.,1.));
#27509=DIRECTION('ref_axis',(1.,0.,0.));
#27510=DIRECTION('center_axis',(0.,0.,1.));
#27511=DIRECTION('ref_axis',(0.819152044288992,-0.573576436351046,0.));
#27512=DIRECTION('',(0.,0.,1.));
#27513=DIRECTION('center_axis',(0.,0.,1.));
#27514=DIRECTION('ref_axis',(0.819152044288992,-0.573576436351046,0.));
#27515=DIRECTION('center_axis',(0.,0.,1.));
#27516=DIRECTION('ref_axis',(-0.819152044288992,-0.573576436351046,0.));
#27517=DIRECTION('center_axis',(0.,0.,1.));
#27518=DIRECTION('ref_axis',(-0.819152044288992,-0.573576436351046,0.));
#27519=DIRECTION('',(0.,0.,1.));
#27520=DIRECTION('center_axis',(0.,0.,1.));
#27521=DIRECTION('ref_axis',(0.819152044288991,0.573576436351047,0.));
#27522=DIRECTION('center_axis',(0.,0.,1.));
#27523=DIRECTION('ref_axis',(1.,0.,0.));
#27524=DIRECTION('center_axis',(0.,0.,-1.));
#27525=DIRECTION('ref_axis',(-1.,0.,0.));
#27526=DIRECTION('',(-0.707106781186547,8.65956056235493E-17,0.707106781186547));
#27527=DIRECTION('center_axis',(0.,0.,1.));
#27528=DIRECTION('ref_axis',(-1.,0.,0.));
#27529=DIRECTION('center_axis',(0.,0.,1.));
#27530=DIRECTION('ref_axis',(-1.,0.,0.));
#27531=DIRECTION('center_axis',(0.,0.,1.));
#27532=DIRECTION('ref_axis',(1.,0.,0.));
#27533=DIRECTION('center_axis',(0.,0.,-1.));
#27534=DIRECTION('ref_axis',(-1.,0.,0.));
#27535=DIRECTION('center_axis',(0.,0.,-1.));
#27536=DIRECTION('ref_axis',(-1.,0.,0.));
#27537=DIRECTION('',(0.,0.,-1.));
#27538=DIRECTION('center_axis',(0.,0.,1.));
#27539=DIRECTION('ref_axis',(-1.,0.,0.));
#27540=DIRECTION('',(0.707106781186549,-8.65956056235495E-17,0.707106781186546));
#27541=DIRECTION('center_axis',(0.,0.,1.));
#27542=DIRECTION('ref_axis',(1.,0.,0.));
#27543=DIRECTION('center_axis',(0.,0.,1.));
#27544=DIRECTION('ref_axis',(1.,0.,0.));
#27545=DIRECTION('center_axis',(0.,0.,1.));
#27546=DIRECTION('ref_axis',(1.,0.,0.));
#27547=DIRECTION('center_axis',(0.,0.,1.));
#27548=DIRECTION('ref_axis',(1.,0.,0.));
#27549=DIRECTION('center_axis',(0.,0.,-1.));
#27550=DIRECTION('ref_axis',(1.,0.,0.));
#27551=DIRECTION('axis',(0.,0.,1.));
#27552=DIRECTION('refdir',(1.,0.,0.));
#27553=DIRECTION('',(0.,0.,-1.));
#27554=DIRECTION('',(0.,0.,-1.));
#27555=DIRECTION('',(0.,0.,-1.));
#27556=DIRECTION('',(0.,0.,-1.));
#27557=DIRECTION('',(0.,0.,-1.));
#27558=DIRECTION('',(0.,0.,-1.));
#27559=DIRECTION('',(0.,0.,-1.));
#27560=DIRECTION('',(0.,0.,-1.));
#27561=DIRECTION('',(0.,0.,-1.));
#27562=DIRECTION('',(0.,0.,-1.));
#27563=DIRECTION('center_axis',(-1.,0.,0.));
#27564=DIRECTION('ref_axis',(0.,1.,0.));
#27565=DIRECTION('',(0.,1.,0.));
#27566=DIRECTION('',(0.,1.,0.));
#27567=DIRECTION('',(0.,0.,-1.));
#27568=DIRECTION('',(0.,0.,-1.));
#27569=DIRECTION('',(0.,0.,-1.));
#27570=DIRECTION('center_axis',(1.,0.,0.));
#27571=DIRECTION('ref_axis',(0.,-1.,0.));
#27572=DIRECTION('',(0.,-1.,0.));
#27573=DIRECTION('',(0.,0.,-1.));
#27574=DIRECTION('',(0.,-1.,0.));
#27575=DIRECTION('',(0.,0.,-1.));
#27576=DIRECTION('',(0.,0.,-1.));
#27577=DIRECTION('',(0.,0.,-1.));
#27578=DIRECTION('',(0.,0.,-1.));
#27579=DIRECTION('',(0.,0.,-1.));
#27580=DIRECTION('',(0.,0.,-1.));
#27581=DIRECTION('',(0.,0.,-1.));
#27582=DIRECTION('center_axis',(-0.135112645952214,-0.990830244241561,0.));
#27583=DIRECTION('ref_axis',(-0.990830244241561,0.135112645952214,0.));
#27584=DIRECTION('',(-0.990830244241561,0.135112645952214,0.));
#27585=DIRECTION('',(0.,0.,-1.));
#27586=DIRECTION('',(-0.990830244241561,0.135112645952214,0.));
#27587=DIRECTION('',(0.,0.,-1.));
#27588=DIRECTION('',(0.,0.,-1.));
#27589=DIRECTION('',(0.,0.,-1.));
#27590=DIRECTION('',(0.,0.,-1.));
#27591=DIRECTION('',(0.,0.,-1.));
#27592=DIRECTION('',(0.,0.,-1.));
#27593=DIRECTION('',(0.,0.,-1.));
#27594=DIRECTION('',(0.,0.,-1.));
#27595=DIRECTION('',(0.,0.,-1.));
#27596=DIRECTION('',(0.,0.,-1.));
#27597=DIRECTION('',(0.,0.,-1.));
#27598=DIRECTION('',(0.,0.,-1.));
#27599=DIRECTION('',(0.,0.,-1.));
#27600=DIRECTION('',(0.,0.,-1.));
#27601=DIRECTION('',(0.,0.,-1.));
#27602=DIRECTION('center_axis',(-1.57407341770917E-15,-1.,0.));
#27603=DIRECTION('ref_axis',(-1.,1.57407341770917E-15,0.));
#27604=DIRECTION('',(-1.,1.57407341770917E-15,0.));
#27605=DIRECTION('',(-1.,1.57407341770917E-15,0.));
#27606=DIRECTION('center_axis',(0.,0.,1.));
#27607=DIRECTION('ref_axis',(1.,0.,0.));
#27608=DIRECTION('',(0.,0.,-1.));
#27609=DIRECTION('',(0.,0.,-1.));
#27610=DIRECTION('',(0.,0.,-1.));
#27611=DIRECTION('',(0.,0.,-1.));
#27612=DIRECTION('',(0.,0.,-1.));
#27613=DIRECTION('',(0.,0.,-1.));
#27614=DIRECTION('',(0.,0.,-1.));
#27615=DIRECTION('',(0.,0.,-1.));
#27616=DIRECTION('',(0.,0.,-1.));
#27617=DIRECTION('',(0.,0.,-1.));
#27618=DIRECTION('',(0.,0.,-1.));
#27619=DIRECTION('',(0.,0.,-1.));
#27620=DIRECTION('',(0.,0.,-1.));
#27621=DIRECTION('',(0.,0.,-1.));
#27622=DIRECTION('',(0.,0.,-1.));
#27623=DIRECTION('',(0.,0.,-1.));
#27624=DIRECTION('',(0.,0.,-1.));
#27625=DIRECTION('',(0.,0.,-1.));
#27626=DIRECTION('',(0.,0.,-1.));
#27627=DIRECTION('',(0.,0.,-1.));
#27628=DIRECTION('center_axis',(0.,0.,1.));
#27629=DIRECTION('ref_axis',(1.,0.,0.));
#27630=DIRECTION('',(0.,0.,-1.));
#27631=DIRECTION('',(0.,0.,-1.));
#27632=DIRECTION('',(0.,0.,-1.));
#27633=DIRECTION('center_axis',(-1.,0.,0.));
#27634=DIRECTION('ref_axis',(0.,1.,0.));
#27635=DIRECTION('',(0.,1.,0.));
#27636=DIRECTION('',(0.,0.,-1.));
#27637=DIRECTION('',(0.,1.,0.));
#27638=DIRECTION('',(0.,0.,-1.));
#27639=DIRECTION('',(0.,0.,-1.));
#27640=DIRECTION('center_axis',(-1.,0.,0.));
#27641=DIRECTION('ref_axis',(0.,1.,0.));
#27642=DIRECTION('',(0.,1.,0.));
#27643=DIRECTION('',(0.,0.,-1.));
#27644=DIRECTION('',(0.,1.,0.));
#27645=DIRECTION('center_axis',(0.,-1.,0.));
#27646=DIRECTION('ref_axis',(-1.,0.,0.));
#27647=DIRECTION('',(-1.,0.,0.));
#27648=DIRECTION('',(0.,0.,-1.));
#27649=DIRECTION('',(-1.,0.,0.));
#27650=DIRECTION('center_axis',(1.,0.,0.));
#27651=DIRECTION('ref_axis',(0.,-1.,0.));
#27652=DIRECTION('',(0.,-1.,0.));
#27653=DIRECTION('',(0.,0.,-1.));
#27654=DIRECTION('',(0.,-1.,0.));
#27655=DIRECTION('center_axis',(0.,1.,0.));
#27656=DIRECTION('ref_axis',(1.,0.,0.));
#27657=DIRECTION('',(1.,0.,0.));
#27658=DIRECTION('',(1.,0.,0.));
#27659=DIRECTION('center_axis',(0.,0.,1.));
#27660=DIRECTION('ref_axis',(1.,0.,0.));
#27661=DIRECTION('center_axis',(-0.946846713341944,-0.321685096691715,0.));
#27662=DIRECTION('ref_axis',(-0.321685096691715,0.946846713341944,0.));
#27663=DIRECTION('',(-0.321685096691715,0.946846713341944,0.));
#27664=DIRECTION('',(0.,0.,-1.));
#27665=DIRECTION('',(-0.321685096691715,0.946846713341944,0.));
#27666=DIRECTION('',(0.,0.,-1.));
#27667=DIRECTION('center_axis',(0.,-1.,0.));
#27668=DIRECTION('ref_axis',(-1.,0.,0.));
#27669=DIRECTION('',(-1.,0.,0.));
#27670=DIRECTION('',(0.,0.,-1.));
#27671=DIRECTION('',(-1.,0.,0.));
#27672=DIRECTION('center_axis',(0.944683612861939,-0.327983035521831,0.));
#27673=DIRECTION('ref_axis',(-0.327983035521831,-0.944683612861939,0.));
#27674=DIRECTION('',(-0.327983035521831,-0.944683612861939,0.));
#27675=DIRECTION('',(0.,0.,-1.));
#27676=DIRECTION('',(-0.327983035521831,-0.944683612861939,0.));
#27677=DIRECTION('center_axis',(-1.,0.,0.));
#27678=DIRECTION('ref_axis',(0.,1.,0.));
#27679=DIRECTION('',(0.,1.,0.));
#27680=DIRECTION('',(0.,0.,-1.));
#27681=DIRECTION('',(0.,1.,0.));
#27682=DIRECTION('center_axis',(0.,-1.,0.));
#27683=DIRECTION('ref_axis',(-1.,0.,0.));
#27684=DIRECTION('',(-1.,0.,0.));
#27685=DIRECTION('',(0.,0.,-1.));
#27686=DIRECTION('',(-1.,0.,0.));
#27687=DIRECTION('center_axis',(1.,0.,0.));
#27688=DIRECTION('ref_axis',(0.,-1.,0.));
#27689=DIRECTION('',(0.,-1.,0.));
#27690=DIRECTION('',(0.,0.,-1.));
#27691=DIRECTION('',(0.,-1.,0.));
#27692=DIRECTION('center_axis',(0.,1.,0.));
#27693=DIRECTION('ref_axis',(1.,0.,0.));
#27694=DIRECTION('',(1.,0.,0.));
#27695=DIRECTION('',(0.,0.,-1.));
#27696=DIRECTION('',(1.,0.,0.));
#27697=DIRECTION('center_axis',(-0.945579690186978,0.325390610660323,0.));
#27698=DIRECTION('ref_axis',(0.325390610660323,0.945579690186978,0.));
#27699=DIRECTION('',(0.325390610660323,0.945579690186978,0.));
#27700=DIRECTION('',(0.,0.,-1.));
#27701=DIRECTION('',(0.325390610660323,0.945579690186978,0.));
#27702=DIRECTION('',(0.,0.,-1.));
#27703=DIRECTION('',(0.,0.,-1.));
#27704=DIRECTION('center_axis',(0.948408837989887,0.317049958244238,0.));
#27705=DIRECTION('ref_axis',(0.317049958244238,-0.948408837989887,0.));
#27706=DIRECTION('',(0.317049958244238,-0.948408837989887,0.));
#27707=DIRECTION('',(0.,0.,-1.));
#27708=DIRECTION('',(0.317049958244238,-0.948408837989887,0.));
#27709=DIRECTION('center_axis',(0.,1.,0.));
#27710=DIRECTION('ref_axis',(1.,0.,0.));
#27711=DIRECTION('',(1.,0.,0.));
#27712=DIRECTION('',(0.,0.,-1.));
#27713=DIRECTION('',(1.,0.,0.));
#27714=DIRECTION('center_axis',(-1.,0.,0.));
#27715=DIRECTION('ref_axis',(0.,1.,0.));
#27716=DIRECTION('',(0.,1.,0.));
#27717=DIRECTION('',(0.,0.,-1.));
#27718=DIRECTION('',(0.,1.,0.));
#27719=DIRECTION('center_axis',(0.,-1.,0.));
#27720=DIRECTION('ref_axis',(-1.,0.,0.));
#27721=DIRECTION('',(-1.,0.,0.));
#27722=DIRECTION('',(0.,0.,-1.));
#27723=DIRECTION('',(-1.,0.,0.));
#27724=DIRECTION('center_axis',(1.,0.,0.));
#27725=DIRECTION('ref_axis',(0.,-1.,0.));
#27726=DIRECTION('',(0.,-1.,0.));
#27727=DIRECTION('',(0.,-1.,0.));
#27728=DIRECTION('center_axis',(0.,0.,1.));
#27729=DIRECTION('ref_axis',(1.,0.,0.));
#27730=DIRECTION('',(0.,0.,-1.));
#27731=DIRECTION('',(0.,0.,-1.));
#27732=DIRECTION('',(0.,0.,-1.));
#27733=DIRECTION('',(0.,0.,-1.));
#27734=DIRECTION('',(0.,0.,-1.));
#27735=DIRECTION('',(0.,0.,-1.));
#27736=DIRECTION('',(0.,0.,-1.));
#27737=DIRECTION('',(0.,0.,-1.));
#27738=DIRECTION('',(0.,0.,-1.));
#27739=DIRECTION('',(0.,0.,-1.));
#27740=DIRECTION('',(0.,0.,-1.));
#27741=DIRECTION('',(0.,0.,-1.));
#27742=DIRECTION('center_axis',(-0.175032773131272,-0.984562607623292,0.));
#27743=DIRECTION('ref_axis',(-0.984562607623292,0.175032773131272,0.));
#27744=DIRECTION('',(-0.984562607623292,0.175032773131272,0.));
#27745=DIRECTION('',(0.,0.,-1.));
#27746=DIRECTION('',(-0.984562607623292,0.175032773131272,0.));
#27747=DIRECTION('',(0.,0.,-1.));
#27748=DIRECTION('',(0.,0.,-1.));
#27749=DIRECTION('',(0.,0.,-1.));
#27750=DIRECTION('',(0.,0.,-1.));
#27751=DIRECTION('',(0.,0.,-1.));
#27752=DIRECTION('',(0.,0.,-1.));
#27753=DIRECTION('',(0.,0.,-1.));
#27754=DIRECTION('center_axis',(-0.992083762154323,0.125577899607075,0.));
#27755=DIRECTION('ref_axis',(0.125577899607075,0.992083762154323,0.));
#27756=DIRECTION('',(0.125577899607075,0.992083762154323,0.));
#27757=DIRECTION('',(0.,0.,-1.));
#27758=DIRECTION('',(0.125577899607075,0.992083762154323,0.));
#27759=DIRECTION('',(0.,0.,-1.));
#27760=DIRECTION('',(0.,0.,-1.));
#27761=DIRECTION('',(0.,0.,-1.));
#27762=DIRECTION('',(0.,0.,-1.));
#27763=DIRECTION('',(0.,0.,-1.));
#27764=DIRECTION('',(0.,0.,-1.));
#27765=DIRECTION('',(0.,0.,-1.));
#27766=DIRECTION('center_axis',(-0.132163748744578,0.99122789686216,0.));
#27767=DIRECTION('ref_axis',(0.99122789686216,0.132163748744578,0.));
#27768=DIRECTION('',(0.99122789686216,0.132163748744578,0.));
#27769=DIRECTION('',(0.,0.,-1.));
#27770=DIRECTION('',(0.99122789686216,0.132163748744578,0.));
#27771=DIRECTION('',(0.,0.,-1.));
#27772=DIRECTION('center_axis',(0.,0.,1.));
#27773=DIRECTION('ref_axis',(1.,0.,0.));
#27774=DIRECTION('center_axis',(0.,1.,0.));
#27775=DIRECTION('ref_axis',(1.,0.,0.));
#27776=DIRECTION('',(1.,0.,0.));
#27777=DIRECTION('',(0.,0.,-1.));
#27778=DIRECTION('',(1.,0.,0.));
#27779=DIRECTION('',(0.,0.,-1.));
#27780=DIRECTION('center_axis',(-1.,0.,0.));
#27781=DIRECTION('ref_axis',(0.,1.,0.));
#27782=DIRECTION('',(0.,1.,0.));
#27783=DIRECTION('',(0.,0.,-1.));
#27784=DIRECTION('',(0.,1.,0.));
#27785=DIRECTION('center_axis',(0.,-1.,0.));
#27786=DIRECTION('ref_axis',(-1.,0.,0.));
#27787=DIRECTION('',(-1.,0.,0.));
#27788=DIRECTION('',(0.,0.,-1.));
#27789=DIRECTION('',(-1.,0.,0.));
#27790=DIRECTION('center_axis',(1.,0.,0.));
#27791=DIRECTION('ref_axis',(0.,-1.,0.));
#27792=DIRECTION('',(0.,-1.,0.));
#27793=DIRECTION('',(0.,-1.,0.));
#27794=DIRECTION('center_axis',(0.,0.,-1.));
#27795=DIRECTION('ref_axis',(-1.,0.,0.));
#27796=DIRECTION('',(0.,0.,-1.));
#27797=DIRECTION('',(0.,0.,-1.));
#27798=DIRECTION('',(0.,0.,-1.));
#27799=DIRECTION('center_axis',(-0.935759711779643,-0.352638287498792,0.));
#27800=DIRECTION('ref_axis',(-0.352638287498792,0.935759711779643,0.));
#27801=DIRECTION('',(-0.352638287498792,0.935759711779643,0.));
#27802=DIRECTION('',(0.,0.,-1.));
#27803=DIRECTION('',(-0.352638287498792,0.935759711779643,0.));
#27804=DIRECTION('center_axis',(0.,1.,0.));
#27805=DIRECTION('ref_axis',(1.,0.,0.));
#27806=DIRECTION('',(1.,0.,0.));
#27807=DIRECTION('',(0.,0.,-1.));
#27808=DIRECTION('',(1.,0.,0.));
#27809=DIRECTION('center_axis',(0.936507962144564,-0.35064631302758,0.));
#27810=DIRECTION('ref_axis',(-0.35064631302758,-0.936507962144564,0.));
#27811=DIRECTION('',(-0.35064631302758,-0.936507962144564,0.));
#27812=DIRECTION('',(-0.35064631302758,-0.936507962144564,0.));
#27813=DIRECTION('center_axis',(0.,-1.,0.));
#27814=DIRECTION('ref_axis',(-1.,0.,0.));
#27815=DIRECTION('',(-1.,0.,0.));
#27816=DIRECTION('',(0.,0.,-1.));
#27817=DIRECTION('',(-1.,0.,0.));
#27818=DIRECTION('',(0.,0.,-1.));
#27819=DIRECTION('center_axis',(-0.933183037129681,-0.359401473582713,0.));
#27820=DIRECTION('ref_axis',(-0.359401473582713,0.933183037129681,0.));
#27821=DIRECTION('',(-0.359401473582713,0.933183037129681,0.));
#27822=DIRECTION('',(0.,0.,-1.));
#27823=DIRECTION('',(-0.359401473582713,0.933183037129681,0.));
#27824=DIRECTION('center_axis',(0.,-1.,0.));
#27825=DIRECTION('ref_axis',(-1.,0.,0.));
#27826=DIRECTION('',(-1.,0.,0.));
#27827=DIRECTION('',(0.,0.,-1.));
#27828=DIRECTION('',(-1.,0.,0.));
#27829=DIRECTION('center_axis',(0.925486618796678,0.378780303643539,0.));
#27830=DIRECTION('ref_axis',(0.378780303643539,-0.925486618796678,0.));
#27831=DIRECTION('',(0.378780303643539,-0.925486618796678,0.));
#27832=DIRECTION('',(0.,0.,-1.));
#27833=DIRECTION('',(0.378780303643539,-0.925486618796678,0.));
#27834=DIRECTION('center_axis',(0.,1.,0.));
#27835=DIRECTION('ref_axis',(1.,0.,0.));
#27836=DIRECTION('',(1.,0.,0.));
#27837=DIRECTION('',(0.,0.,-1.));
#27838=DIRECTION('',(1.,0.,0.));
#27839=DIRECTION('center_axis',(-0.93352603941556,0.35850960061496,0.));
#27840=DIRECTION('ref_axis',(0.35850960061496,0.93352603941556,0.));
#27841=DIRECTION('',(0.35850960061496,0.93352603941556,0.));
#27842=DIRECTION('',(0.,0.,-1.));
#27843=DIRECTION('',(0.35850960061496,0.93352603941556,0.));
#27844=DIRECTION('center_axis',(0.,-1.,0.));
#27845=DIRECTION('ref_axis',(-1.,0.,0.));
#27846=DIRECTION('',(-1.,0.,0.));
#27847=DIRECTION('',(0.,0.,-1.));
#27848=DIRECTION('',(-1.,0.,0.));
#27849=DIRECTION('center_axis',(0.940102154683871,-0.340892855247427,0.));
#27850=DIRECTION('ref_axis',(-0.340892855247427,-0.940102154683871,0.));
#27851=DIRECTION('',(-0.340892855247427,-0.940102154683871,0.));
#27852=DIRECTION('',(-0.340892855247427,-0.940102154683871,0.));
#27853=DIRECTION('center_axis',(0.,0.,1.));
#27854=DIRECTION('ref_axis',(1.,0.,0.));
#27855=DIRECTION('',(0.,0.,-1.));
#27856=DIRECTION('',(0.,0.,-1.));
#27857=DIRECTION('',(0.,0.,-1.));
#27858=DIRECTION('',(0.,0.,-1.));
#27859=DIRECTION('',(0.,0.,-1.));
#27860=DIRECTION('',(0.,0.,-1.));
#27861=DIRECTION('',(0.,0.,-1.));
#27862=DIRECTION('',(0.,0.,-1.));
#27863=DIRECTION('',(0.,0.,-1.));
#27864=DIRECTION('',(0.,0.,-1.));
#27865=DIRECTION('',(0.,0.,-1.));
#27866=DIRECTION('',(0.,0.,-1.));
#27867=DIRECTION('',(0.,0.,-1.));
#27868=DIRECTION('',(0.,0.,-1.));
#27869=DIRECTION('center_axis',(0.0750566189565801,-0.99717927372705,0.));
#27870=DIRECTION('ref_axis',(-0.99717927372705,-0.0750566189565801,0.));
#27871=DIRECTION('',(-0.99717927372705,-0.0750566189565801,0.));
#27872=DIRECTION('',(0.,0.,-1.));
#27873=DIRECTION('',(-0.99717927372705,-0.0750566189565801,0.));
#27874=DIRECTION('',(0.,0.,-1.));
#27875=DIRECTION('',(0.,0.,-1.));
#27876=DIRECTION('',(0.,0.,-1.));
#27877=DIRECTION('',(0.,0.,-1.));
#27878=DIRECTION('',(0.,0.,-1.));
#27879=DIRECTION('',(0.,0.,-1.));
#27880=DIRECTION('',(0.,0.,-1.));
#27881=DIRECTION('',(0.,0.,-1.));
#27882=DIRECTION('',(0.,0.,-1.));
#27883=DIRECTION('',(0.,0.,-1.));
#27884=DIRECTION('',(0.,0.,-1.));
#27885=DIRECTION('',(0.,0.,-1.));
#27886=DIRECTION('',(0.,0.,-1.));
#27887=DIRECTION('',(0.,0.,-1.));
#27888=DIRECTION('',(0.,0.,-1.));
#27889=DIRECTION('',(0.,0.,-1.));
#27890=DIRECTION('',(0.,0.,-1.));
#27891=DIRECTION('',(0.,0.,-1.));
#27892=DIRECTION('center_axis',(-0.0870993597080284,0.996199629360728,0.));
#27893=DIRECTION('ref_axis',(0.996199629360728,0.0870993597080284,0.));
#27894=DIRECTION('',(0.996199629360728,0.0870993597080284,0.));
#27895=DIRECTION('',(0.,0.,-1.));
#27896=DIRECTION('',(0.996199629360728,0.0870993597080284,0.));
#27897=DIRECTION('',(0.,0.,-1.));
#27898=DIRECTION('center_axis',(0.,0.,1.));
#27899=DIRECTION('ref_axis',(1.,0.,0.));
#27900=DIRECTION('',(0.,0.,-1.));
#27901=DIRECTION('',(0.,0.,-1.));
#27902=DIRECTION('',(0.,0.,-1.));
#27903=DIRECTION('',(0.,0.,-1.));
#27904=DIRECTION('',(0.,0.,-1.));
#27905=DIRECTION('',(0.,0.,-1.));
#27906=DIRECTION('',(0.,0.,-1.));
#27907=DIRECTION('',(0.,0.,-1.));
#27908=DIRECTION('',(0.,0.,-1.));
#27909=DIRECTION('',(0.,0.,-1.));
#27910=DIRECTION('',(0.,0.,-1.));
#27911=DIRECTION('',(0.,0.,-1.));
#27912=DIRECTION('center_axis',(-0.175032773131272,-0.984562607623292,0.));
#27913=DIRECTION('ref_axis',(-0.984562607623292,0.175032773131272,0.));
#27914=DIRECTION('',(-0.984562607623292,0.175032773131272,0.));
#27915=DIRECTION('',(0.,0.,-1.));
#27916=DIRECTION('',(-0.984562607623292,0.175032773131272,0.));
#27917=DIRECTION('',(0.,0.,-1.));
#27918=DIRECTION('',(0.,0.,-1.));
#27919=DIRECTION('',(0.,0.,-1.));
#27920=DIRECTION('',(0.,0.,-1.));
#27921=DIRECTION('',(0.,0.,-1.));
#27922=DIRECTION('',(0.,0.,-1.));
#27923=DIRECTION('',(0.,0.,-1.));
#27924=DIRECTION('center_axis',(-0.992083762154323,0.125577899607073,0.));
#27925=DIRECTION('ref_axis',(0.125577899607073,0.992083762154323,0.));
#27926=DIRECTION('',(0.125577899607073,0.992083762154323,0.));
#27927=DIRECTION('',(0.,0.,-1.));
#27928=DIRECTION('',(0.125577899607073,0.992083762154323,0.));
#27929=DIRECTION('',(0.,0.,-1.));
#27930=DIRECTION('',(0.,0.,-1.));
#27931=DIRECTION('',(0.,0.,-1.));
#27932=DIRECTION('',(0.,0.,-1.));
#27933=DIRECTION('',(0.,0.,-1.));
#27934=DIRECTION('',(0.,0.,-1.));
#27935=DIRECTION('',(0.,0.,-1.));
#27936=DIRECTION('center_axis',(-0.132163748744578,0.99122789686216,0.));
#27937=DIRECTION('ref_axis',(0.99122789686216,0.132163748744578,0.));
#27938=DIRECTION('',(0.99122789686216,0.132163748744578,0.));
#27939=DIRECTION('',(0.,0.,-1.));
#27940=DIRECTION('',(0.99122789686216,0.132163748744578,0.));
#27941=DIRECTION('',(0.,0.,-1.));
#27942=DIRECTION('center_axis',(0.,0.,1.));
#27943=DIRECTION('ref_axis',(1.,0.,0.));
#27944=DIRECTION('',(0.,0.,-1.));
#27945=DIRECTION('',(0.,0.,-1.));
#27946=DIRECTION('',(0.,0.,-1.));
#27947=DIRECTION('',(0.,0.,-1.));
#27948=DIRECTION('',(0.,0.,-1.));
#27949=DIRECTION('',(0.,0.,-1.));
#27950=DIRECTION('',(0.,0.,-1.));
#27951=DIRECTION('',(0.,0.,-1.));
#27952=DIRECTION('',(0.,0.,-1.));
#27953=DIRECTION('center_axis',(-0.102165340737178,-0.994767431690471,0.));
#27954=DIRECTION('ref_axis',(-0.994767431690471,0.102165340737178,0.));
#27955=DIRECTION('',(-0.994767431690471,0.102165340737178,0.));
#27956=DIRECTION('',(0.,0.,-1.));
#27957=DIRECTION('',(-0.994767431690471,0.102165340737178,0.));
#27958=DIRECTION('',(0.,0.,-1.));
#27959=DIRECTION('',(0.,0.,-1.));
#27960=DIRECTION('',(0.,0.,-1.));
#27961=DIRECTION('',(0.,0.,-1.));
#27962=DIRECTION('',(0.,0.,-1.));
#27963=DIRECTION('',(0.,0.,-1.));
#27964=DIRECTION('',(0.,0.,-1.));
#27965=DIRECTION('',(0.,0.,-1.));
#27966=DIRECTION('',(0.,0.,-1.));
#27967=DIRECTION('center_axis',(0.,-1.,0.));
#27968=DIRECTION('ref_axis',(-1.,0.,0.));
#27969=DIRECTION('',(-1.,0.,0.));
#27970=DIRECTION('',(0.,0.,-1.));
#27971=DIRECTION('',(-1.,0.,0.));
#27972=DIRECTION('center_axis',(1.,0.,0.));
#27973=DIRECTION('ref_axis',(0.,-1.,0.));
#27974=DIRECTION('',(0.,-1.,0.));
#27975=DIRECTION('',(0.,0.,-1.));
#27976=DIRECTION('',(0.,-1.,0.));
#27977=DIRECTION('center_axis',(-1.0289465542069E-16,1.,0.));
#27978=DIRECTION('ref_axis',(1.,1.0289465542069E-16,0.));
#27979=DIRECTION('',(1.,1.0289465542069E-16,0.));
#27980=DIRECTION('',(0.,0.,-1.));
#27981=DIRECTION('',(1.,1.0289465542069E-16,0.));
#27982=DIRECTION('center_axis',(0.,0.,1.));
#27983=DIRECTION('ref_axis',(1.,0.,0.));
#27984=DIRECTION('center_axis',(0.,-1.,0.));
#27985=DIRECTION('ref_axis',(-1.,0.,0.));
#27986=DIRECTION('',(-1.,0.,0.));
#27987=DIRECTION('',(0.,0.,-1.));
#27988=DIRECTION('',(-1.,0.,0.));
#27989=DIRECTION('',(0.,0.,-1.));
#27990=DIRECTION('',(0.,0.,-1.));
#27991=DIRECTION('',(0.,0.,-1.));
#27992=DIRECTION('',(0.,0.,-1.));
#27993=DIRECTION('',(0.,0.,-1.));
#27994=DIRECTION('',(0.,0.,-1.));
#27995=DIRECTION('center_axis',(0.,1.,0.));
#27996=DIRECTION('ref_axis',(1.,0.,0.));
#27997=DIRECTION('',(1.,0.,0.));
#27998=DIRECTION('',(0.,0.,-1.));
#27999=DIRECTION('',(1.,0.,0.));
#28000=DIRECTION('center_axis',(1.,0.,0.));
#28001=DIRECTION('ref_axis',(0.,-1.,0.));
#28002=DIRECTION('',(0.,-1.,0.));
#28003=DIRECTION('',(0.,-1.,0.));
#28004=DIRECTION('center_axis',(0.,-1.,0.));
#28005=DIRECTION('ref_axis',(-1.,0.,0.));
#28006=DIRECTION('',(-1.,0.,0.));
#28007=DIRECTION('',(0.,0.,-1.));
#28008=DIRECTION('',(-1.,0.,0.));
#28009=DIRECTION('',(0.,0.,-1.));
#28010=DIRECTION('',(0.,0.,-1.));
#28011=DIRECTION('',(0.,0.,-1.));
#28012=DIRECTION('',(0.,0.,-1.));
#28013=DIRECTION('',(0.,0.,-1.));
#28014=DIRECTION('',(0.,0.,-1.));
#28015=DIRECTION('',(0.,0.,-1.));
#28016=DIRECTION('center_axis',(0.,1.,0.));
#28017=DIRECTION('ref_axis',(1.,0.,0.));
#28018=DIRECTION('',(1.,0.,0.));
#28019=DIRECTION('',(0.,0.,-1.));
#28020=DIRECTION('',(1.,0.,0.));
#28021=DIRECTION('center_axis',(-1.,0.,0.));
#28022=DIRECTION('ref_axis',(0.,1.,0.));
#28023=DIRECTION('',(0.,1.,0.));
#28024=DIRECTION('',(0.,0.,-1.));
#28025=DIRECTION('',(0.,1.,0.));
#28026=DIRECTION('center_axis',(0.,-1.,0.));
#28027=DIRECTION('ref_axis',(-1.,0.,0.));
#28028=DIRECTION('',(-1.,0.,0.));
#28029=DIRECTION('',(0.,0.,-1.));
#28030=DIRECTION('',(-1.,0.,0.));
#28031=DIRECTION('center_axis',(1.,0.,0.));
#28032=DIRECTION('ref_axis',(0.,-1.,0.));
#28033=DIRECTION('',(0.,-1.,0.));
#28034=DIRECTION('',(0.,-1.,0.));
#28035=DIRECTION('center_axis',(0.,0.,1.));
#28036=DIRECTION('ref_axis',(1.,0.,0.));
#28037=DIRECTION('',(0.,0.,-1.));
#28038=DIRECTION('',(0.,0.,-1.));
#28039=DIRECTION('',(0.,0.,-1.));
#28040=DIRECTION('',(0.,0.,-1.));
#28041=DIRECTION('',(0.,0.,-1.));
#28042=DIRECTION('',(0.,0.,-1.));
#28043=DIRECTION('',(0.,0.,-1.));
#28044=DIRECTION('',(0.,0.,-1.));
#28045=DIRECTION('',(0.,0.,-1.));
#28046=DIRECTION('',(0.,0.,-1.));
#28047=DIRECTION('',(0.,0.,-1.));
#28048=DIRECTION('',(0.,0.,-1.));
#28049=DIRECTION('',(0.,0.,-1.));
#28050=DIRECTION('',(0.,0.,-1.));
#28051=DIRECTION('',(0.,0.,-1.));
#28052=DIRECTION('',(0.,0.,-1.));
#28053=DIRECTION('',(0.,0.,-1.));
#28054=DIRECTION('',(0.,0.,-1.));
#28055=DIRECTION('',(0.,0.,-1.));
#28056=DIRECTION('',(0.,0.,-1.));
#28057=DIRECTION('',(0.,0.,-1.));
#28058=DIRECTION('',(0.,0.,-1.));
#28059=DIRECTION('',(0.,0.,-1.));
#28060=DIRECTION('',(0.,0.,-1.));
#28061=DIRECTION('',(0.,0.,-1.));
#28062=DIRECTION('',(0.,0.,-1.));
#28063=DIRECTION('center_axis',(0.0779744070100615,-0.996955361012432,0.));
#28064=DIRECTION('ref_axis',(-0.996955361012432,-0.0779744070100615,0.));
#28065=DIRECTION('',(-0.996955361012432,-0.0779744070100615,0.));
#28066=DIRECTION('',(0.,0.,-1.));
#28067=DIRECTION('',(-0.996955361012432,-0.0779744070100615,0.));
#28068=DIRECTION('',(0.,0.,-1.));
#28069=DIRECTION('center_axis',(0.,0.,1.));
#28070=DIRECTION('ref_axis',(1.,0.,0.));
#28071=DIRECTION('',(0.,0.,-1.));
#28072=DIRECTION('',(0.,0.,-1.));
#28073=DIRECTION('',(0.,0.,-1.));
#28074=DIRECTION('',(0.,0.,-1.));
#28075=DIRECTION('',(0.,0.,-1.));
#28076=DIRECTION('',(0.,0.,-1.));
#28077=DIRECTION('',(0.,0.,-1.));
#28078=DIRECTION('',(0.,0.,-1.));
#28079=DIRECTION('',(0.,0.,-1.));
#28080=DIRECTION('',(0.,0.,-1.));
#28081=DIRECTION('',(0.,0.,-1.));
#28082=DIRECTION('',(0.,0.,-1.));
#28083=DIRECTION('',(0.,0.,-1.));
#28084=DIRECTION('',(0.,0.,-1.));
#28085=DIRECTION('',(0.,0.,-1.));
#28086=DIRECTION('',(0.,0.,-1.));
#28087=DIRECTION('center_axis',(1.,0.,0.));
#28088=DIRECTION('ref_axis',(0.,-1.,0.));
#28089=DIRECTION('',(0.,-1.,0.));
#28090=DIRECTION('',(0.,0.,-1.));
#28091=DIRECTION('',(0.,-1.,0.));
#28092=DIRECTION('center_axis',(0.,1.,0.));
#28093=DIRECTION('ref_axis',(1.,0.,0.));
#28094=DIRECTION('',(1.,0.,0.));
#28095=DIRECTION('',(0.,0.,-1.));
#28096=DIRECTION('',(1.,0.,0.));
#28097=DIRECTION('center_axis',(-1.,0.,0.));
#28098=DIRECTION('ref_axis',(0.,1.,0.));
#28099=DIRECTION('',(0.,1.,0.));
#28100=DIRECTION('',(0.,0.,-1.));
#28101=DIRECTION('',(0.,1.,0.));
#28102=DIRECTION('center_axis',(0.,-1.,0.));
#28103=DIRECTION('ref_axis',(-1.,0.,0.));
#28104=DIRECTION('',(-1.,0.,0.));
#28105=DIRECTION('',(0.,0.,-1.));
#28106=DIRECTION('',(-1.,0.,0.));
#28107=DIRECTION('center_axis',(1.,0.,0.));
#28108=DIRECTION('ref_axis',(0.,-1.,0.));
#28109=DIRECTION('',(0.,-1.,0.));
#28110=DIRECTION('',(0.,0.,-1.));
#28111=DIRECTION('',(0.,-1.,0.));
#28112=DIRECTION('center_axis',(0.,0.,1.));
#28113=DIRECTION('ref_axis',(1.,0.,0.));
#28114=DIRECTION('',(0.,0.,-1.));
#28115=DIRECTION('',(0.,0.,-1.));
#28116=DIRECTION('',(0.,0.,-1.));
#28117=DIRECTION('',(0.,0.,-1.));
#28118=DIRECTION('',(0.,0.,-1.));
#28119=DIRECTION('center_axis',(0.937477410285731,-0.348046125109819,0.));
#28120=DIRECTION('ref_axis',(-0.348046125109819,-0.937477410285731,0.));
#28121=DIRECTION('',(-0.348046125109819,-0.937477410285731,0.));
#28122=DIRECTION('',(0.,0.,-1.));
#28123=DIRECTION('',(-0.348046125109819,-0.937477410285731,0.));
#28124=DIRECTION('',(0.,0.,-1.));
#28125=DIRECTION('',(0.,0.,-1.));
#28126=DIRECTION('',(0.,0.,-1.));
#28127=DIRECTION('center_axis',(1.,0.,0.));
#28128=DIRECTION('ref_axis',(0.,-1.,0.));
#28129=DIRECTION('',(0.,-1.,0.));
#28130=DIRECTION('',(0.,0.,-1.));
#28131=DIRECTION('',(0.,-1.,0.));
#28132=DIRECTION('center_axis',(0.,1.,0.));
#28133=DIRECTION('ref_axis',(1.,0.,0.));
#28134=DIRECTION('',(1.,0.,0.));
#28135=DIRECTION('',(0.,0.,-1.));
#28136=DIRECTION('',(1.,0.,0.));
#28137=DIRECTION('center_axis',(-1.,0.,0.));
#28138=DIRECTION('ref_axis',(0.,1.,0.));
#28139=DIRECTION('',(0.,1.,0.));
#28140=DIRECTION('',(0.,0.,-1.));
#28141=DIRECTION('',(0.,1.,0.));
#28142=DIRECTION('center_axis',(0.,-1.,0.));
#28143=DIRECTION('ref_axis',(-1.,0.,0.));
#28144=DIRECTION('',(-1.,0.,0.));
#28145=DIRECTION('',(0.,0.,-1.));
#28146=DIRECTION('',(-1.,0.,0.));
#28147=DIRECTION('center_axis',(1.,0.,0.));
#28148=DIRECTION('ref_axis',(0.,-1.,0.));
#28149=DIRECTION('',(0.,-1.,0.));
#28150=DIRECTION('',(0.,-1.,0.));
#28151=DIRECTION('center_axis',(0.,0.,1.));
#28152=DIRECTION('ref_axis',(1.,0.,0.));
#28153=DIRECTION('center_axis',(0.,0.,1.));
#28154=DIRECTION('ref_axis',(1.,0.,0.));
#28155=DIRECTION('center_axis',(0.,0.,1.));
#28156=DIRECTION('ref_axis',(1.,0.,0.));
#28157=DIRECTION('center_axis',(0.,0.,1.));
#28158=DIRECTION('ref_axis',(1.,0.,0.));
#28159=DIRECTION('center_axis',(0.,0.,1.));
#28160=DIRECTION('ref_axis',(1.,0.,0.));
#28161=DIRECTION('center_axis',(0.,0.,1.));
#28162=DIRECTION('ref_axis',(1.,0.,0.));
#28163=DIRECTION('center_axis',(0.,0.,1.));
#28164=DIRECTION('ref_axis',(1.,0.,0.));
#28165=DIRECTION('center_axis',(0.,0.,1.));
#28166=DIRECTION('ref_axis',(1.,0.,0.));
#28167=DIRECTION('center_axis',(0.,0.,1.));
#28168=DIRECTION('ref_axis',(1.,0.,0.));
#28169=DIRECTION('',(0.,0.,1.));
#28170=DIRECTION('center_axis',(0.,1.,0.));
#28171=DIRECTION('ref_axis',(0.,0.,1.));
#28172=DIRECTION('center_axis',(0.,1.,0.));
#28173=DIRECTION('ref_axis',(0.,0.,1.));
#28174=DIRECTION('',(8.65956056235493E-17,-0.707106781186548,0.707106781186548));
#28175=DIRECTION('center_axis',(0.,-1.,0.));
#28176=DIRECTION('ref_axis',(0.,0.,1.));
#28177=DIRECTION('center_axis',(0.,1.,0.));
#28178=DIRECTION('ref_axis',(0.,0.,1.));
#28179=DIRECTION('center_axis',(0.,1.,0.));
#28180=DIRECTION('ref_axis',(1.,0.,0.));
#28181=DIRECTION('',(0.,1.,0.));
#28182=DIRECTION('center_axis',(0.,1.,0.));
#28183=DIRECTION('ref_axis',(1.,0.,0.));
#28184=DIRECTION('',(0.,0.,-1.));
#28185=DIRECTION('',(0.,0.,1.));
#28186=DIRECTION('',(1.,0.,0.));
#28187=DIRECTION('center_axis',(0.,1.,0.));
#28188=DIRECTION('ref_axis',(0.,0.,1.));
#28189=DIRECTION('',(-1.04972719113862E-16,0.515038074910054,-0.857167300702112));
#28190=DIRECTION('center_axis',(0.,1.,0.));
#28191=DIRECTION('ref_axis',(1.,0.,0.));
#28192=DIRECTION('center_axis',(0.,1.,0.));
#28193=DIRECTION('ref_axis',(0.,0.,1.));
#28194=DIRECTION('',(0.,1.,0.));
#28195=DIRECTION('',(0.,1.,0.));
#28196=DIRECTION('center_axis',(0.,1.,0.));
#28197=DIRECTION('ref_axis',(1.,0.,0.));
#28198=DIRECTION('center_axis',(0.,-1.,0.));
#28199=DIRECTION('ref_axis',(0.,0.,-1.));
#28200=DIRECTION('center_axis',(0.,0.,-1.));
#28201=DIRECTION('ref_axis',(-1.,0.,0.));
#28202=DIRECTION('center_axis',(0.,0.,-1.));
#28203=DIRECTION('ref_axis',(1.,0.,0.));
#28204=DIRECTION('center_axis',(0.,0.,1.));
#28205=DIRECTION('ref_axis',(1.,0.,0.));
#28206=DIRECTION('center_axis',(0.,0.,1.));
#28207=DIRECTION('ref_axis',(-1.,1.22464679914735E-16,0.));
#28208=DIRECTION('',(0.,0.,-1.));
#28209=DIRECTION('center_axis',(0.,0.,1.));
#28210=DIRECTION('ref_axis',(1.,0.,0.));
#28211=DIRECTION('center_axis',(0.,0.,1.));
#28212=DIRECTION('ref_axis',(-1.,1.22464679914735E-16,0.));
#28213=DIRECTION('center_axis',(0.,0.,1.));
#28214=DIRECTION('ref_axis',(1.,0.,0.));
#28215=DIRECTION('center_axis',(0.,0.,-1.));
#28216=DIRECTION('ref_axis',(-1.,1.22464679914735E-16,0.));
#28217=DIRECTION('center_axis',(1.22464679914735E-16,-1.,0.));
#28218=DIRECTION('ref_axis',(-1.,-1.22464679914735E-16,0.));
#28219=DIRECTION('center_axis',(0.,0.,-1.));
#28220=DIRECTION('ref_axis',(1.,0.,0.));
#28221=DIRECTION('center_axis',(0.,0.,-1.));
#28222=DIRECTION('ref_axis',(1.,0.,0.));
#28223=DIRECTION('',(0.707106781186548,-8.65956056235493E-17,0.707106781186548));
#28224=DIRECTION('center_axis',(0.,0.,1.));
#28225=DIRECTION('ref_axis',(1.,0.,0.));
#28226=DIRECTION('center_axis',(0.,0.,-1.));
#28227=DIRECTION('ref_axis',(-1.,0.,0.));
#28228=DIRECTION('center_axis',(0.,0.,1.));
#28229=DIRECTION('ref_axis',(1.,0.,0.));
#28230=DIRECTION('center_axis',(0.,0.,-1.));
#28231=DIRECTION('ref_axis',(1.,0.,0.));
#28232=DIRECTION('center_axis',(0.,0.,-1.));
#28233=DIRECTION('ref_axis',(1.,0.,0.));
#28234=DIRECTION('center_axis',(0.,0.,-1.));
#28235=DIRECTION('ref_axis',(-1.,0.,0.));
#28236=DIRECTION('center_axis',(0.,0.,-1.));
#28237=DIRECTION('ref_axis',(1.,0.,0.));
#28238=DIRECTION('center_axis',(0.,0.,-1.));
#28239=DIRECTION('ref_axis',(1.,0.,0.));
#28240=DIRECTION('center_axis',(0.,0.,-1.));
#28241=DIRECTION('ref_axis',(1.,0.,0.));
#28242=DIRECTION('center_axis',(0.,0.,1.));
#28243=DIRECTION('ref_axis',(1.,0.,0.));
#28244=DIRECTION('',(0.,0.,1.));
#28245=DIRECTION('center_axis',(0.,0.,1.));
#28246=DIRECTION('ref_axis',(1.,0.,0.));
#28247=DIRECTION('center_axis',(0.,0.,-1.));
#28248=DIRECTION('ref_axis',(1.,0.,0.));
#28249=DIRECTION('',(0.707106781186548,-8.65956056235493E-17,0.707106781186548));
#28250=DIRECTION('center_axis',(0.,0.,1.));
#28251=DIRECTION('ref_axis',(1.,0.,0.));
#28252=DIRECTION('center_axis',(0.,0.,1.));
#28253=DIRECTION('ref_axis',(1.,0.,0.));
#28254=DIRECTION('',(0.,0.,1.));
#28255=DIRECTION('center_axis',(0.,0.,1.));
#28256=DIRECTION('ref_axis',(1.,0.,0.));
#28257=DIRECTION('center_axis',(0.,0.,-1.));
#28258=DIRECTION('ref_axis',(1.,0.,0.));
#28259=DIRECTION('',(0.707106781186547,-8.65956056235493E-17,0.707106781186547));
#28260=DIRECTION('center_axis',(0.,0.,1.));
#28261=DIRECTION('ref_axis',(1.,0.,0.));
#28262=DIRECTION('center_axis',(0.,0.,1.));
#28263=DIRECTION('ref_axis',(1.,0.,0.));
#28264=DIRECTION('',(0.,0.,1.));
#28265=DIRECTION('center_axis',(0.,0.,1.));
#28266=DIRECTION('ref_axis',(1.,0.,0.));
#28267=DIRECTION('center_axis',(0.,0.,-1.));
#28268=DIRECTION('ref_axis',(1.,0.,0.));
#28269=DIRECTION('',(0.707106781186548,-8.65956056235493E-17,0.707106781186548));
#28270=DIRECTION('center_axis',(0.,0.,1.));
#28271=DIRECTION('ref_axis',(1.,0.,0.));
#28272=DIRECTION('center_axis',(0.,0.,1.));
#28273=DIRECTION('ref_axis',(1.,0.,0.));
#28274=DIRECTION('',(0.,0.,1.));
#28275=DIRECTION('center_axis',(0.,0.,1.));
#28276=DIRECTION('ref_axis',(1.,0.,0.));
#28277=DIRECTION('center_axis',(0.,0.,-1.));
#28278=DIRECTION('ref_axis',(1.,0.,0.));
#28279=DIRECTION('',(0.707106781186548,-8.65956056235493E-17,0.707106781186548));
#28280=DIRECTION('center_axis',(0.,0.,1.));
#28281=DIRECTION('ref_axis',(1.,0.,0.));
#28282=DIRECTION('center_axis',(0.,0.,1.));
#28283=DIRECTION('ref_axis',(1.,0.,0.));
#28284=DIRECTION('',(0.,0.,1.));
#28285=DIRECTION('center_axis',(0.,0.,1.));
#28286=DIRECTION('ref_axis',(1.,0.,0.));
#28287=DIRECTION('center_axis',(0.,0.,-1.));
#28288=DIRECTION('ref_axis',(1.,0.,0.));
#28289=DIRECTION('',(0.707106781186548,-8.65956056235493E-17,0.707106781186548));
#28290=DIRECTION('center_axis',(0.,0.,1.));
#28291=DIRECTION('ref_axis',(1.,0.,0.));
#28292=DIRECTION('center_axis',(0.,0.,1.));
#28293=DIRECTION('ref_axis',(1.,0.,0.));
#28294=DIRECTION('',(0.,0.,1.));
#28295=DIRECTION('center_axis',(0.,0.,1.));
#28296=DIRECTION('ref_axis',(1.,0.,0.));
#28297=DIRECTION('center_axis',(0.,0.,-1.));
#28298=DIRECTION('ref_axis',(1.,0.,0.));
#28299=DIRECTION('',(0.857167300702112,1.04972719113862E-16,0.515038074910054));
#28300=DIRECTION('center_axis',(0.,0.,-1.));
#28301=DIRECTION('ref_axis',(1.,0.,0.));
#28302=DIRECTION('',(0.857167300702112,1.04972719113862E-16,0.515038074910054));
#28303=DIRECTION('center_axis',(0.,0.,-1.));
#28304=DIRECTION('ref_axis',(1.,0.,0.));
#28305=DIRECTION('',(0.857167300702112,1.04972719113862E-16,0.515038074910054));
#28306=DIRECTION('center_axis',(0.,0.,-1.));
#28307=DIRECTION('ref_axis',(1.,0.,0.));
#28308=DIRECTION('',(0.857167300702113,1.04972719113862E-16,0.515038074910053));
#28309=DIRECTION('center_axis',(0.,0.,-1.));
#28310=DIRECTION('ref_axis',(1.,0.,0.));
#28311=DIRECTION('',(0.857167300702112,1.04972719113862E-16,0.515038074910054));
#28312=DIRECTION('center_axis',(0.,0.,-1.));
#28313=DIRECTION('ref_axis',(1.,0.,0.));
#28314=DIRECTION('',(0.857167300702112,1.04972719113862E-16,0.515038074910054));
#28315=DIRECTION('center_axis',(0.,0.,-1.));
#28316=DIRECTION('ref_axis',(-1.,0.,0.));
#28317=DIRECTION('',(-0.707106781186548,8.65956056235493E-17,0.707106781186548));
#28318=DIRECTION('center_axis',(0.,0.,1.));
#28319=DIRECTION('ref_axis',(-1.,0.,0.));
#28320=DIRECTION('center_axis',(0.,0.,1.));
#28321=DIRECTION('ref_axis',(-1.,0.,0.));
#28322=DIRECTION('center_axis',(0.,0.,1.));
#28323=DIRECTION('ref_axis',(1.,0.,0.));
#28324=DIRECTION('center_axis',(0.,0.,1.));
#28325=DIRECTION('ref_axis',(1.,0.,0.));
#28326=DIRECTION('',(0.,0.,-1.));
#28327=DIRECTION('center_axis',(0.,0.,1.));
#28328=DIRECTION('ref_axis',(1.,0.,0.));
#28329=DIRECTION('center_axis',(0.,0.,1.));
#28330=DIRECTION('ref_axis',(1.,0.,0.));
#28331=DIRECTION('',(0.707106781186544,8.65956056235489E-17,-0.707106781186551));
#28332=DIRECTION('center_axis',(0.,0.,-1.));
#28333=DIRECTION('ref_axis',(-1.,0.,0.));
#28334=DIRECTION('center_axis',(0.,0.,1.));
#28335=DIRECTION('ref_axis',(1.,0.,0.));
#28336=DIRECTION('center_axis',(0.,0.,1.));
#28337=DIRECTION('ref_axis',(1.,0.,0.));
#28338=DIRECTION('',(0.,0.,-1.));
#28339=DIRECTION('center_axis',(0.,0.,1.));
#28340=DIRECTION('ref_axis',(1.,0.,0.));
#28341=DIRECTION('center_axis',(0.,0.,-1.));
#28342=DIRECTION('ref_axis',(-1.,0.,0.));
#28343=DIRECTION('axis',(0.,0.,1.));
#28344=DIRECTION('refdir',(1.,0.,0.));
#28345=DIRECTION('center_axis',(0.,0.,1.));
#28346=DIRECTION('ref_axis',(1.,0.,0.));
#28347=DIRECTION('center_axis',(0.,0.,1.));
#28348=DIRECTION('ref_axis',(1.,0.,0.));
#28349=DIRECTION('center_axis',(0.,0.,1.));
#28350=DIRECTION('ref_axis',(1.,0.,0.));
#28351=DIRECTION('center_axis',(0.,0.,1.));
#28352=DIRECTION('ref_axis',(1.,0.,0.));
#28353=DIRECTION('center_axis',(0.,0.,1.));
#28354=DIRECTION('ref_axis',(1.,0.,0.));
#28355=DIRECTION('',(0.,0.,1.));
#28356=DIRECTION('center_axis',(0.,0.,-1.));
#28357=DIRECTION('ref_axis',(-1.,0.,0.));
#28358=DIRECTION('center_axis',(0.,0.,-1.));
#28359=DIRECTION('ref_axis',(1.,0.,0.));
#28360=DIRECTION('center_axis',(0.,0.,1.));
#28361=DIRECTION('ref_axis',(1.,0.,0.));
#28362=DIRECTION('',(0.,0.,-1.));
#28363=DIRECTION('center_axis',(0.,0.,1.));
#28364=DIRECTION('ref_axis',(1.,0.,0.));
#28365=DIRECTION('center_axis',(0.,0.,1.));
#28366=DIRECTION('ref_axis',(1.,0.,0.));
#28367=DIRECTION('center_axis',(0.,0.,1.));
#28368=DIRECTION('ref_axis',(1.,0.,0.));
#28369=DIRECTION('center_axis',(0.,0.,1.));
#28370=DIRECTION('ref_axis',(1.,0.,0.));
#28371=DIRECTION('center_axis',(0.,0.,1.));
#28372=DIRECTION('ref_axis',(1.,0.,0.));
#28373=DIRECTION('',(0.,0.,1.));
#28374=DIRECTION('center_axis',(0.,0.,-1.));
#28375=DIRECTION('ref_axis',(-1.,0.,0.));
#28376=DIRECTION('center_axis',(0.,0.,-1.));
#28377=DIRECTION('ref_axis',(1.,0.,0.));
#28378=DIRECTION('center_axis',(0.,0.,1.));
#28379=DIRECTION('ref_axis',(1.,0.,0.));
#28380=DIRECTION('',(0.,0.,-1.));
#28381=DIRECTION('center_axis',(0.,0.,1.));
#28382=DIRECTION('ref_axis',(1.,0.,0.));
#28383=DIRECTION('center_axis',(0.,0.,1.));
#28384=DIRECTION('ref_axis',(1.,0.,0.));
#28385=DIRECTION('center_axis',(0.,0.,1.));
#28386=DIRECTION('ref_axis',(1.,0.,0.));
#28387=DIRECTION('',(0.,0.,-1.));
#28388=DIRECTION('center_axis',(0.,0.,1.));
#28389=DIRECTION('ref_axis',(1.,0.,0.));
#28390=DIRECTION('center_axis',(0.,0.,1.));
#28391=DIRECTION('ref_axis',(1.,0.,0.));
#28392=DIRECTION('center_axis',(0.,0.,1.));
#28393=DIRECTION('ref_axis',(1.,0.,0.));
#28394=DIRECTION('',(0.978980419737605,1.19890523745959E-16,-0.203954254112001));
#28395=DIRECTION('center_axis',(0.,0.,1.));
#28396=DIRECTION('ref_axis',(1.,0.,0.));
#28397=DIRECTION('',(0.707106781186548,8.65956056235493E-17,-0.707106781186547));
#28398=DIRECTION('center_axis',(0.,0.,1.));
#28399=DIRECTION('ref_axis',(1.,0.,0.));
#28400=DIRECTION('center_axis',(0.,0.,1.));
#28401=DIRECTION('ref_axis',(1.,0.,0.));
#28402=DIRECTION('',(0.,0.,-1.));
#28403=DIRECTION('center_axis',(0.,0.,-1.));
#28404=DIRECTION('ref_axis',(1.,0.,0.));
#28405=DIRECTION('center_axis',(0.,0.,1.));
#28406=DIRECTION('ref_axis',(1.,0.,0.));
#28407=DIRECTION('',(-0.707106781186549,-8.65956056235496E-17,-0.707106781186546));
#28408=DIRECTION('center_axis',(0.,0.,1.));
#28409=DIRECTION('ref_axis',(1.,0.,0.));
#28410=DIRECTION('center_axis',(0.,0.,1.));
#28411=DIRECTION('ref_axis',(1.,0.,0.));
#28412=DIRECTION('center_axis',(0.,0.,1.));
#28413=DIRECTION('ref_axis',(1.,0.,0.));
#28414=DIRECTION('',(0.,0.,-1.));
#28415=DIRECTION('center_axis',(0.,0.,1.));
#28416=DIRECTION('ref_axis',(1.,0.,0.));
#28417=DIRECTION('center_axis',(0.,0.,1.));
#28418=DIRECTION('ref_axis',(1.,0.,0.));
#28419=DIRECTION('',(0.961523947640823,1.17752722478186E-16,-0.274721127897378));
#28420=DIRECTION('center_axis',(0.,0.,1.));
#28421=DIRECTION('ref_axis',(1.,0.,0.));
#28422=DIRECTION('center_axis',(0.,0.,1.));
#28423=DIRECTION('ref_axis',(1.,0.,0.));
#28424=DIRECTION('',(0.,0.,-1.));
#28425=DIRECTION('center_axis',(0.,0.,1.));
#28426=DIRECTION('ref_axis',(1.,0.,0.));
#28427=DIRECTION('center_axis',(6.12323399573677E-17,0.,1.));
#28428=DIRECTION('ref_axis',(1.,0.,0.));
#28429=DIRECTION('center_axis',(1.22464679914735E-16,-1.,0.));
#28430=DIRECTION('ref_axis',(-1.,-1.22464679914735E-16,0.));
#28431=DIRECTION('axis',(0.,0.,1.));
#28432=DIRECTION('refdir',(1.,0.,0.));
#28433=DIRECTION('center_axis',(0.,0.,1.));
#28434=DIRECTION('ref_axis',(1.,0.,0.));
#28435=DIRECTION('center_axis',(0.,0.,-1.));
#28436=DIRECTION('ref_axis',(1.,0.,0.));
#28437=DIRECTION('',(0.,0.,1.));
#28438=DIRECTION('center_axis',(0.,0.,-1.));
#28439=DIRECTION('ref_axis',(1.,0.,0.));
#28440=DIRECTION('center_axis',(0.,0.,1.));
#28441=DIRECTION('ref_axis',(1.,0.,0.));
#28442=DIRECTION('center_axis',(0.,0.,1.));
#28443=DIRECTION('ref_axis',(1.,0.,0.));
#28444=DIRECTION('',(0.,0.,1.));
#28445=DIRECTION('center_axis',(0.,0.,1.));
#28446=DIRECTION('ref_axis',(1.,0.,0.));
#28447=DIRECTION('center_axis',(0.,0.,1.));
#28448=DIRECTION('ref_axis',(1.,0.,0.));
#28449=DIRECTION('center_axis',(0.,0.,-1.));
#28450=DIRECTION('ref_axis',(-1.,0.,0.));
#28451=DIRECTION('center_axis',(0.,0.,1.));
#28452=DIRECTION('ref_axis',(1.,0.,0.));
#28453=DIRECTION('center_axis',(6.12323399573677E-17,0.,1.));
#28454=DIRECTION('ref_axis',(1.,0.,0.));
#28455=DIRECTION('center_axis',(0.,0.,1.));
#28456=DIRECTION('ref_axis',(1.,0.,0.));
#28457=DIRECTION('center_axis',(1.22464679914735E-16,-1.,0.));
#28458=DIRECTION('ref_axis',(-1.,-1.22464679914735E-16,0.));
#28459=DIRECTION('center_axis',(0.,0.,1.));
#28460=DIRECTION('ref_axis',(1.,0.,0.));
#28461=DIRECTION('center_axis',(0.,0.,1.));
#28462=DIRECTION('ref_axis',(1.,0.,0.));
#28463=DIRECTION('',(0.,0.,-1.));
#28464=DIRECTION('center_axis',(0.,0.,1.));
#28465=DIRECTION('ref_axis',(1.,0.,0.));
#28466=DIRECTION('center_axis',(0.,0.,-1.));
#28467=DIRECTION('ref_axis',(-1.,0.,0.));
#28468=DIRECTION('center_axis',(0.,0.,1.));
#28469=DIRECTION('ref_axis',(1.,0.,0.));
#28470=DIRECTION('center_axis',(0.,0.,1.));
#28471=DIRECTION('ref_axis',(1.,0.,0.));
#28472=DIRECTION('',(0.,0.,-1.));
#28473=DIRECTION('center_axis',(0.,0.,1.));
#28474=DIRECTION('ref_axis',(1.,0.,0.));
#28475=DIRECTION('center_axis',(0.,0.,-1.));
#28476=DIRECTION('ref_axis',(-1.,0.,0.));
#28477=DIRECTION('center_axis',(0.,0.,1.));
#28478=DIRECTION('ref_axis',(1.,0.,0.));
#28479=DIRECTION('center_axis',(0.,0.,1.));
#28480=DIRECTION('ref_axis',(1.,0.,0.));
#28481=DIRECTION('',(0.707106781186548,8.65956056235493E-17,-0.707106781186548));
#28482=DIRECTION('center_axis',(0.,0.,1.));
#28483=DIRECTION('ref_axis',(1.,0.,0.));
#28484=DIRECTION('center_axis',(0.,0.,1.));
#28485=DIRECTION('ref_axis',(1.,0.,0.));
#28486=DIRECTION('',(0.,0.,-1.));
#28487=DIRECTION('center_axis',(0.,0.,-1.));
#28488=DIRECTION('ref_axis',(1.,0.,0.));
#28489=DIRECTION('center_axis',(0.,0.,1.));
#28490=DIRECTION('ref_axis',(1.,0.,0.));
#28491=DIRECTION('',(-0.707106781186548,-8.65956056235494E-17,-0.707106781186547));
#28492=DIRECTION('center_axis',(0.,0.,1.));
#28493=DIRECTION('ref_axis',(1.,0.,0.));
#28494=DIRECTION('center_axis',(0.,0.,1.));
#28495=DIRECTION('ref_axis',(1.,0.,0.));
#28496=DIRECTION('center_axis',(0.,0.,1.));
#28497=DIRECTION('ref_axis',(1.,0.,0.));
#28498=DIRECTION('center_axis',(0.,0.,1.));
#28499=DIRECTION('ref_axis',(1.,0.,0.));
#28500=DIRECTION('',(0.,0.,-1.));
#28501=DIRECTION('center_axis',(0.,0.,-1.));
#28502=DIRECTION('ref_axis',(1.,0.,0.));
#28503=DIRECTION('center_axis',(0.,0.,1.));
#28504=DIRECTION('ref_axis',(1.,0.,0.));
#28505=DIRECTION('',(-0.707106781186548,-8.65956056235494E-17,-0.707106781186547));
#28506=DIRECTION('center_axis',(0.,0.,1.));
#28507=DIRECTION('ref_axis',(1.,0.,0.));
#28508=DIRECTION('axis',(0.,0.,1.));
#28509=DIRECTION('refdir',(1.,0.,0.));
#28510=DIRECTION('center_axis',(0.,0.,-1.));
#28511=DIRECTION('ref_axis',(1.,0.,0.));
#28512=DIRECTION('center_axis',(0.,0.,1.));
#28513=DIRECTION('ref_axis',(1.,0.,0.));
#28514=DIRECTION('',(-0.207911690817759,-2.54618386665283E-17,-0.978147600733806));
#28515=DIRECTION('center_axis',(0.,0.,1.));
#28516=DIRECTION('ref_axis',(1.,0.,0.));
#28517=DIRECTION('center_axis',(0.193871877856065,-0.0751063656107956,-0.978147600733806));
#28518=DIRECTION('ref_axis',(0.912095473942782,-0.353347669066023,0.207911690817759));
#28519=DIRECTION('center_axis',(-0.193871877856065,0.0751063656107956,0.978147600733806));
#28520=DIRECTION('ref_axis',(0.912095473942777,-0.353347669066036,0.207911690817759));
#28521=DIRECTION('center_axis',(0.153648593508749,-0.140069200367114,-0.978147600733806));
#28522=DIRECTION('ref_axis',(0.72285979930028,-0.658973777457692,0.207911690817759));
#28523=DIRECTION('center_axis',(-0.153648593508749,0.140069200367114,0.978147600733806));
#28524=DIRECTION('ref_axis',(-0.722859799300274,0.658973777457698,-0.207911690817759));
#28525=DIRECTION('center_axis',(0.0926742152118281,-0.186114913463622,-0.978147600733806));
#28526=DIRECTION('ref_axis',(-0.435997903257843,0.875601825703936,-0.207911690817759));
#28527=DIRECTION('center_axis',(-0.0926742152118281,0.186114913463622,0.978147600733806));
#28528=DIRECTION('ref_axis',(-0.435997903257843,0.875601825703936,-0.207911690817759));
#28529=DIRECTION('center_axis',(0.0191836706249958,-0.207024776198529,-0.978147600733806));
#28530=DIRECTION('ref_axis',(0.0902520744326832,-0.973974995511639,0.207911690817759));
#28531=DIRECTION('center_axis',(-0.0191836706249958,0.207024776198529,0.978147600733806));
#28532=DIRECTION('ref_axis',(-0.09025207443267,0.973974995511641,-0.207911690817759));
#28533=DIRECTION('center_axis',(-0.0568977349801305,-0.19997479574394,-0.978147600733806));
#28534=DIRECTION('ref_axis',(-0.267682797148639,-0.940807445193745,0.207911690817759));
#28535=DIRECTION('center_axis',(0.0568977349801305,0.19997479574394,0.978147600733806));
#28536=DIRECTION('ref_axis',(0.267682797148655,0.94080744519374,-0.207911690817759));
#28537=DIRECTION('center_axis',(-0.125294786194957,-0.165917111025535,-0.978147600733806));
#28538=DIRECTION('ref_axis',(0.589465623693464,0.780578636208407,-0.207911690817759));
#28539=DIRECTION('center_axis',(0.125294786194957,0.165917111025535,0.978147600733806));
#28540=DIRECTION('ref_axis',(0.589465623693459,0.78057863620841,-0.207911690817759));
#28541=DIRECTION('center_axis',(-0.176770082251776,-0.109451401084681,-0.978147600733806));
#28542=DIRECTION('ref_axis',(0.831637851416697,0.514928357067584,-0.207911690817759));
#28543=DIRECTION('center_axis',(0.176770082251776,0.109451401084681,0.978147600733806));
#28544=DIRECTION('ref_axis',(-0.831637851416687,-0.514928357067599,0.207911690817759));
#28545=DIRECTION('center_axis',(-0.204371599183654,-0.0382036729361911,
-0.978147600733806));
#28546=DIRECTION('ref_axis',(-0.961492779041678,-0.179734149988288,0.207911690817759));
#28547=DIRECTION('center_axis',(0.204371599183654,0.0382036729361911,0.978147600733806));
#28548=DIRECTION('ref_axis',(-0.961492779041679,-0.179734149988278,0.207911690817759));
#28549=DIRECTION('center_axis',(-0.204371599183654,0.0382036729361911,-0.978147600733806));
#28550=DIRECTION('ref_axis',(-0.961492779041682,0.179734149988266,0.207911690817759));
#28551=DIRECTION('center_axis',(0.204371599183654,-0.0382036729361911,0.978147600733806));
#28552=DIRECTION('ref_axis',(-0.961492779041682,0.179734149988263,0.207911690817759));
#28553=DIRECTION('center_axis',(-0.176770082251776,0.109451401084681,-0.978147600733806));
#28554=DIRECTION('ref_axis',(0.831637851416689,-0.514928357067596,-0.207911690817759));
#28555=DIRECTION('center_axis',(0.176770082251776,-0.109451401084681,0.978147600733806));
#28556=DIRECTION('ref_axis',(0.831637851416683,-0.514928357067606,-0.207911690817759));
#28557=DIRECTION('center_axis',(-0.125294786194957,0.165917111025535,-0.978147600733806));
#28558=DIRECTION('ref_axis',(0.589465623693458,-0.780578636208411,-0.207911690817759));
#28559=DIRECTION('center_axis',(0.125294786194957,-0.165917111025535,0.978147600733806));
#28560=DIRECTION('ref_axis',(-0.589465623693466,0.780578636208405,0.207911690817759));
#28561=DIRECTION('center_axis',(-0.0568977349801304,0.19997479574394,-0.978147600733806));
#28562=DIRECTION('ref_axis',(0.267682797148634,-0.940807445193746,-0.207911690817759));
#28563=DIRECTION('center_axis',(0.0568977349801304,-0.19997479574394,0.978147600733806));
#28564=DIRECTION('ref_axis',(-0.267682797148657,0.94080744519374,0.207911690817759));
#28565=DIRECTION('center_axis',(0.0191836706249959,0.207024776198529,-0.978147600733806));
#28566=DIRECTION('ref_axis',(-0.0902520744327104,-0.973974995511637,-0.207911690817759));
#28567=DIRECTION('center_axis',(-0.0191836706249959,-0.207024776198529,
0.978147600733806));
#28568=DIRECTION('ref_axis',(-0.0902520744326996,-0.973974995511638,-0.207911690817759));
#28569=DIRECTION('center_axis',(0.092674215211828,0.186114913463622,-0.978147600733806));
#28570=DIRECTION('ref_axis',(-0.435997903257874,-0.87560182570392,-0.207911690817759));
#28571=DIRECTION('center_axis',(-0.092674215211828,-0.186114913463622,0.978147600733806));
#28572=DIRECTION('ref_axis',(-0.435997903257872,-0.875601825703921,-0.207911690817759));
#28573=DIRECTION('center_axis',(0.153648593508749,0.140069200367114,-0.978147600733806));
#28574=DIRECTION('ref_axis',(-0.722859799300277,-0.658973777457695,-0.207911690817759));
#28575=DIRECTION('center_axis',(-0.153648593508749,-0.140069200367114,0.978147600733806));
#28576=DIRECTION('ref_axis',(0.722859799300275,0.658973777457698,0.207911690817759));
#28577=DIRECTION('center_axis',(0.193871877856065,0.0751063656107956,-0.978147600733806));
#28578=DIRECTION('ref_axis',(-0.91209547394278,-0.353347669066029,-0.207911690817759));
#28579=DIRECTION('center_axis',(-0.193871877856065,-0.0751063656107956,
0.978147600733806));
#28580=DIRECTION('ref_axis',(-0.912095473942774,-0.353347669066044,-0.207911690817759));
#28581=DIRECTION('center_axis',(-0.207911690817759,0.,0.978147600733806));
#28582=DIRECTION('ref_axis',(-0.978147600733806,1.44941316600844E-14,-0.207911690817759));
#28583=DIRECTION('center_axis',(0.207911690817759,0.,-0.978147600733806));
#28584=DIRECTION('ref_axis',(-0.978147600733806,2.89270309802114E-14,-0.207911690817759));
#28585=DIRECTION('center_axis',(0.,0.,-1.));
#28586=DIRECTION('ref_axis',(1.,0.,0.));
#28587=DIRECTION('center_axis',(0.,0.,1.));
#28588=DIRECTION('ref_axis',(1.,0.,0.));
#28589=DIRECTION('',(-0.207911690817759,-2.54618386665283E-17,-0.978147600733806));
#28590=DIRECTION('center_axis',(0.,0.,1.));
#28591=DIRECTION('ref_axis',(1.,0.,0.));
#28592=DIRECTION('center_axis',(-0.193871877856065,0.0751063656107956,0.978147600733806));
#28593=DIRECTION('ref_axis',(-0.912095473942771,0.353347669066052,-0.207911690817759));
#28594=DIRECTION('center_axis',(0.193871877856065,-0.0751063656107956,-0.978147600733806));
#28595=DIRECTION('ref_axis',(0.912095473942774,-0.353347669066046,0.207911690817759));
#28596=DIRECTION('center_axis',(-0.153648593508749,0.140069200367114,0.978147600733806));
#28597=DIRECTION('ref_axis',(-0.722859799300271,0.658973777457701,-0.207911690817759));
#28598=DIRECTION('center_axis',(0.153648593508749,-0.140069200367114,-0.978147600733806));
#28599=DIRECTION('ref_axis',(-0.722859799300268,0.658973777457704,-0.207911690817759));
#28600=DIRECTION('center_axis',(-0.0926742152118281,0.186114913463622,0.978147600733806));
#28601=DIRECTION('ref_axis',(-0.435997903257849,0.875601825703933,-0.207911690817759));
#28602=DIRECTION('center_axis',(0.0926742152118281,-0.186114913463622,-0.978147600733806));
#28603=DIRECTION('ref_axis',(0.435997903257857,-0.875601825703929,0.207911690817759));
#28604=DIRECTION('center_axis',(-0.0191836706249958,0.207024776198529,0.978147600733806));
#28605=DIRECTION('ref_axis',(-0.0902520744326517,0.973974995511642,-0.20791169081776));
#28606=DIRECTION('center_axis',(0.0191836706249958,-0.207024776198529,-0.978147600733806));
#28607=DIRECTION('ref_axis',(-0.0902520744326596,0.973974995511642,-0.207911690817759));
#28608=DIRECTION('center_axis',(0.0568977349801305,0.19997479574394,0.978147600733806));
#28609=DIRECTION('ref_axis',(-0.267682797148646,-0.940807445193743,0.207911690817759));
#28610=DIRECTION('center_axis',(-0.0568977349801305,-0.19997479574394,-0.978147600733806));
#28611=DIRECTION('ref_axis',(0.267682797148649,0.940807445193742,-0.207911690817759));
#28612=DIRECTION('center_axis',(0.125294786194957,0.165917111025535,0.978147600733806));
#28613=DIRECTION('ref_axis',(-0.589465623693455,-0.780578636208413,0.207911690817759));
#28614=DIRECTION('center_axis',(-0.125294786194957,-0.165917111025535,-0.978147600733806));
#28615=DIRECTION('ref_axis',(-0.589465623693456,-0.780578636208413,0.207911690817759));
#28616=DIRECTION('center_axis',(0.176770082251776,0.109451401084681,0.978147600733806));
#28617=DIRECTION('ref_axis',(-0.831637851416686,-0.514928357067601,0.207911690817759));
#28618=DIRECTION('center_axis',(-0.176770082251776,-0.109451401084681,-0.978147600733806));
#28619=DIRECTION('ref_axis',(-0.831637851416685,-0.514928357067603,0.207911690817759));
#28620=DIRECTION('center_axis',(0.204371599183654,0.0382036729361911,0.978147600733806));
#28621=DIRECTION('ref_axis',(-0.961492779041674,-0.179734149988305,0.207911690817759));
#28622=DIRECTION('center_axis',(-0.204371599183654,-0.0382036729361911,
-0.978147600733806));
#28623=DIRECTION('ref_axis',(-0.96149277904168,-0.179734149988275,0.207911690817759));
#28624=DIRECTION('center_axis',(0.204371599183654,-0.0382036729361911,0.978147600733806));
#28625=DIRECTION('ref_axis',(0.96149277904168,-0.179734149988275,-0.20791169081776));
#28626=DIRECTION('center_axis',(-0.204371599183654,0.0382036729361911,-0.978147600733806));
#28627=DIRECTION('ref_axis',(-0.961492779041682,0.179734149988263,0.207911690817759));
#28628=DIRECTION('center_axis',(0.176770082251776,-0.109451401084681,0.978147600733806));
#28629=DIRECTION('ref_axis',(-0.831637851416696,0.514928357067584,0.207911690817759));
#28630=DIRECTION('center_axis',(-0.176770082251776,0.109451401084681,-0.978147600733806));
#28631=DIRECTION('ref_axis',(-0.831637851416691,0.514928357067592,0.207911690817759));
#28632=DIRECTION('center_axis',(0.125294786194957,-0.165917111025535,0.978147600733806));
#28633=DIRECTION('ref_axis',(0.589465623693455,-0.780578636208414,-0.207911690817759));
#28634=DIRECTION('center_axis',(-0.125294786194957,0.165917111025535,-0.978147600733806));
#28635=DIRECTION('ref_axis',(0.589465623693456,-0.780578636208413,-0.207911690817759));
#28636=DIRECTION('center_axis',(0.0568977349801304,-0.19997479574394,0.978147600733806));
#28637=DIRECTION('ref_axis',(0.267682797148621,-0.94080744519375,-0.207911690817759));
#28638=DIRECTION('center_axis',(-0.0568977349801304,0.19997479574394,-0.978147600733806));
#28639=DIRECTION('ref_axis',(0.267682797148624,-0.940807445193749,-0.207911690817759));
#28640=DIRECTION('center_axis',(-0.0191836706249959,-0.207024776198529,
0.978147600733806));
#28641=DIRECTION('ref_axis',(-0.0902520744327203,-0.973974995511636,-0.207911690817759));
#28642=DIRECTION('center_axis',(0.0191836706249959,0.207024776198529,-0.978147600733806));
#28643=DIRECTION('ref_axis',(-0.0902520744327027,-0.973974995511638,-0.207911690817759));
#28644=DIRECTION('center_axis',(-0.092674215211828,-0.186114913463622,0.978147600733806));
#28645=DIRECTION('ref_axis',(-0.435997903257856,-0.875601825703929,-0.207911690817759));
#28646=DIRECTION('center_axis',(0.092674215211828,0.186114913463622,-0.978147600733806));
#28647=DIRECTION('ref_axis',(0.435997903257841,0.875601825703937,0.207911690817759));
#28648=DIRECTION('center_axis',(-0.153648593508749,-0.140069200367114,0.978147600733806));
#28649=DIRECTION('ref_axis',(-0.722859799300277,-0.658973777457695,-0.207911690817759));
#28650=DIRECTION('center_axis',(0.153648593508749,0.140069200367114,-0.978147600733806));
#28651=DIRECTION('ref_axis',(0.722859799300275,0.658973777457697,0.207911690817759));
#28652=DIRECTION('center_axis',(-0.193871877856065,-0.0751063656107956,
0.978147600733806));
#28653=DIRECTION('ref_axis',(-0.912095473942778,-0.353347669066035,-0.207911690817759));
#28654=DIRECTION('center_axis',(0.193871877856065,0.0751063656107956,-0.978147600733806));
#28655=DIRECTION('ref_axis',(-0.91209547394278,-0.353347669066029,-0.20791169081776));
#28656=DIRECTION('center_axis',(-0.207911690817759,0.,0.978147600733806));
#28657=DIRECTION('ref_axis',(-0.978147600733806,4.72416904338303E-15,-0.207911690817759));
#28658=DIRECTION('center_axis',(0.207911690817759,0.,-0.978147600733806));
#28659=DIRECTION('ref_axis',(-0.978147600733806,1.44941316600844E-14,-0.207911690817759));
#28660=DIRECTION('center_axis',(0.,0.,1.));
#28661=DIRECTION('ref_axis',(1.,0.,0.));
#28662=DIRECTION('',(0.978147600733806,1.19788532833232E-16,-0.207911690817759));
#28663=DIRECTION('center_axis',(0.,0.,1.));
#28664=DIRECTION('ref_axis',(1.,0.,0.));
#28665=DIRECTION('',(0.978147600733805,1.19788532833232E-16,-0.207911690817761));
#28666=DIRECTION('center_axis',(-0.193871877856065,0.0751063656107956,0.978147600733806));
#28667=DIRECTION('ref_axis',(0.912095473942774,-0.353347669066046,0.207911690817759));
#28668=DIRECTION('center_axis',(-0.193871877856065,0.0751063656107956,0.978147600733806));
#28669=DIRECTION('ref_axis',(0.912095473942773,-0.353347669066046,0.207911690817759));
#28670=DIRECTION('center_axis',(-0.193871877856065,0.0751063656107956,0.978147600733806));
#28671=DIRECTION('ref_axis',(0.912095473942774,-0.353347669066046,0.207911690817759));
#28672=DIRECTION('center_axis',(-0.193871877856065,0.0751063656107956,0.978147600733806));
#28673=DIRECTION('ref_axis',(0.912095473942773,-0.353347669066046,0.207911690817759));
#28674=DIRECTION('center_axis',(-0.193871877856065,0.0751063656107956,0.978147600733806));
#28675=DIRECTION('ref_axis',(-0.91209547394277,0.353347669066056,-0.207911690817759));
#28676=DIRECTION('center_axis',(-0.193871877856065,0.0751063656107956,0.978147600733806));
#28677=DIRECTION('ref_axis',(0.912095473942773,-0.353347669066046,0.207911690817759));
#28678=DIRECTION('center_axis',(0.193871877856065,-0.0751063656107956,-0.978147600733806));
#28679=DIRECTION('ref_axis',(0.912095473942773,-0.353347669066046,0.207911690817759));
#28680=DIRECTION('center_axis',(-0.193871877856065,0.0751063656107956,0.978147600733806));
#28681=DIRECTION('ref_axis',(0.912095473942773,-0.353347669066046,0.207911690817759));
#28682=DIRECTION('center_axis',(0.193871877856065,-0.0751063656107956,-0.978147600733806));
#28683=DIRECTION('ref_axis',(0.912095473942773,-0.353347669066046,0.207911690817759));
#28684=DIRECTION('center_axis',(-0.193871877856065,0.0751063656107956,0.978147600733806));
#28685=DIRECTION('ref_axis',(0.912095473942773,-0.353347669066046,0.207911690817759));
#28686=DIRECTION('center_axis',(0.,0.,-1.));
#28687=DIRECTION('ref_axis',(-0.932472229404348,0.361241666187173,1.58735880974294E-16));
#28688=DIRECTION('center_axis',(0.193871877856065,-0.0751063656107956,-0.978147600733806));
#28689=DIRECTION('ref_axis',(-0.912095473942774,0.353347669066046,-0.207911690817759));
#28690=DIRECTION('center_axis',(-0.153648593508749,0.140069200367114,0.978147600733806));
#28691=DIRECTION('ref_axis',(0.722859799300275,-0.658973777457697,0.207911690817759));
#28692=DIRECTION('center_axis',(-0.153648593508749,0.140069200367114,0.978147600733806));
#28693=DIRECTION('ref_axis',(0.722859799300275,-0.658973777457697,0.207911690817759));
#28694=DIRECTION('center_axis',(-0.153648593508749,0.140069200367114,0.978147600733806));
#28695=DIRECTION('ref_axis',(0.722859799300275,-0.658973777457697,0.207911690817759));
#28696=DIRECTION('center_axis',(-0.153648593508749,0.140069200367114,0.978147600733806));
#28697=DIRECTION('ref_axis',(0.722859799300275,-0.658973777457697,0.207911690817759));
#28698=DIRECTION('center_axis',(-0.153648593508749,0.140069200367114,0.978147600733806));
#28699=DIRECTION('ref_axis',(0.722859799300277,-0.658973777457695,0.207911690817759));
#28700=DIRECTION('center_axis',(-0.153648593508749,0.140069200367114,0.978147600733806));
#28701=DIRECTION('ref_axis',(0.722859799300275,-0.658973777457697,0.207911690817759));
#28702=DIRECTION('center_axis',(0.153648593508749,-0.140069200367114,-0.978147600733806));
#28703=DIRECTION('ref_axis',(0.722859799300276,-0.658973777457697,0.207911690817759));
#28704=DIRECTION('center_axis',(-0.153648593508749,0.140069200367114,0.978147600733806));
#28705=DIRECTION('ref_axis',(0.722859799300275,-0.658973777457697,0.207911690817759));
#28706=DIRECTION('center_axis',(0.153648593508749,-0.140069200367114,-0.978147600733806));
#28707=DIRECTION('ref_axis',(0.722859799300276,-0.658973777457697,0.207911690817759));
#28708=DIRECTION('center_axis',(-0.153648593508749,0.140069200367114,0.978147600733806));
#28709=DIRECTION('ref_axis',(0.722859799300275,-0.658973777457697,0.207911690817759));
#28710=DIRECTION('center_axis',(0.,0.,-1.));
#28711=DIRECTION('ref_axis',(-0.739008917220659,0.673695643646558,1.58735880974294E-16));
#28712=DIRECTION('center_axis',(0.153648593508749,-0.140069200367114,-0.978147600733806));
#28713=DIRECTION('ref_axis',(-0.722859799300275,0.658973777457697,-0.207911690817759));
#28714=DIRECTION('center_axis',(-0.0926742152118281,0.186114913463622,0.978147600733806));
#28715=DIRECTION('ref_axis',(0.435997903257853,-0.875601825703931,0.207911690817759));
#28716=DIRECTION('center_axis',(-0.0926742152118281,0.186114913463622,0.978147600733806));
#28717=DIRECTION('ref_axis',(0.435997903257853,-0.875601825703931,0.207911690817759));
#28718=DIRECTION('center_axis',(-0.0926742152118281,0.186114913463622,0.978147600733806));
#28719=DIRECTION('ref_axis',(0.435997903257853,-0.875601825703931,0.207911690817759));
#28720=DIRECTION('center_axis',(-0.0926742152118281,0.186114913463622,0.978147600733806));
#28721=DIRECTION('ref_axis',(0.435997903257853,-0.875601825703931,0.207911690817759));
#28722=DIRECTION('center_axis',(-0.0926742152118281,0.186114913463622,0.978147600733806));
#28723=DIRECTION('ref_axis',(0.435997903257859,-0.875601825703928,0.207911690817759));
#28724=DIRECTION('center_axis',(-0.0926742152118281,0.186114913463622,0.978147600733806));
#28725=DIRECTION('ref_axis',(0.435997903257853,-0.875601825703931,0.207911690817759));
#28726=DIRECTION('center_axis',(0.0926742152118281,-0.186114913463622,-0.978147600733806));
#28727=DIRECTION('ref_axis',(0.435997903257853,-0.875601825703931,0.207911690817759));
#28728=DIRECTION('center_axis',(-0.0926742152118281,0.186114913463622,0.978147600733806));
#28729=DIRECTION('ref_axis',(0.435997903257853,-0.875601825703931,0.207911690817759));
#28730=DIRECTION('center_axis',(0.0926742152118281,-0.186114913463622,-0.978147600733806));
#28731=DIRECTION('ref_axis',(0.435997903257853,-0.875601825703931,0.207911690817759));
#28732=DIRECTION('center_axis',(-0.0926742152118281,0.186114913463622,0.978147600733806));
#28733=DIRECTION('ref_axis',(0.435997903257853,-0.875601825703931,0.207911690817759));
#28734=DIRECTION('center_axis',(0.,0.,-1.));
#28735=DIRECTION('ref_axis',(-0.445738355776558,0.895163291355053,1.58735880974294E-16));
#28736=DIRECTION('center_axis',(0.0926742152118281,-0.186114913463622,-0.978147600733806));
#28737=DIRECTION('ref_axis',(-0.435997903257853,0.875601825703931,-0.207911690817759));
#28738=DIRECTION('center_axis',(-0.0191836706249958,0.207024776198529,0.978147600733806));
#28739=DIRECTION('ref_axis',(0.0902520744326727,-0.97397499551164,0.207911690817759));
#28740=DIRECTION('center_axis',(-0.0191836706249958,0.207024776198529,0.978147600733806));
#28741=DIRECTION('ref_axis',(0.0902520744326727,-0.97397499551164,0.207911690817759));
#28742=DIRECTION('center_axis',(-0.0191836706249958,0.207024776198529,0.978147600733806));
#28743=DIRECTION('ref_axis',(0.0902520744326727,-0.97397499551164,0.207911690817759));
#28744=DIRECTION('center_axis',(-0.0191836706249958,0.207024776198529,0.978147600733806));
#28745=DIRECTION('ref_axis',(0.0902520744326727,-0.97397499551164,0.207911690817759));
#28746=DIRECTION('center_axis',(-0.0191836706249958,0.207024776198529,0.978147600733806));
#28747=DIRECTION('ref_axis',(-0.0902520744326673,0.973974995511641,-0.207911690817759));
#28748=DIRECTION('center_axis',(-0.0191836706249958,0.207024776198529,0.978147600733806));
#28749=DIRECTION('ref_axis',(0.0902520744326727,-0.97397499551164,0.207911690817759));
#28750=DIRECTION('center_axis',(0.0191836706249958,-0.207024776198529,-0.978147600733806));
#28751=DIRECTION('ref_axis',(0.0902520744326727,-0.97397499551164,0.207911690817759));
#28752=DIRECTION('center_axis',(-0.0191836706249958,0.207024776198529,0.978147600733806));
#28753=DIRECTION('ref_axis',(0.0902520744326727,-0.97397499551164,0.207911690817759));
#28754=DIRECTION('center_axis',(0.0191836706249958,-0.207024776198529,-0.978147600733806));
#28755=DIRECTION('ref_axis',(0.0902520744326727,-0.97397499551164,0.207911690817759));
#28756=DIRECTION('center_axis',(-0.0191836706249958,0.207024776198529,0.978147600733806));
#28757=DIRECTION('ref_axis',(0.0902520744326727,-0.97397499551164,0.207911690817759));
#28758=DIRECTION('center_axis',(0.,0.,-1.));
#28759=DIRECTION('ref_axis',(-0.0922683594632729,0.995734176295037,1.58735880974294E-16));
#28760=DIRECTION('center_axis',(0.0191836706249958,-0.207024776198529,-0.978147600733806));
#28761=DIRECTION('ref_axis',(-0.0902520744326727,0.97397499551164,-0.207911690817759));
#28762=DIRECTION('center_axis',(0.0568977349801305,0.19997479574394,0.978147600733806));
#28763=DIRECTION('ref_axis',(-0.267682797148647,-0.940807445193742,0.207911690817759));
#28764=DIRECTION('center_axis',(0.0568977349801305,0.19997479574394,0.978147600733806));
#28765=DIRECTION('ref_axis',(-0.267682797148647,-0.940807445193742,0.207911690817759));
#28766=DIRECTION('center_axis',(0.0568977349801305,0.19997479574394,0.978147600733806));
#28767=DIRECTION('ref_axis',(-0.267682797148647,-0.940807445193742,0.207911690817759));
#28768=DIRECTION('center_axis',(0.0568977349801305,0.19997479574394,0.978147600733806));
#28769=DIRECTION('ref_axis',(-0.267682797148647,-0.940807445193742,0.207911690817759));
#28770=DIRECTION('center_axis',(0.0568977349801305,0.19997479574394,0.978147600733806));
#28771=DIRECTION('ref_axis',(0.267682797148653,0.940807445193741,-0.207911690817759));
#28772=DIRECTION('center_axis',(0.0568977349801305,0.19997479574394,0.978147600733806));
#28773=DIRECTION('ref_axis',(-0.267682797148647,-0.940807445193742,0.207911690817759));
#28774=DIRECTION('center_axis',(-0.0568977349801305,-0.19997479574394,-0.978147600733806));
#28775=DIRECTION('ref_axis',(-0.267682797148647,-0.940807445193742,0.207911690817759));
#28776=DIRECTION('center_axis',(0.0568977349801305,0.19997479574394,0.978147600733806));
#28777=DIRECTION('ref_axis',(-0.267682797148647,-0.940807445193742,0.207911690817759));
#28778=DIRECTION('center_axis',(-0.0568977349801305,-0.19997479574394,-0.978147600733806));
#28779=DIRECTION('ref_axis',(-0.267682797148647,-0.940807445193742,0.207911690817759));
#28780=DIRECTION('center_axis',(0.0568977349801305,0.19997479574394,0.978147600733806));
#28781=DIRECTION('ref_axis',(-0.267682797148647,-0.940807445193742,0.207911690817759));
#28782=DIRECTION('center_axis',(0.,0.,-1.));
#28783=DIRECTION('ref_axis',(0.273662990072067,0.961825643172824,1.58735880974294E-16));
#28784=DIRECTION('center_axis',(-0.0568977349801305,-0.19997479574394,-0.978147600733806));
#28785=DIRECTION('ref_axis',(0.267682797148647,0.940807445193742,-0.207911690817759));
#28786=DIRECTION('center_axis',(0.125294786194957,0.165917111025535,0.978147600733806));
#28787=DIRECTION('ref_axis',(-0.589465623693459,-0.78057863620841,0.207911690817759));
#28788=DIRECTION('center_axis',(0.125294786194957,0.165917111025535,0.978147600733806));
#28789=DIRECTION('ref_axis',(-0.589465623693459,-0.78057863620841,0.207911690817759));
#28790=DIRECTION('center_axis',(0.125294786194957,0.165917111025535,0.978147600733806));
#28791=DIRECTION('ref_axis',(-0.589465623693459,-0.78057863620841,0.207911690817759));
#28792=DIRECTION('center_axis',(0.125294786194957,0.165917111025535,0.978147600733806));
#28793=DIRECTION('ref_axis',(-0.589465623693459,-0.78057863620841,0.207911690817759));
#28794=DIRECTION('center_axis',(0.125294786194957,0.165917111025535,0.978147600733806));
#28795=DIRECTION('ref_axis',(0.589465623693459,0.78057863620841,-0.207911690817759));
#28796=DIRECTION('center_axis',(0.125294786194957,0.165917111025535,0.978147600733806));
#28797=DIRECTION('ref_axis',(-0.589465623693459,-0.78057863620841,0.207911690817759));
#28798=DIRECTION('center_axis',(-0.125294786194957,-0.165917111025535,-0.978147600733806));
#28799=DIRECTION('ref_axis',(-0.589465623693459,-0.78057863620841,0.207911690817759));
#28800=DIRECTION('center_axis',(0.125294786194957,0.165917111025535,0.978147600733806));
#28801=DIRECTION('ref_axis',(-0.589465623693459,-0.78057863620841,0.207911690817759));
#28802=DIRECTION('center_axis',(-0.125294786194957,-0.165917111025535,-0.978147600733806));
#28803=DIRECTION('ref_axis',(-0.589465623693459,-0.78057863620841,0.207911690817759));
#28804=DIRECTION('center_axis',(0.125294786194957,0.165917111025535,0.978147600733806));
#28805=DIRECTION('ref_axis',(-0.589465623693459,-0.78057863620841,0.207911690817759));
#28806=DIRECTION('center_axis',(0.,0.,-1.));
#28807=DIRECTION('ref_axis',(0.602634636379246,0.798017227280247,1.58735880974294E-16));
#28808=DIRECTION('center_axis',(-0.125294786194957,-0.165917111025535,-0.978147600733806));
#28809=DIRECTION('ref_axis',(0.589465623693459,0.78057863620841,-0.207911690817759));
#28810=DIRECTION('center_axis',(0.176770082251776,0.109451401084681,0.978147600733806));
#28811=DIRECTION('ref_axis',(-0.831637851416691,-0.514928357067594,0.207911690817759));
#28812=DIRECTION('center_axis',(0.176770082251776,0.109451401084681,0.978147600733806));
#28813=DIRECTION('ref_axis',(-0.83163785141669,-0.514928357067594,0.207911690817759));
#28814=DIRECTION('center_axis',(0.176770082251776,0.109451401084681,0.978147600733806));
#28815=DIRECTION('ref_axis',(-0.831637851416691,-0.514928357067594,0.207911690817759));
#28816=DIRECTION('center_axis',(0.176770082251776,0.109451401084681,0.978147600733806));
#28817=DIRECTION('ref_axis',(-0.83163785141669,-0.514928357067594,0.207911690817759));
#28818=DIRECTION('center_axis',(0.176770082251776,0.109451401084681,0.978147600733806));
#28819=DIRECTION('ref_axis',(-0.831637851416684,-0.514928357067604,0.207911690817759));
#28820=DIRECTION('center_axis',(0.176770082251776,0.109451401084681,0.978147600733806));
#28821=DIRECTION('ref_axis',(-0.83163785141669,-0.514928357067594,0.207911690817759));
#28822=DIRECTION('center_axis',(-0.176770082251776,-0.109451401084681,-0.978147600733806));
#28823=DIRECTION('ref_axis',(-0.831637851416691,-0.514928357067594,0.207911690817759));
#28824=DIRECTION('center_axis',(0.176770082251776,0.109451401084681,0.978147600733806));
#28825=DIRECTION('ref_axis',(-0.83163785141669,-0.514928357067594,0.207911690817759));
#28826=DIRECTION('center_axis',(-0.176770082251776,-0.109451401084681,-0.978147600733806));
#28827=DIRECTION('ref_axis',(-0.831637851416691,-0.514928357067594,0.207911690817759));
#28828=DIRECTION('center_axis',(0.176770082251776,0.109451401084681,0.978147600733806));
#28829=DIRECTION('ref_axis',(-0.83163785141669,-0.514928357067594,0.207911690817759));
#28830=DIRECTION('center_axis',(0.,0.,-1.));
#28831=DIRECTION('ref_axis',(0.85021713572961,0.526432162877362,1.58735880974294E-16));
#28832=DIRECTION('center_axis',(-0.176770082251776,-0.109451401084681,-0.978147600733806));
#28833=DIRECTION('ref_axis',(0.831637851416691,0.514928357067594,-0.207911690817759));
#28834=DIRECTION('center_axis',(0.204371599183654,0.0382036729361911,0.978147600733806));
#28835=DIRECTION('ref_axis',(-0.961492779041681,-0.179734149988272,0.207911690817759));
#28836=DIRECTION('center_axis',(0.204371599183654,0.0382036729361911,0.978147600733806));
#28837=DIRECTION('ref_axis',(-0.961492779041681,-0.179734149988272,0.207911690817759));
#28838=DIRECTION('center_axis',(0.204371599183654,0.0382036729361911,0.978147600733806));
#28839=DIRECTION('ref_axis',(-0.961492779041681,-0.179734149988272,0.207911690817759));
#28840=DIRECTION('center_axis',(0.204371599183654,0.0382036729361911,0.978147600733806));
#28841=DIRECTION('ref_axis',(-0.961492779041681,-0.179734149988272,0.207911690817759));
#28842=DIRECTION('center_axis',(0.204371599183654,0.0382036729361911,0.978147600733806));
#28843=DIRECTION('ref_axis',(-0.961492779041679,-0.179734149988281,0.207911690817759));
#28844=DIRECTION('center_axis',(0.204371599183654,0.0382036729361911,0.978147600733806));
#28845=DIRECTION('ref_axis',(-0.961492779041681,-0.179734149988272,0.207911690817759));
#28846=DIRECTION('center_axis',(-0.204371599183654,-0.0382036729361911,
-0.978147600733806));
#28847=DIRECTION('ref_axis',(-0.961492779041681,-0.179734149988272,0.207911690817759));
#28848=DIRECTION('center_axis',(0.204371599183654,0.0382036729361911,0.978147600733806));
#28849=DIRECTION('ref_axis',(-0.961492779041681,-0.179734149988272,0.207911690817759));
#28850=DIRECTION('center_axis',(-0.204371599183654,-0.0382036729361911,
-0.978147600733806));
#28851=DIRECTION('ref_axis',(-0.961492779041681,-0.179734149988272,0.207911690817759));
#28852=DIRECTION('center_axis',(0.204371599183654,0.0382036729361911,0.978147600733806));
#28853=DIRECTION('ref_axis',(-0.961492779041681,-0.179734149988272,0.207911690817759));
#28854=DIRECTION('center_axis',(0.,0.,-1.));
#28855=DIRECTION('ref_axis',(0.982973099683894,0.18374951781661,1.58735880974294E-16));
#28856=DIRECTION('center_axis',(-0.204371599183654,-0.0382036729361911,
-0.978147600733806));
#28857=DIRECTION('ref_axis',(0.961492779041681,0.179734149988272,-0.207911690817759));
#28858=DIRECTION('center_axis',(0.204371599183654,-0.0382036729361911,0.978147600733806));
#28859=DIRECTION('ref_axis',(-0.96149277904168,0.179734149988272,0.207911690817759));
#28860=DIRECTION('center_axis',(0.204371599183654,-0.0382036729361911,0.978147600733806));
#28861=DIRECTION('ref_axis',(-0.961492779041681,0.179734149988272,0.207911690817759));
#28862=DIRECTION('center_axis',(0.204371599183654,-0.0382036729361911,0.978147600733806));
#28863=DIRECTION('ref_axis',(-0.96149277904168,0.179734149988272,0.207911690817759));
#28864=DIRECTION('center_axis',(0.204371599183654,-0.0382036729361911,0.978147600733806));
#28865=DIRECTION('ref_axis',(-0.961492779041681,0.179734149988272,0.207911690817759));
#28866=DIRECTION('center_axis',(0.204371599183654,-0.0382036729361911,0.978147600733806));
#28867=DIRECTION('ref_axis',(0.961492779041679,-0.179734149988281,-0.207911690817759));
#28868=DIRECTION('center_axis',(0.204371599183654,-0.0382036729361911,0.978147600733806));
#28869=DIRECTION('ref_axis',(-0.961492779041681,0.179734149988272,0.207911690817759));
#28870=DIRECTION('center_axis',(-0.204371599183654,0.0382036729361911,-0.978147600733806));
#28871=DIRECTION('ref_axis',(-0.961492779041681,0.179734149988272,0.207911690817759));
#28872=DIRECTION('center_axis',(0.204371599183654,-0.0382036729361911,0.978147600733806));
#28873=DIRECTION('ref_axis',(-0.961492779041681,0.179734149988272,0.207911690817759));
#28874=DIRECTION('center_axis',(-0.204371599183654,0.0382036729361911,-0.978147600733806));
#28875=DIRECTION('ref_axis',(-0.961492779041681,0.179734149988272,0.207911690817759));
#28876=DIRECTION('center_axis',(0.204371599183654,-0.0382036729361911,0.978147600733806));
#28877=DIRECTION('ref_axis',(-0.961492779041681,0.179734149988272,0.207911690817759));
#28878=DIRECTION('center_axis',(0.,0.,-1.));
#28879=DIRECTION('ref_axis',(-0.982973099683909,0.183749517816531,1.58735880974294E-16));
#28880=DIRECTION('center_axis',(-0.204371599183654,0.0382036729361911,-0.978147600733806));
#28881=DIRECTION('ref_axis',(0.96149277904168,-0.179734149988272,-0.207911690817759));
#28882=DIRECTION('center_axis',(0.176770082251776,-0.109451401084681,0.978147600733806));
#28883=DIRECTION('ref_axis',(-0.83163785141669,0.514928357067593,0.207911690817759));
#28884=DIRECTION('center_axis',(0.176770082251776,-0.109451401084681,0.978147600733806));
#28885=DIRECTION('ref_axis',(-0.831637851416691,0.514928357067594,0.207911690817759));
#28886=DIRECTION('center_axis',(0.176770082251776,-0.109451401084681,0.978147600733806));
#28887=DIRECTION('ref_axis',(-0.83163785141669,0.514928357067593,0.207911690817759));
#28888=DIRECTION('center_axis',(0.176770082251776,-0.109451401084681,0.978147600733806));
#28889=DIRECTION('ref_axis',(-0.831637851416691,0.514928357067594,0.207911690817759));
#28890=DIRECTION('center_axis',(0.176770082251776,-0.109451401084681,0.978147600733806));
#28891=DIRECTION('ref_axis',(0.831637851416689,-0.514928357067597,-0.207911690817759));
#28892=DIRECTION('center_axis',(0.176770082251776,-0.109451401084681,0.978147600733806));
#28893=DIRECTION('ref_axis',(-0.831637851416691,0.514928357067594,0.207911690817759));
#28894=DIRECTION('center_axis',(-0.176770082251776,0.109451401084681,-0.978147600733806));
#28895=DIRECTION('ref_axis',(-0.831637851416691,0.514928357067593,0.207911690817759));
#28896=DIRECTION('center_axis',(0.176770082251776,-0.109451401084681,0.978147600733806));
#28897=DIRECTION('ref_axis',(-0.831637851416691,0.514928357067594,0.207911690817759));
#28898=DIRECTION('center_axis',(-0.176770082251776,0.109451401084681,-0.978147600733806));
#28899=DIRECTION('ref_axis',(-0.831637851416691,0.514928357067593,0.207911690817759));
#28900=DIRECTION('center_axis',(0.176770082251776,-0.109451401084681,0.978147600733806));
#28901=DIRECTION('ref_axis',(-0.831637851416691,0.514928357067594,0.207911690817759));
#28902=DIRECTION('center_axis',(0.,0.,-1.));
#28903=DIRECTION('ref_axis',(-0.850217135729556,0.52643216287745,1.58735880974294E-16));
#28904=DIRECTION('center_axis',(-0.176770082251776,0.109451401084681,-0.978147600733806));
#28905=DIRECTION('ref_axis',(0.83163785141669,-0.514928357067593,-0.207911690817759));
#28906=DIRECTION('center_axis',(0.125294786194957,-0.165917111025535,0.978147600733806));
#28907=DIRECTION('ref_axis',(-0.589465623693459,0.78057863620841,0.207911690817759));
#28908=DIRECTION('center_axis',(0.125294786194957,-0.165917111025535,0.978147600733806));
#28909=DIRECTION('ref_axis',(-0.589465623693459,0.78057863620841,0.207911690817759));
#28910=DIRECTION('center_axis',(0.125294786194957,-0.165917111025535,0.978147600733806));
#28911=DIRECTION('ref_axis',(-0.589465623693459,0.78057863620841,0.207911690817759));
#28912=DIRECTION('center_axis',(0.125294786194957,-0.165917111025535,0.978147600733806));
#28913=DIRECTION('ref_axis',(-0.589465623693459,0.78057863620841,0.207911690817759));
#28914=DIRECTION('center_axis',(0.125294786194957,-0.165917111025535,0.978147600733806));
#28915=DIRECTION('ref_axis',(0.589465623693453,-0.780578636208415,-0.207911690817759));
#28916=DIRECTION('center_axis',(0.125294786194957,-0.165917111025535,0.978147600733806));
#28917=DIRECTION('ref_axis',(-0.589465623693459,0.78057863620841,0.207911690817759));
#28918=DIRECTION('center_axis',(-0.125294786194957,0.165917111025535,-0.978147600733806));
#28919=DIRECTION('ref_axis',(-0.589465623693459,0.78057863620841,0.207911690817759));
#28920=DIRECTION('center_axis',(0.125294786194957,-0.165917111025535,0.978147600733806));
#28921=DIRECTION('ref_axis',(-0.589465623693459,0.78057863620841,0.207911690817759));
#28922=DIRECTION('center_axis',(-0.125294786194957,0.165917111025535,-0.978147600733806));
#28923=DIRECTION('ref_axis',(-0.589465623693459,0.78057863620841,0.207911690817759));
#28924=DIRECTION('center_axis',(0.125294786194957,-0.165917111025535,0.978147600733806));
#28925=DIRECTION('ref_axis',(-0.589465623693459,0.78057863620841,0.207911690817759));
#28926=DIRECTION('center_axis',(0.,0.,-1.));
#28927=DIRECTION('ref_axis',(-0.602634636379309,0.7980172272802,1.58735880974294E-16));
#28928=DIRECTION('center_axis',(-0.125294786194957,0.165917111025535,-0.978147600733806));
#28929=DIRECTION('ref_axis',(0.589465623693459,-0.78057863620841,-0.207911690817759));
#28930=DIRECTION('center_axis',(0.0568977349801304,-0.19997479574394,0.978147600733806));
#28931=DIRECTION('ref_axis',(-0.267682797148647,0.940807445193742,0.207911690817759));
#28932=DIRECTION('center_axis',(0.0568977349801304,-0.19997479574394,0.978147600733806));
#28933=DIRECTION('ref_axis',(-0.267682797148647,0.940807445193742,0.207911690817759));
#28934=DIRECTION('center_axis',(0.0568977349801304,-0.19997479574394,0.978147600733806));
#28935=DIRECTION('ref_axis',(-0.267682797148647,0.940807445193742,0.207911690817759));
#28936=DIRECTION('center_axis',(0.0568977349801304,-0.19997479574394,0.978147600733806));
#28937=DIRECTION('ref_axis',(-0.267682797148647,0.940807445193742,0.207911690817759));
#28938=DIRECTION('center_axis',(0.0568977349801304,-0.19997479574394,0.978147600733806));
#28939=DIRECTION('ref_axis',(0.267682797148644,-0.940807445193743,-0.207911690817759));
#28940=DIRECTION('center_axis',(0.0568977349801304,-0.19997479574394,0.978147600733806));
#28941=DIRECTION('ref_axis',(-0.267682797148647,0.940807445193742,0.207911690817759));
#28942=DIRECTION('center_axis',(-0.0568977349801304,0.19997479574394,-0.978147600733806));
#28943=DIRECTION('ref_axis',(-0.267682797148647,0.940807445193742,0.207911690817759));
#28944=DIRECTION('center_axis',(0.0568977349801304,-0.19997479574394,0.978147600733806));
#28945=DIRECTION('ref_axis',(-0.267682797148647,0.940807445193742,0.207911690817759));
#28946=DIRECTION('center_axis',(-0.0568977349801304,0.19997479574394,-0.978147600733806));
#28947=DIRECTION('ref_axis',(-0.267682797148647,0.940807445193742,0.207911690817759));
#28948=DIRECTION('center_axis',(0.0568977349801304,-0.19997479574394,0.978147600733806));
#28949=DIRECTION('ref_axis',(-0.267682797148647,0.940807445193742,0.207911690817759));
#28950=DIRECTION('center_axis',(0.,0.,-1.));
#28951=DIRECTION('ref_axis',(-0.273662990072115,0.96182564317281,1.58735880974294E-16));
#28952=DIRECTION('center_axis',(-0.0568977349801304,0.19997479574394,-0.978147600733806));
#28953=DIRECTION('ref_axis',(0.267682797148647,-0.940807445193742,-0.207911690817759));
#28954=DIRECTION('center_axis',(-0.0191836706249959,-0.207024776198529,
0.978147600733806));
#28955=DIRECTION('ref_axis',(0.0902520744326732,0.97397499551164,0.207911690817759));
#28956=DIRECTION('center_axis',(-0.0191836706249959,-0.207024776198529,
0.978147600733806));
#28957=DIRECTION('ref_axis',(0.0902520744326732,0.97397499551164,0.207911690817759));
#28958=DIRECTION('center_axis',(-0.0191836706249959,-0.207024776198529,
0.978147600733806));
#28959=DIRECTION('ref_axis',(0.0902520744326732,0.97397499551164,0.207911690817759));
#28960=DIRECTION('center_axis',(-0.0191836706249959,-0.207024776198529,
0.978147600733806));
#28961=DIRECTION('ref_axis',(0.0902520744326732,0.97397499551164,0.207911690817759));
#28962=DIRECTION('center_axis',(-0.0191836706249959,-0.207024776198529,
0.978147600733806));
#28963=DIRECTION('ref_axis',(-0.0902520744326954,-0.973974995511638,-0.207911690817759));
#28964=DIRECTION('center_axis',(-0.0191836706249959,-0.207024776198529,
0.978147600733806));
#28965=DIRECTION('ref_axis',(0.0902520744326732,0.97397499551164,0.207911690817759));
#28966=DIRECTION('center_axis',(0.0191836706249959,0.207024776198529,-0.978147600733806));
#28967=DIRECTION('ref_axis',(0.0902520744326732,0.97397499551164,0.207911690817759));
#28968=DIRECTION('center_axis',(-0.0191836706249959,-0.207024776198529,
0.978147600733806));
#28969=DIRECTION('ref_axis',(0.0902520744326732,0.97397499551164,0.207911690817759));
#28970=DIRECTION('center_axis',(0.0191836706249959,0.207024776198529,-0.978147600733806));
#28971=DIRECTION('ref_axis',(0.0902520744326732,0.97397499551164,0.207911690817759));
#28972=DIRECTION('center_axis',(-0.0191836706249959,-0.207024776198529,
0.978147600733806));
#28973=DIRECTION('ref_axis',(0.0902520744326732,0.97397499551164,0.207911690817759));
#28974=DIRECTION('center_axis',(0.,0.,-1.));
#28975=DIRECTION('ref_axis',(0.0922683594632895,0.995734176295036,1.58735880974294E-16));
#28976=DIRECTION('center_axis',(0.0191836706249959,0.207024776198529,-0.978147600733806));
#28977=DIRECTION('ref_axis',(-0.0902520744326732,-0.97397499551164,-0.207911690817759));
#28978=DIRECTION('center_axis',(-0.092674215211828,-0.186114913463622,0.978147600733806));
#28979=DIRECTION('ref_axis',(0.435997903257852,0.875601825703931,0.207911690817759));
#28980=DIRECTION('center_axis',(-0.092674215211828,-0.186114913463622,0.978147600733806));
#28981=DIRECTION('ref_axis',(0.435997903257852,0.875601825703931,0.207911690817759));
#28982=DIRECTION('center_axis',(-0.092674215211828,-0.186114913463622,0.978147600733806));
#28983=DIRECTION('ref_axis',(0.435997903257852,0.875601825703931,0.207911690817759));
#28984=DIRECTION('center_axis',(-0.092674215211828,-0.186114913463622,0.978147600733806));
#28985=DIRECTION('ref_axis',(0.435997903257852,0.875601825703931,0.207911690817759));
#28986=DIRECTION('center_axis',(-0.092674215211828,-0.186114913463622,0.978147600733806));
#28987=DIRECTION('ref_axis',(-0.435997903257876,-0.875601825703919,-0.207911690817759));
#28988=DIRECTION('center_axis',(-0.092674215211828,-0.186114913463622,0.978147600733806));
#28989=DIRECTION('ref_axis',(0.435997903257852,0.875601825703931,0.207911690817759));
#28990=DIRECTION('center_axis',(0.092674215211828,0.186114913463622,-0.978147600733806));
#28991=DIRECTION('ref_axis',(0.435997903257852,0.875601825703931,0.207911690817759));
#28992=DIRECTION('center_axis',(-0.092674215211828,-0.186114913463622,0.978147600733806));
#28993=DIRECTION('ref_axis',(0.435997903257852,0.875601825703931,0.207911690817759));
#28994=DIRECTION('center_axis',(0.092674215211828,0.186114913463622,-0.978147600733806));
#28995=DIRECTION('ref_axis',(0.435997903257852,0.875601825703931,0.207911690817759));
#28996=DIRECTION('center_axis',(-0.092674215211828,-0.186114913463622,0.978147600733806));
#28997=DIRECTION('ref_axis',(0.435997903257852,0.875601825703931,0.207911690817759));
#28998=DIRECTION('center_axis',(0.,0.,-1.));
#28999=DIRECTION('ref_axis',(0.445738355776574,0.895163291355045,1.58735880974294E-16));
#29000=DIRECTION('center_axis',(0.092674215211828,0.186114913463622,-0.978147600733806));
#29001=DIRECTION('ref_axis',(-0.435997903257852,-0.875601825703931,-0.207911690817759));
#29002=DIRECTION('center_axis',(-0.153648593508749,-0.140069200367114,0.978147600733806));
#29003=DIRECTION('ref_axis',(0.722859799300275,0.658973777457697,0.207911690817759));
#29004=DIRECTION('center_axis',(-0.153648593508749,-0.140069200367114,0.978147600733806));
#29005=DIRECTION('ref_axis',(0.722859799300275,0.658973777457697,0.207911690817759));
#29006=DIRECTION('center_axis',(-0.153648593508749,-0.140069200367114,0.978147600733806));
#29007=DIRECTION('ref_axis',(0.722859799300275,0.658973777457697,0.207911690817759));
#29008=DIRECTION('center_axis',(-0.153648593508749,-0.140069200367114,0.978147600733806));
#29009=DIRECTION('ref_axis',(0.722859799300275,0.658973777457697,0.207911690817759));
#29010=DIRECTION('center_axis',(-0.153648593508749,-0.140069200367114,0.978147600733806));
#29011=DIRECTION('ref_axis',(0.722859799300273,0.658973777457699,0.207911690817759));
#29012=DIRECTION('center_axis',(-0.153648593508749,-0.140069200367114,0.978147600733806));
#29013=DIRECTION('ref_axis',(0.722859799300275,0.658973777457697,0.207911690817759));
#29014=DIRECTION('center_axis',(0.153648593508749,0.140069200367114,-0.978147600733806));
#29015=DIRECTION('ref_axis',(0.722859799300275,0.658973777457697,0.207911690817759));
#29016=DIRECTION('center_axis',(-0.153648593508749,-0.140069200367114,0.978147600733806));
#29017=DIRECTION('ref_axis',(0.722859799300275,0.658973777457697,0.207911690817759));
#29018=DIRECTION('center_axis',(0.153648593508749,0.140069200367114,-0.978147600733806));
#29019=DIRECTION('ref_axis',(0.722859799300275,0.658973777457697,0.207911690817759));
#29020=DIRECTION('center_axis',(-0.153648593508749,-0.140069200367114,0.978147600733806));
#29021=DIRECTION('ref_axis',(0.722859799300275,0.658973777457697,0.207911690817759));
#29022=DIRECTION('center_axis',(0.,0.,-1.));
#29023=DIRECTION('ref_axis',(0.739008917220659,0.673695643646557,1.58735880974294E-16));
#29024=DIRECTION('center_axis',(0.153648593508749,0.140069200367114,-0.978147600733806));
#29025=DIRECTION('ref_axis',(-0.722859799300275,-0.658973777457697,-0.207911690817759));
#29026=DIRECTION('center_axis',(-0.193871877856065,-0.0751063656107956,
0.978147600733806));
#29027=DIRECTION('ref_axis',(0.912095473942774,0.353347669066046,0.207911690817759));
#29028=DIRECTION('center_axis',(-0.193871877856065,-0.0751063656107956,
0.978147600733806));
#29029=DIRECTION('ref_axis',(0.912095473942774,0.353347669066046,0.207911690817759));
#29030=DIRECTION('center_axis',(-0.193871877856065,-0.0751063656107956,
0.978147600733806));
#29031=DIRECTION('ref_axis',(0.912095473942774,0.353347669066046,0.207911690817759));
#29032=DIRECTION('center_axis',(-0.193871877856065,-0.0751063656107956,
0.978147600733806));
#29033=DIRECTION('ref_axis',(0.912095473942774,0.353347669066046,0.207911690817759));
#29034=DIRECTION('center_axis',(-0.193871877856065,-0.0751063656107956,
0.978147600733806));
#29035=DIRECTION('ref_axis',(-0.912095473942778,-0.353347669066033,-0.207911690817759));
#29036=DIRECTION('center_axis',(-0.193871877856065,-0.0751063656107956,
0.978147600733806));
#29037=DIRECTION('ref_axis',(0.912095473942774,0.353347669066046,0.207911690817759));
#29038=DIRECTION('center_axis',(0.193871877856065,0.0751063656107956,-0.978147600733806));
#29039=DIRECTION('ref_axis',(0.912095473942773,0.353347669066046,0.207911690817759));
#29040=DIRECTION('center_axis',(-0.193871877856065,-0.0751063656107956,
0.978147600733806));
#29041=DIRECTION('ref_axis',(0.912095473942773,0.353347669066046,0.207911690817759));
#29042=DIRECTION('center_axis',(0.193871877856065,0.0751063656107956,-0.978147600733806));
#29043=DIRECTION('ref_axis',(0.912095473942773,0.353347669066046,0.207911690817759));
#29044=DIRECTION('center_axis',(-0.193871877856065,-0.0751063656107956,
0.978147600733806));
#29045=DIRECTION('ref_axis',(0.912095473942773,0.353347669066046,0.207911690817759));
#29046=DIRECTION('center_axis',(0.,0.,-1.));
#29047=DIRECTION('ref_axis',(0.932472229404352,0.361241666187163,1.58735880974294E-16));
#29048=DIRECTION('center_axis',(0.193871877856065,0.0751063656107956,-0.978147600733806));
#29049=DIRECTION('ref_axis',(-0.912095473942774,-0.353347669066046,-0.207911690817759));
#29050=DIRECTION('center_axis',(0.207911690817759,0.,-0.978147600733806));
#29051=DIRECTION('ref_axis',(-0.978147600733806,0.,-0.207911690817759));
#29052=DIRECTION('center_axis',(-0.207911690817759,0.,0.978147600733806));
#29053=DIRECTION('ref_axis',(0.978147600733806,0.,0.207911690817759));
#29054=DIRECTION('center_axis',(-0.207911690817759,0.,0.978147600733806));
#29055=DIRECTION('ref_axis',(0.978147600733806,0.,0.207911690817759));
#29056=DIRECTION('center_axis',(-0.207911690817759,0.,0.978147600733806));
#29057=DIRECTION('ref_axis',(0.978147600733806,0.,0.207911690817759));
#29058=DIRECTION('center_axis',(-0.207911690817759,0.,0.978147600733806));
#29059=DIRECTION('ref_axis',(0.978147600733806,0.,0.207911690817759));
#29060=DIRECTION('center_axis',(-0.207911690817759,0.,0.978147600733806));
#29061=DIRECTION('ref_axis',(0.978147600733806,0.,0.207911690817759));
#29062=DIRECTION('center_axis',(-0.207911690817759,0.,0.978147600733806));
#29063=DIRECTION('ref_axis',(0.978147600733806,1.96011575733601E-14,0.207911690817759));
#29064=DIRECTION('center_axis',(-0.207911690817759,0.,0.978147600733806));
#29065=DIRECTION('ref_axis',(0.978147600733806,0.,0.207911690817759));
#29066=DIRECTION('center_axis',(0.207911690817759,0.,-0.978147600733806));
#29067=DIRECTION('ref_axis',(0.978147600733806,0.,0.207911690817759));
#29068=DIRECTION('center_axis',(0.207911690817759,0.,-0.978147600733806));
#29069=DIRECTION('ref_axis',(0.978147600733806,0.,0.207911690817759));
#29070=DIRECTION('center_axis',(-0.207911690817759,0.,0.978147600733806));
#29071=DIRECTION('ref_axis',(0.978147600733806,0.,0.207911690817759));
#29072=DIRECTION('center_axis',(0.,0.,-1.));
#29073=DIRECTION('ref_axis',(1.,8.77688512853447E-14,1.58735880974294E-16));
#29074=DIRECTION('center_axis',(0.193871877856065,-0.0751063656107956,-0.978147600733806));
#29075=DIRECTION('ref_axis',(-0.912095473942774,0.353347669066046,-0.207911690817759));
#29076=DIRECTION('center_axis',(-0.193871877856065,0.0751063656107956,0.978147600733806));
#29077=DIRECTION('ref_axis',(0.912095473942773,-0.353347669066046,0.207911690817759));
#29078=DIRECTION('',(-0.361241666187153,-0.932472229404356,0.));
#29079=DIRECTION('center_axis',(0.193871877856065,-0.0751063656107956,-0.978147600733806));
#29080=DIRECTION('ref_axis',(0.912095473942773,-0.353347669066046,0.207911690817759));
#29081=DIRECTION('center_axis',(0.,0.,-1.));
#29082=DIRECTION('ref_axis',(-0.932472229404348,0.361241666187173,1.58735880974294E-16));
#29083=DIRECTION('center_axis',(0.,0.,-1.));
#29084=DIRECTION('ref_axis',(1.,0.,0.));
#29085=DIRECTION('center_axis',(0.,0.,1.));
#29086=DIRECTION('ref_axis',(1.,0.,0.));
#29087=DIRECTION('',(-0.173648177666931,-2.12657684957577E-17,-0.984807753012208));
#29088=DIRECTION('center_axis',(0.,0.,1.));
#29089=DIRECTION('ref_axis',(1.,0.,0.));
#29090=DIRECTION('center_axis',(0.,0.,1.));
#29091=DIRECTION('ref_axis',(1.,0.,0.));
#29092=DIRECTION('center_axis',(0.,0.,1.));
#29093=DIRECTION('ref_axis',(1.,0.,0.));
#29094=DIRECTION('center_axis',(0.,0.,1.));
#29095=DIRECTION('ref_axis',(1.,0.,0.));
#29096=DIRECTION('center_axis',(0.,0.,1.));
#29097=DIRECTION('ref_axis',(1.,0.,0.));
#29098=DIRECTION('center_axis',(0.,0.,1.));
#29099=DIRECTION('ref_axis',(1.,0.,0.));
#29100=DIRECTION('center_axis',(0.,0.,1.));
#29101=DIRECTION('ref_axis',(1.,0.,0.));
#29102=DIRECTION('center_axis',(0.,0.,1.));
#29103=DIRECTION('ref_axis',(1.,0.,0.));
#29104=DIRECTION('center_axis',(0.,0.,1.));
#29105=DIRECTION('ref_axis',(1.,0.,0.));
#29106=DIRECTION('center_axis',(0.,0.,1.));
#29107=DIRECTION('ref_axis',(1.,0.,0.));
#29108=DIRECTION('center_axis',(0.,0.,1.));
#29109=DIRECTION('ref_axis',(1.,0.,0.));
#29110=DIRECTION('center_axis',(0.,0.,1.));
#29111=DIRECTION('ref_axis',(1.,0.,0.));
#29112=DIRECTION('center_axis',(0.,0.,1.));
#29113=DIRECTION('ref_axis',(1.,0.,0.));
#29114=DIRECTION('center_axis',(0.,0.,1.));
#29115=DIRECTION('ref_axis',(1.,0.,0.));
#29116=DIRECTION('center_axis',(0.,0.,1.));
#29117=DIRECTION('ref_axis',(1.,0.,0.));
#29118=DIRECTION('center_axis',(0.,0.,1.));
#29119=DIRECTION('ref_axis',(1.,0.,0.));
#29120=DIRECTION('center_axis',(0.,0.,1.));
#29121=DIRECTION('ref_axis',(1.,0.,0.));
#29122=DIRECTION('center_axis',(0.,0.,1.));
#29123=DIRECTION('ref_axis',(1.,0.,0.));
#29124=DIRECTION('center_axis',(0.153648593508749,-0.140069200367114,-0.978147600733806));
#29125=DIRECTION('ref_axis',(-0.722859799300275,0.658973777457697,-0.207911690817759));
#29126=DIRECTION('center_axis',(-0.153648593508749,0.140069200367114,0.978147600733806));
#29127=DIRECTION('ref_axis',(0.722859799300275,-0.658973777457697,0.207911690817759));
#29128=DIRECTION('',(-0.673695643646557,-0.739008917220659,0.));
#29129=DIRECTION('center_axis',(0.153648593508749,-0.140069200367114,-0.978147600733806));
#29130=DIRECTION('ref_axis',(0.722859799300276,-0.658973777457697,0.207911690817759));
#29131=DIRECTION('center_axis',(0.,0.,-1.));
#29132=DIRECTION('ref_axis',(-0.739008917220659,0.673695643646558,1.58735880974294E-16));
#29133=DIRECTION('center_axis',(0.0926742152118281,-0.186114913463622,-0.978147600733806));
#29134=DIRECTION('ref_axis',(-0.435997903257853,0.875601825703931,-0.207911690817759));
#29135=DIRECTION('center_axis',(-0.0926742152118281,0.186114913463622,0.978147600733806));
#29136=DIRECTION('ref_axis',(0.435997903257853,-0.875601825703931,0.207911690817759));
#29137=DIRECTION('',(-0.895163291355062,-0.445738355776538,0.));
#29138=DIRECTION('center_axis',(0.0926742152118281,-0.186114913463622,-0.978147600733806));
#29139=DIRECTION('ref_axis',(0.435997903257853,-0.875601825703931,0.207911690817759));
#29140=DIRECTION('center_axis',(0.,0.,-1.));
#29141=DIRECTION('ref_axis',(-0.445738355776558,0.895163291355053,1.58735880974294E-16));
#29142=DIRECTION('center_axis',(0.0191836706249958,-0.207024776198529,-0.978147600733806));
#29143=DIRECTION('ref_axis',(-0.0902520744326727,0.97397499551164,-0.207911690817759));
#29144=DIRECTION('center_axis',(-0.0191836706249958,0.207024776198529,0.978147600733806));
#29145=DIRECTION('ref_axis',(0.0902520744326727,-0.97397499551164,0.207911690817759));
#29146=DIRECTION('',(-0.995734176295035,-0.0922683594633015,0.));
#29147=DIRECTION('center_axis',(0.0191836706249958,-0.207024776198529,-0.978147600733806));
#29148=DIRECTION('ref_axis',(0.0902520744326727,-0.97397499551164,0.207911690817759));
#29149=DIRECTION('center_axis',(0.,0.,-1.));
#29150=DIRECTION('ref_axis',(-0.0922683594632729,0.995734176295037,1.58735880974294E-16));
#29151=DIRECTION('center_axis',(-0.0568977349801305,-0.19997479574394,-0.978147600733806));
#29152=DIRECTION('ref_axis',(0.267682797148647,0.940807445193742,-0.207911690817759));
#29153=DIRECTION('center_axis',(0.0568977349801305,0.19997479574394,0.978147600733806));
#29154=DIRECTION('ref_axis',(-0.267682797148647,-0.940807445193742,0.207911690817759));
#29155=DIRECTION('',(-0.961825643172819,0.273662990072083,0.));
#29156=DIRECTION('center_axis',(-0.0568977349801305,-0.19997479574394,-0.978147600733806));
#29157=DIRECTION('ref_axis',(-0.267682797148647,-0.940807445193742,0.207911690817759));
#29158=DIRECTION('center_axis',(0.,0.,-1.));
#29159=DIRECTION('ref_axis',(0.273662990072067,0.961825643172824,1.58735880974294E-16));
#29160=DIRECTION('center_axis',(-0.125294786194957,-0.165917111025535,-0.978147600733806));
#29161=DIRECTION('ref_axis',(0.589465623693459,0.78057863620841,-0.207911690817759));
#29162=DIRECTION('center_axis',(0.125294786194957,0.165917111025535,0.978147600733806));
#29163=DIRECTION('ref_axis',(-0.589465623693459,-0.78057863620841,0.207911690817759));
#29164=DIRECTION('',(-0.798017227280239,0.602634636379257,0.));
#29165=DIRECTION('center_axis',(-0.125294786194957,-0.165917111025535,-0.978147600733806));
#29166=DIRECTION('ref_axis',(-0.589465623693459,-0.78057863620841,0.207911690817759));
#29167=DIRECTION('center_axis',(0.,0.,-1.));
#29168=DIRECTION('ref_axis',(0.602634636379246,0.798017227280247,1.58735880974294E-16));
#29169=DIRECTION('center_axis',(-0.176770082251776,-0.109451401084681,-0.978147600733806));
#29170=DIRECTION('ref_axis',(0.831637851416691,0.514928357067594,-0.207911690817759));
#29171=DIRECTION('center_axis',(0.176770082251776,0.109451401084681,0.978147600733806));
#29172=DIRECTION('ref_axis',(-0.83163785141669,-0.514928357067594,0.207911690817759));
#29173=DIRECTION('',(-0.526432162877356,0.850217135729614,0.));
#29174=DIRECTION('center_axis',(-0.176770082251776,-0.109451401084681,-0.978147600733806));
#29175=DIRECTION('ref_axis',(-0.831637851416691,-0.514928357067594,0.207911690817759));
#29176=DIRECTION('center_axis',(0.,0.,-1.));
#29177=DIRECTION('ref_axis',(0.85021713572961,0.526432162877362,1.58735880974294E-16));
#29178=DIRECTION('center_axis',(-0.204371599183654,-0.0382036729361911,
-0.978147600733806));
#29179=DIRECTION('ref_axis',(0.961492779041681,0.179734149988272,-0.207911690817759));
#29180=DIRECTION('center_axis',(0.204371599183654,0.0382036729361911,0.978147600733806));
#29181=DIRECTION('ref_axis',(-0.961492779041681,-0.179734149988272,0.207911690817759));
#29182=DIRECTION('',(-0.18374951781657,0.982973099683902,0.));
#29183=DIRECTION('center_axis',(-0.204371599183654,-0.0382036729361911,
-0.978147600733806));
#29184=DIRECTION('ref_axis',(-0.961492779041681,-0.179734149988272,0.207911690817759));
#29185=DIRECTION('center_axis',(0.,0.,-1.));
#29186=DIRECTION('ref_axis',(0.982973099683894,0.18374951781661,1.58735880974294E-16));
#29187=DIRECTION('center_axis',(-0.204371599183654,0.0382036729361911,-0.978147600733806));
#29188=DIRECTION('ref_axis',(0.96149277904168,-0.179734149988272,-0.207911690817759));
#29189=DIRECTION('center_axis',(0.204371599183654,-0.0382036729361911,0.978147600733806));
#29190=DIRECTION('ref_axis',(-0.961492779041681,0.179734149988272,0.207911690817759));
#29191=DIRECTION('',(0.18374951781657,0.982973099683902,0.));
#29192=DIRECTION('center_axis',(-0.204371599183654,0.0382036729361911,-0.978147600733806));
#29193=DIRECTION('ref_axis',(-0.961492779041681,0.179734149988272,0.207911690817759));
#29194=DIRECTION('center_axis',(0.,0.,-1.));
#29195=DIRECTION('ref_axis',(-0.982973099683909,0.183749517816531,1.58735880974294E-16));
#29196=DIRECTION('center_axis',(-0.176770082251776,0.109451401084681,-0.978147600733806));
#29197=DIRECTION('ref_axis',(0.83163785141669,-0.514928357067593,-0.207911690817759));
#29198=DIRECTION('center_axis',(0.176770082251776,-0.109451401084681,0.978147600733806));
#29199=DIRECTION('ref_axis',(-0.831637851416691,0.514928357067594,0.207911690817759));
#29200=DIRECTION('',(0.526432162877356,0.850217135729614,0.));
#29201=DIRECTION('center_axis',(-0.176770082251776,0.109451401084681,-0.978147600733806));
#29202=DIRECTION('ref_axis',(-0.831637851416691,0.514928357067593,0.207911690817759));
#29203=DIRECTION('center_axis',(0.,0.,-1.));
#29204=DIRECTION('ref_axis',(-0.850217135729556,0.52643216287745,1.58735880974294E-16));
#29205=DIRECTION('center_axis',(-0.125294786194957,0.165917111025535,-0.978147600733806));
#29206=DIRECTION('ref_axis',(0.589465623693459,-0.78057863620841,-0.207911690817759));
#29207=DIRECTION('center_axis',(0.125294786194957,-0.165917111025535,0.978147600733806));
#29208=DIRECTION('ref_axis',(-0.589465623693459,0.78057863620841,0.207911690817759));
#29209=DIRECTION('',(0.79801722728024,0.602634636379256,0.));
#29210=DIRECTION('center_axis',(-0.125294786194957,0.165917111025535,-0.978147600733806));
#29211=DIRECTION('ref_axis',(-0.589465623693459,0.78057863620841,0.207911690817759));
#29212=DIRECTION('center_axis',(0.,0.,-1.));
#29213=DIRECTION('ref_axis',(-0.602634636379309,0.7980172272802,1.58735880974294E-16));
#29214=DIRECTION('center_axis',(-0.0568977349801304,0.19997479574394,-0.978147600733806));
#29215=DIRECTION('ref_axis',(0.267682797148647,-0.940807445193742,-0.207911690817759));
#29216=DIRECTION('center_axis',(0.0568977349801304,-0.19997479574394,0.978147600733806));
#29217=DIRECTION('ref_axis',(-0.267682797148647,0.940807445193742,0.207911690817759));
#29218=DIRECTION('',(0.961825643172819,0.273662990072083,0.));
#29219=DIRECTION('center_axis',(-0.0568977349801304,0.19997479574394,-0.978147600733806));
#29220=DIRECTION('ref_axis',(-0.267682797148647,0.940807445193742,0.207911690817759));
#29221=DIRECTION('center_axis',(0.,0.,-1.));
#29222=DIRECTION('ref_axis',(-0.273662990072115,0.96182564317281,1.58735880974294E-16));
#29223=DIRECTION('center_axis',(0.0191836706249959,0.207024776198529,-0.978147600733806));
#29224=DIRECTION('ref_axis',(-0.0902520744326732,-0.97397499551164,-0.207911690817759));
#29225=DIRECTION('center_axis',(-0.0191836706249959,-0.207024776198529,
0.978147600733806));
#29226=DIRECTION('ref_axis',(0.0902520744326732,0.97397499551164,0.207911690817759));
#29227=DIRECTION('',(0.995734176295035,-0.092268359463302,0.));
#29228=DIRECTION('center_axis',(0.0191836706249959,0.207024776198529,-0.978147600733806));
#29229=DIRECTION('ref_axis',(0.0902520744326732,0.97397499551164,0.207911690817759));
#29230=DIRECTION('center_axis',(0.,0.,-1.));
#29231=DIRECTION('ref_axis',(0.0922683594632895,0.995734176295036,1.58735880974294E-16));
#29232=DIRECTION('center_axis',(0.092674215211828,0.186114913463622,-0.978147600733806));
#29233=DIRECTION('ref_axis',(-0.435997903257852,-0.875601825703931,-0.207911690817759));
#29234=DIRECTION('center_axis',(-0.092674215211828,-0.186114913463622,0.978147600733806));
#29235=DIRECTION('ref_axis',(0.435997903257852,0.875601825703931,0.207911690817759));
#29236=DIRECTION('',(0.895163291355062,-0.445738355776538,0.));
#29237=DIRECTION('center_axis',(0.092674215211828,0.186114913463622,-0.978147600733806));
#29238=DIRECTION('ref_axis',(0.435997903257852,0.875601825703931,0.207911690817759));
#29239=DIRECTION('center_axis',(0.,0.,-1.));
#29240=DIRECTION('ref_axis',(0.445738355776574,0.895163291355045,1.58735880974294E-16));
#29241=DIRECTION('center_axis',(0.153648593508749,0.140069200367114,-0.978147600733806));
#29242=DIRECTION('ref_axis',(-0.722859799300275,-0.658973777457697,-0.207911690817759));
#29243=DIRECTION('center_axis',(-0.153648593508749,-0.140069200367114,0.978147600733806));
#29244=DIRECTION('ref_axis',(0.722859799300275,0.658973777457697,0.207911690817759));
#29245=DIRECTION('',(0.673695643646557,-0.739008917220659,0.));
#29246=DIRECTION('center_axis',(0.153648593508749,0.140069200367114,-0.978147600733806));
#29247=DIRECTION('ref_axis',(0.722859799300275,0.658973777457697,0.207911690817759));
#29248=DIRECTION('center_axis',(0.,0.,-1.));
#29249=DIRECTION('ref_axis',(0.739008917220659,0.673695643646557,1.58735880974294E-16));
#29250=DIRECTION('center_axis',(0.193871877856065,0.0751063656107956,-0.978147600733806));
#29251=DIRECTION('ref_axis',(-0.912095473942774,-0.353347669066046,-0.207911690817759));
#29252=DIRECTION('center_axis',(-0.193871877856065,-0.0751063656107956,
0.978147600733806));
#29253=DIRECTION('ref_axis',(0.912095473942773,0.353347669066046,0.207911690817759));
#29254=DIRECTION('',(0.361241666187153,-0.932472229404356,0.));
#29255=DIRECTION('center_axis',(0.193871877856065,0.0751063656107956,-0.978147600733806));
#29256=DIRECTION('ref_axis',(0.912095473942773,0.353347669066046,0.207911690817759));
#29257=DIRECTION('center_axis',(0.,0.,-1.));
#29258=DIRECTION('ref_axis',(0.932472229404352,0.361241666187163,1.58735880974294E-16));
#29259=DIRECTION('center_axis',(0.207911690817759,0.,-0.978147600733806));
#29260=DIRECTION('ref_axis',(0.978147600733806,0.,0.207911690817759));
#29261=DIRECTION('center_axis',(0.,0.,-1.));
#29262=DIRECTION('ref_axis',(1.,8.77688512853447E-14,1.58735880974294E-16));
#29263=DIRECTION('center_axis',(-0.207911690817759,0.,0.978147600733806));
#29264=DIRECTION('ref_axis',(0.978147600733806,0.,0.207911690817759));
#29265=DIRECTION('center_axis',(0.207911690817759,0.,-0.978147600733806));
#29266=DIRECTION('ref_axis',(-0.978147600733806,0.,-0.207911690817759));
#29267=DIRECTION('',(0.,-1.,0.));
#29268=DIRECTION('center_axis',(0.,0.,-1.));
#29269=DIRECTION('ref_axis',(1.,0.,0.));
#29270=DIRECTION('center_axis',(0.,0.,1.));
#29271=DIRECTION('ref_axis',(1.,0.,0.));
#29272=DIRECTION('',(-0.707106781186548,-8.65956056235494E-17,-0.707106781186547));
#29273=DIRECTION('center_axis',(0.,0.,1.));
#29274=DIRECTION('ref_axis',(1.,0.,0.));
#29275=DIRECTION('center_axis',(0.,0.,-1.));
#29276=DIRECTION('ref_axis',(-1.,0.,0.));
#29277=DIRECTION('center_axis',(0.,0.,1.));
#29278=DIRECTION('ref_axis',(1.,0.,0.));
#29279=DIRECTION('center_axis',(0.,0.,1.));
#29280=DIRECTION('ref_axis',(1.,0.,0.));
#29281=DIRECTION('center_axis',(0.,0.,1.));
#29282=DIRECTION('ref_axis',(1.,0.,0.));
#29283=DIRECTION('',(0.707106781186548,8.65956056235494E-17,-0.707106781186547));
#29284=DIRECTION('center_axis',(0.,0.,1.));
#29285=DIRECTION('ref_axis',(1.,0.,0.));
#29286=DIRECTION('center_axis',(0.,0.,1.));
#29287=DIRECTION('ref_axis',(1.,0.,0.));
#29288=DIRECTION('',(0.,0.,-1.));
#29289=DIRECTION('center_axis',(0.,0.,1.));
#29290=DIRECTION('ref_axis',(1.,0.,0.));
#29291=DIRECTION('center_axis',(0.,0.,-1.));
#29292=DIRECTION('ref_axis',(-1.,0.,0.));
#29293=DIRECTION('center_axis',(0.,0.,1.));
#29294=DIRECTION('ref_axis',(1.,0.,0.));
#29295=DIRECTION('center_axis',(0.,0.,1.));
#29296=DIRECTION('ref_axis',(1.,0.,0.));
#29297=DIRECTION('center_axis',(0.,0.,1.));
#29298=DIRECTION('ref_axis',(1.,0.,0.));
#29299=DIRECTION('',(0.,0.,-1.));
#29300=DIRECTION('center_axis',(0.,0.,1.));
#29301=DIRECTION('ref_axis',(1.,0.,0.));
#29302=DIRECTION('center_axis',(0.,0.,1.));
#29303=DIRECTION('ref_axis',(1.,0.,0.));
#29304=DIRECTION('center_axis',(0.,0.,1.));
#29305=DIRECTION('ref_axis',(1.,0.,0.));
#29306=DIRECTION('',(0.707106781186547,8.65956056235493E-17,-0.707106781186547));
#29307=DIRECTION('center_axis',(0.,0.,1.));
#29308=DIRECTION('ref_axis',(1.,0.,0.));
#29309=DIRECTION('center_axis',(0.,0.,1.));
#29310=DIRECTION('ref_axis',(1.,0.,0.));
#29311=DIRECTION('',(0.,0.,-1.));
#29312=DIRECTION('axis',(0.,0.,1.));
#29313=DIRECTION('refdir',(1.,0.,0.));
#29314=DIRECTION('center_axis',(0.,0.,-1.));
#29315=DIRECTION('ref_axis',(1.,0.,0.));
#29316=DIRECTION('center_axis',(0.,0.,1.));
#29317=DIRECTION('ref_axis',(1.,0.,0.));
#29318=DIRECTION('',(-0.780704907087438,-9.56087765543263E-17,-0.624899870418929));
#29319=DIRECTION('center_axis',(0.,0.,1.));
#29320=DIRECTION('ref_axis',(1.,0.,0.));
#29321=DIRECTION('center_axis',(0.,0.,-1.));
#29322=DIRECTION('ref_axis',(-1.,0.,0.));
#29323=DIRECTION('center_axis',(0.,0.,1.));
#29324=DIRECTION('ref_axis',(1.,0.,0.));
#29325=DIRECTION('center_axis',(0.,0.,1.));
#29326=DIRECTION('ref_axis',(1.,0.,0.));
#29327=DIRECTION('center_axis',(0.,0.,1.));
#29328=DIRECTION('ref_axis',(1.,0.,0.));
#29329=DIRECTION('',(0.707106781186548,8.65956056235494E-17,-0.707106781186547));
#29330=DIRECTION('center_axis',(0.,0.,1.));
#29331=DIRECTION('ref_axis',(1.,0.,0.));
#29332=DIRECTION('center_axis',(0.,0.,1.));
#29333=DIRECTION('ref_axis',(1.,0.,0.));
#29334=DIRECTION('',(0.,0.,-1.));
#29335=DIRECTION('center_axis',(0.,0.,-1.));
#29336=DIRECTION('ref_axis',(1.,0.,0.));
#29337=DIRECTION('center_axis',(0.,0.,1.));
#29338=DIRECTION('ref_axis',(1.,0.,0.));
#29339=DIRECTION('',(-0.707106781186548,-8.65956056235493E-17,-0.707106781186548));
#29340=DIRECTION('center_axis',(0.,0.,1.));
#29341=DIRECTION('ref_axis',(1.,0.,0.));
#29342=DIRECTION('center_axis',(0.,0.,1.));
#29343=DIRECTION('ref_axis',(1.,0.,0.));
#29344=DIRECTION('center_axis',(0.,0.,1.));
#29345=DIRECTION('ref_axis',(1.,0.,0.));
#29346=DIRECTION('',(0.600343896113564,7.35209230763127E-17,-0.79974196238486));
#29347=DIRECTION('center_axis',(0.,0.,1.));
#29348=DIRECTION('ref_axis',(1.,0.,0.));
#29349=DIRECTION('center_axis',(0.,0.,-1.));
#29350=DIRECTION('ref_axis',(1.,0.,0.));
#29351=DIRECTION('',(-0.241921895599668,-2.96268875089794E-17,-0.970295726275996));
#29352=DIRECTION('axis',(0.,0.,1.));
#29353=DIRECTION('refdir',(1.,0.,0.));
#29354=DIRECTION('center_axis',(0.,0.,-1.));
#29355=DIRECTION('ref_axis',(1.,0.,0.));
#29356=DIRECTION('center_axis',(0.,0.,-1.));
#29357=DIRECTION('ref_axis',(1.,0.,0.));
#29358=DIRECTION('',(0.,0.,-1.));
#29359=DIRECTION('center_axis',(0.,0.,1.));
#29360=DIRECTION('ref_axis',(1.,0.,0.));
#29361=DIRECTION('center_axis',(0.,0.,-1.));
#29362=DIRECTION('ref_axis',(1.,0.,0.));
#29363=DIRECTION('center_axis',(0.,0.,-1.));
#29364=DIRECTION('ref_axis',(1.,0.,0.));
#29365=DIRECTION('',(0.,0.,-1.));
#29366=DIRECTION('center_axis',(0.,0.,1.));
#29367=DIRECTION('ref_axis',(1.,0.,0.));
#29368=DIRECTION('center_axis',(0.529919264233205,-0.848048096156426,0.));
#29369=DIRECTION('ref_axis',(0.848048096156426,0.529919264233205,0.));
#29370=DIRECTION('',(-0.848048096156426,-0.529919264233205,0.));
#29371=DIRECTION('',(0.,0.,1.));
#29372=DIRECTION('',(0.848048096156426,0.529919264233205,0.));
#29373=DIRECTION('',(0.,0.,1.));
#29374=DIRECTION('center_axis',(0.,0.,1.));
#29375=DIRECTION('ref_axis',(-0.8811002033343,0.472929626566422,0.));
#29376=DIRECTION('center_axis',(0.,0.,1.));
#29377=DIRECTION('ref_axis',(-0.8811002033343,0.472929626566422,0.));
#29378=DIRECTION('center_axis',(0.,0.,1.));
#29379=DIRECTION('ref_axis',(-0.8811002033343,0.472929626566422,0.));
#29380=DIRECTION('',(0.,0.,1.));
#29381=DIRECTION('center_axis',(-0.241921895599668,0.970295726275997,0.));
#29382=DIRECTION('ref_axis',(-0.970295726275997,-0.241921895599668,0.));
#29383=DIRECTION('',(0.970295726275997,0.241921895599668,0.));
#29384=DIRECTION('',(-0.970295726275997,-0.241921895599668,0.));
#29385=DIRECTION('',(0.,0.,1.));
#29386=DIRECTION('center_axis',(0.,0.,1.));
#29387=DIRECTION('ref_axis',(1.,-4.64528462186258E-17,0.));
#29388=DIRECTION('center_axis',(0.,0.,1.));
#29389=DIRECTION('ref_axis',(-0.970295726275996,-0.241921895599668,0.));
#29390=DIRECTION('center_axis',(0.,0.,-1.));
#29391=DIRECTION('ref_axis',(-0.970295726275996,-0.241921895599668,0.));
#29392=DIRECTION('',(0.,0.,1.));
#29393=DIRECTION('center_axis',(-0.241921895599668,-0.970295726275996,0.));
#29394=DIRECTION('ref_axis',(0.970295726275996,-0.241921895599668,0.));
#29395=DIRECTION('',(-0.970295726275996,0.241921895599668,0.));
#29396=DIRECTION('',(0.970295726275996,-0.241921895599668,0.));
#29397=DIRECTION('',(0.,0.,1.));
#29398=DIRECTION('center_axis',(0.,0.,1.));
#29399=DIRECTION('ref_axis',(-0.060878153376398,0.998145205088658,0.));
#29400=DIRECTION('center_axis',(0.,0.,1.));
#29401=DIRECTION('ref_axis',(-0.060878153376398,0.998145205088658,0.));
#29402=DIRECTION('center_axis',(0.,0.,1.));
#29403=DIRECTION('ref_axis',(-0.060878153376398,0.998145205088658,0.));
#29404=DIRECTION('',(0.,0.,1.));
#29405=DIRECTION('center_axis',(0.529919264233205,0.848048096156426,0.));
#29406=DIRECTION('ref_axis',(-0.848048096156426,0.529919264233205,0.));
#29407=DIRECTION('',(0.848048096156426,-0.529919264233205,0.));
#29408=DIRECTION('',(-0.848048096156426,0.529919264233205,0.));
#29409=DIRECTION('',(0.,0.,1.));
#29410=DIRECTION('center_axis',(0.,0.,1.));
#29411=DIRECTION('ref_axis',(1.,-1.45127192761458E-16,0.));
#29412=DIRECTION('center_axis',(0.,0.,1.));
#29413=DIRECTION('ref_axis',(-0.848048096156426,-0.529919264233205,0.));
#29414=DIRECTION('center_axis',(0.,0.,1.));
#29415=DIRECTION('ref_axis',(-0.848048096156426,-0.529919264233205,0.));
#29416=DIRECTION('center_axis',(0.,0.,1.));
#29417=DIRECTION('ref_axis',(1.,0.,0.));
#29418=DIRECTION('center_axis',(0.,0.,1.));
#29419=DIRECTION('ref_axis',(1.,0.,0.));
#29420=DIRECTION('axis',(0.,0.,1.));
#29421=DIRECTION('refdir',(1.,0.,0.));
#29422=DIRECTION('center_axis',(0.,0.,1.));
#29423=DIRECTION('ref_axis',(1.,0.,0.));
#29424=DIRECTION('',(0.,0.,-1.));
#29425=DIRECTION('center_axis',(0.,0.,-1.));
#29426=DIRECTION('ref_axis',(1.,0.,0.));
#29427=DIRECTION('',(0.,0.,-1.));
#29428=DIRECTION('center_axis',(0.,0.,1.));
#29429=DIRECTION('ref_axis',(1.,0.,0.));
#29430=DIRECTION('center_axis',(0.,0.,-1.));
#29431=DIRECTION('ref_axis',(1.,0.,0.));
#29432=DIRECTION('center_axis',(0.,0.,1.));
#29433=DIRECTION('ref_axis',(1.,0.,0.));
#29434=DIRECTION('',(0.,0.,-1.));
#29435=DIRECTION('center_axis',(0.,0.,1.));
#29436=DIRECTION('ref_axis',(1.,0.,0.));
#29437=DIRECTION('',(0.,0.,-1.));
#29438=DIRECTION('center_axis',(0.,0.,1.));
#29439=DIRECTION('ref_axis',(1.,0.,0.));
#29440=DIRECTION('',(0.,0.,-1.));
#29441=DIRECTION('center_axis',(0.,0.,1.));
#29442=DIRECTION('ref_axis',(1.,0.,0.));
#29443=DIRECTION('',(0.,0.,-1.));
#29444=DIRECTION('center_axis',(0.,0.,1.));
#29445=DIRECTION('ref_axis',(1.,0.,0.));
#29446=DIRECTION('',(0.,0.,-1.));
#29447=DIRECTION('center_axis',(0.,0.,1.));
#29448=DIRECTION('ref_axis',(1.,0.,0.));
#29449=DIRECTION('',(0.,0.,-1.));
#29450=DIRECTION('center_axis',(0.,0.,1.));
#29451=DIRECTION('ref_axis',(1.,0.,0.));
#29452=DIRECTION('',(0.,0.,-1.));
#29453=DIRECTION('center_axis',(0.,0.,1.));
#29454=DIRECTION('ref_axis',(1.,0.,0.));
#29455=DIRECTION('',(0.,0.,-1.));
#29456=DIRECTION('center_axis',(0.,0.,1.));
#29457=DIRECTION('ref_axis',(1.,0.,0.));
#29458=DIRECTION('',(0.,0.,-1.));
#29459=DIRECTION('center_axis',(0.,0.,1.));
#29460=DIRECTION('ref_axis',(1.,0.,0.));
#29461=DIRECTION('',(0.,0.,-1.));
#29462=DIRECTION('center_axis',(0.,0.,1.));
#29463=DIRECTION('ref_axis',(1.,0.,0.));
#29464=DIRECTION('',(0.,0.,-1.));
#29465=DIRECTION('center_axis',(0.,0.,1.));
#29466=DIRECTION('ref_axis',(1.,0.,0.));
#29467=DIRECTION('',(0.,0.,-1.));
#29468=DIRECTION('center_axis',(0.,0.,1.));
#29469=DIRECTION('ref_axis',(1.,0.,0.));
#29470=DIRECTION('',(0.,0.,-1.));
#29471=DIRECTION('center_axis',(0.,0.,1.));
#29472=DIRECTION('ref_axis',(1.,0.,0.));
#29473=DIRECTION('',(0.,0.,-1.));
#29474=DIRECTION('center_axis',(0.,0.,1.));
#29475=DIRECTION('ref_axis',(1.,0.,0.));
#29476=DIRECTION('',(0.,0.,-1.));
#29477=DIRECTION('center_axis',(0.,0.,1.));
#29478=DIRECTION('ref_axis',(1.,0.,0.));
#29479=DIRECTION('',(0.,0.,-1.));
#29480=DIRECTION('center_axis',(0.,0.,1.));
#29481=DIRECTION('ref_axis',(1.,0.,0.));
#29482=DIRECTION('',(0.,0.,-1.));
#29483=DIRECTION('center_axis',(0.,0.,1.));
#29484=DIRECTION('ref_axis',(1.,0.,0.));
#29485=DIRECTION('',(0.,0.,-1.));
#29486=DIRECTION('center_axis',(0.,0.,1.));
#29487=DIRECTION('ref_axis',(1.,0.,0.));
#29488=DIRECTION('',(0.,0.,-1.));
#29489=DIRECTION('center_axis',(0.,0.,1.));
#29490=DIRECTION('ref_axis',(1.,0.,0.));
#29491=DIRECTION('',(0.,0.,-1.));
#29492=DIRECTION('center_axis',(0.,0.,1.));
#29493=DIRECTION('ref_axis',(1.,0.,0.));
#29494=DIRECTION('',(0.,0.,-1.));
#29495=DIRECTION('center_axis',(0.,0.,1.));
#29496=DIRECTION('ref_axis',(1.,0.,0.));
#29497=DIRECTION('',(0.,0.,-1.));
#29498=DIRECTION('center_axis',(0.,0.,1.));
#29499=DIRECTION('ref_axis',(1.,0.,0.));
#29500=DIRECTION('center_axis',(0.,0.,1.));
#29501=DIRECTION('ref_axis',(0.315430408607799,-0.948948711641213,0.));
#29502=DIRECTION('',(0.,0.,1.));
#29503=DIRECTION('center_axis',(0.,0.,1.));
#29504=DIRECTION('ref_axis',(1.,4.63459159752748E-15,0.));
#29505=DIRECTION('center_axis',(0.,0.,1.));
#29506=DIRECTION('ref_axis',(1.,4.63459159752748E-15,0.));
#29507=DIRECTION('',(0.,0.,1.));
#29508=DIRECTION('center_axis',(0.,0.,1.));
#29509=DIRECTION('ref_axis',(1.,4.63459159752748E-15,0.));
#29510=DIRECTION('',(0.,0.,1.));
#29511=DIRECTION('center_axis',(0.,0.,1.));
#29512=DIRECTION('ref_axis',(1.,4.63459159752748E-15,0.));
#29513=DIRECTION('',(0.,0.,1.));
#29514=DIRECTION('center_axis',(0.,0.,1.));
#29515=DIRECTION('ref_axis',(1.,4.63459159752748E-15,0.));
#29516=DIRECTION('',(0.,0.,1.));
#29517=DIRECTION('center_axis',(0.,0.,1.));
#29518=DIRECTION('ref_axis',(1.,4.63459159752748E-15,0.));
#29519=DIRECTION('',(0.,0.,1.));
#29520=DIRECTION('center_axis',(0.,0.,1.));
#29521=DIRECTION('ref_axis',(1.,4.63459159752748E-15,0.));
#29522=DIRECTION('',(0.,0.,1.));
#29523=DIRECTION('center_axis',(0.,0.,1.));
#29524=DIRECTION('ref_axis',(1.,4.63459159752748E-15,0.));
#29525=DIRECTION('',(0.,0.,1.));
#29526=DIRECTION('center_axis',(0.,0.,1.));
#29527=DIRECTION('ref_axis',(1.,4.63459159752748E-15,0.));
#29528=DIRECTION('',(0.,0.,1.));
#29529=DIRECTION('center_axis',(0.,0.,1.));
#29530=DIRECTION('ref_axis',(1.,4.63459159752748E-15,0.));
#29531=DIRECTION('',(0.,0.,1.));
#29532=DIRECTION('center_axis',(0.,0.,1.));
#29533=DIRECTION('ref_axis',(1.,4.63459159752748E-15,0.));
#29534=DIRECTION('',(0.,0.,1.));
#29535=DIRECTION('center_axis',(0.,0.,1.));
#29536=DIRECTION('ref_axis',(1.,4.63459159752748E-15,0.));
#29537=DIRECTION('',(0.,0.,1.));
#29538=DIRECTION('center_axis',(0.,0.,1.));
#29539=DIRECTION('ref_axis',(1.,4.63459159752748E-15,0.));
#29540=DIRECTION('',(0.,0.,1.));
#29541=DIRECTION('center_axis',(0.,0.,1.));
#29542=DIRECTION('ref_axis',(1.,4.63459159752748E-15,0.));
#29543=DIRECTION('',(0.,0.,1.));
#29544=DIRECTION('center_axis',(0.,0.,1.));
#29545=DIRECTION('ref_axis',(1.,4.63459159752748E-15,0.));
#29546=DIRECTION('',(0.,0.,1.));
#29547=DIRECTION('center_axis',(0.,0.,1.));
#29548=DIRECTION('ref_axis',(1.,4.63459159752748E-15,0.));
#29549=DIRECTION('',(0.,0.,1.));
#29550=DIRECTION('center_axis',(0.,0.,1.));
#29551=DIRECTION('ref_axis',(1.,4.63459159752748E-15,0.));
#29552=DIRECTION('',(0.,0.,1.));
#29553=DIRECTION('center_axis',(0.,0.,1.));
#29554=DIRECTION('ref_axis',(1.,4.63459159752748E-15,0.));
#29555=DIRECTION('',(0.,0.,1.));
#29556=DIRECTION('center_axis',(0.,0.,1.));
#29557=DIRECTION('ref_axis',(1.,4.63459159752748E-15,0.));
#29558=DIRECTION('',(0.,0.,1.));
#29559=DIRECTION('center_axis',(0.,0.,1.));
#29560=DIRECTION('ref_axis',(1.,4.63459159752748E-15,0.));
#29561=DIRECTION('',(0.,0.,1.));
#29562=DIRECTION('center_axis',(0.,0.,1.));
#29563=DIRECTION('ref_axis',(1.,4.63459159752748E-15,0.));
#29564=DIRECTION('',(0.,0.,1.));
#29565=DIRECTION('center_axis',(0.,0.,1.));
#29566=DIRECTION('ref_axis',(1.,4.63459159752748E-15,0.));
#29567=DIRECTION('',(0.,0.,1.));
#29568=DIRECTION('center_axis',(0.,0.,1.));
#29569=DIRECTION('ref_axis',(1.,0.,0.));
#29570=DIRECTION('center_axis',(0.,0.,1.));
#29571=DIRECTION('ref_axis',(1.,0.,0.));
#29572=DIRECTION('center_axis',(0.,0.,1.));
#29573=DIRECTION('ref_axis',(1.,0.,0.));
#29574=DIRECTION('center_axis',(0.,0.,-1.));
#29575=DIRECTION('ref_axis',(1.,4.63459159752748E-15,0.));
#29576=DIRECTION('center_axis',(0.,0.,1.));
#29577=DIRECTION('ref_axis',(1.,4.63459159752748E-15,0.));
#29578=DIRECTION('center_axis',(0.,0.,1.));
#29579=DIRECTION('ref_axis',(-0.970925317856845,-0.239382595742849,0.));
#29580=DIRECTION('center_axis',(0.,0.,1.));
#29581=DIRECTION('ref_axis',(1.,0.,0.));
#29582=DIRECTION('center_axis',(0.,0.,1.));
#29583=DIRECTION('ref_axis',(1.,0.,0.));
#29584=DIRECTION('center_axis',(1.22464679914735E-16,-1.,0.));
#29585=DIRECTION('ref_axis',(-1.,-1.22464679914735E-16,0.));
#29586=DIRECTION('center_axis',(0.,0.,-1.));
#29587=DIRECTION('ref_axis',(1.,0.,0.));
#29588=DIRECTION('center_axis',(0.,0.,-1.));
#29589=DIRECTION('ref_axis',(-1.,0.,0.));
#29590=DIRECTION('center_axis',(0.,0.,1.));
#29591=DIRECTION('ref_axis',(1.,0.,0.));
#29592=DIRECTION('center_axis',(0.,0.,1.));
#29593=DIRECTION('ref_axis',(1.,0.,0.));
#29594=DIRECTION('',(-0.8574862672191,-1.05011781246268E-16,0.514506852753833));
#29595=DIRECTION('center_axis',(0.,0.,-1.));
#29596=DIRECTION('ref_axis',(1.,0.,0.));
#29597=DIRECTION('center_axis',(0.866025403784439,0.5,0.));
#29598=DIRECTION('ref_axis',(0.5,-0.866025403784439,0.));
#29599=DIRECTION('',(0.5,-0.866025403784439,0.));
#29600=DIRECTION('',(0.,0.,-1.));
#29601=DIRECTION('',(0.5,-0.866025403784439,0.));
#29602=DIRECTION('',(0.,0.,-1.));
#29603=DIRECTION('center_axis',(1.60246890531964E-16,1.,0.));
#29604=DIRECTION('ref_axis',(1.,-1.60246890531964E-16,0.));
#29605=DIRECTION('',(1.,-1.60246890531964E-16,0.));
#29606=DIRECTION('',(0.,0.,-1.));
#29607=DIRECTION('',(1.,-1.60246890531964E-16,0.));
#29608=DIRECTION('center_axis',(-0.866025403784439,0.5,0.));
#29609=DIRECTION('ref_axis',(0.5,0.866025403784439,0.));
#29610=DIRECTION('',(0.5,0.866025403784439,0.));
#29611=DIRECTION('',(0.,0.,-1.));
#29612=DIRECTION('',(0.5,0.866025403784439,0.));
#29613=DIRECTION('center_axis',(-0.866025403784439,-0.5,0.));
#29614=DIRECTION('ref_axis',(-0.5,0.866025403784439,0.));
#29615=DIRECTION('',(-0.5,0.866025403784439,0.));
#29616=DIRECTION('',(0.,0.,-1.));
#29617=DIRECTION('',(-0.5,0.866025403784439,0.));
#29618=DIRECTION('center_axis',(-1.60246890531964E-16,-1.,0.));
#29619=DIRECTION('ref_axis',(-1.,1.60246890531964E-16,0.));
#29620=DIRECTION('',(-1.,1.60246890531964E-16,0.));
#29621=DIRECTION('',(0.,0.,-1.));
#29622=DIRECTION('',(-1.,1.60246890531964E-16,0.));
#29623=DIRECTION('center_axis',(0.866025403784439,-0.5,0.));
#29624=DIRECTION('ref_axis',(-0.5,-0.866025403784439,0.));
#29625=DIRECTION('',(-0.5,-0.866025403784439,0.));
#29626=DIRECTION('',(-0.5,-0.866025403784439,0.));
#29627=DIRECTION('center_axis',(0.,0.,-1.));
#29628=DIRECTION('ref_axis',(-1.,0.,0.));
#29629=DIRECTION('center_axis',(-0.738540092256147,-0.674209560989966,0.));
#29630=DIRECTION('ref_axis',(-0.674209560989966,0.738540092256147,0.));
#29631=DIRECTION('',(0.,0.,1.));
#29632=DIRECTION('',(-0.674209560989966,0.738540092256147,0.));
#29633=DIRECTION('',(0.,0.,-1.));
#29634=DIRECTION('',(-0.674209560989966,0.738540092256147,0.));
#29635=DIRECTION('center_axis',(0.,0.,1.));
#29636=DIRECTION('ref_axis',(1.,0.,0.));
#29637=DIRECTION('center_axis',(0.,0.,1.));
#29638=DIRECTION('ref_axis',(1.,0.,0.));
#29639=DIRECTION('',(0.991198908253055,0.132380981556841,0.));
#29640=DIRECTION('center_axis',(-0.132380981556841,0.991198908253055,0.));
#29641=DIRECTION('ref_axis',(0.991198908253055,0.132380981556841,0.));
#29642=DIRECTION('',(0.,0.,-1.));
#29643=DIRECTION('',(0.991198908253055,0.132380981556841,0.));
#29644=DIRECTION('center_axis',(0.,0.,-1.));
#29645=DIRECTION('ref_axis',(-1.,0.,0.));
#29646=DIRECTION('center_axis',(0.,0.,-1.));
#29647=DIRECTION('ref_axis',(1.,0.,0.));
#29648=DIRECTION('center_axis',(-0.924593925528967,-0.380954161120384,0.));
#29649=DIRECTION('ref_axis',(-0.380954161120384,0.924593925528967,0.));
#29650=DIRECTION('',(0.,0.,1.));
#29651=DIRECTION('',(-0.380954161120384,0.924593925528967,0.));
#29652=DIRECTION('',(0.,0.,-1.));
#29653=DIRECTION('',(-0.380954161120384,0.924593925528967,0.));
#29654=DIRECTION('center_axis',(0.,0.,1.));
#29655=DIRECTION('ref_axis',(1.,0.,0.));
#29656=DIRECTION('center_axis',(0.,0.,1.));
#29657=DIRECTION('ref_axis',(1.,0.,0.));
#29658=DIRECTION('',(0.976699262102109,-0.214612561163589,0.));
#29659=DIRECTION('center_axis',(0.214612561163589,0.976699262102109,0.));
#29660=DIRECTION('ref_axis',(0.976699262102109,-0.214612561163589,0.));
#29661=DIRECTION('',(0.,0.,-1.));
#29662=DIRECTION('',(0.976699262102109,-0.214612561163589,0.));
#29663=DIRECTION('center_axis',(0.,0.,-1.));
#29664=DIRECTION('ref_axis',(-1.,0.,0.));
#29665=DIRECTION('center_axis',(0.,0.,-1.));
#29666=DIRECTION('ref_axis',(1.,0.,0.));
#29667=DIRECTION('center_axis',(-0.99912808582995,-0.0417500671350421,0.));
#29668=DIRECTION('ref_axis',(-0.0417500671350421,0.99912808582995,0.));
#29669=DIRECTION('',(0.,0.,1.));
#29670=DIRECTION('',(-0.0417500671350421,0.99912808582995,0.));
#29671=DIRECTION('',(0.,0.,-1.));
#29672=DIRECTION('',(-0.0417500671350421,0.99912808582995,0.));
#29673=DIRECTION('center_axis',(0.,0.,1.));
#29674=DIRECTION('ref_axis',(1.,0.,0.));
#29675=DIRECTION('center_axis',(0.,0.,1.));
#29676=DIRECTION('ref_axis',(1.,0.,0.));
#29677=DIRECTION('',(0.84439527039573,-0.535720661663634,0.));
#29678=DIRECTION('center_axis',(0.535720661663634,0.84439527039573,0.));
#29679=DIRECTION('ref_axis',(0.84439527039573,-0.535720661663634,0.));
#29680=DIRECTION('',(0.,0.,-1.));
#29681=DIRECTION('',(0.84439527039573,-0.535720661663634,0.));
#29682=DIRECTION('center_axis',(0.,0.,-1.));
#29683=DIRECTION('ref_axis',(-1.,0.,0.));
#29684=DIRECTION('center_axis',(0.,0.,-1.));
#29685=DIRECTION('ref_axis',(1.,0.,0.));
#29686=DIRECTION('center_axis',(-0.953152653419739,0.302489701112138,0.));
#29687=DIRECTION('ref_axis',(0.302489701112138,0.953152653419739,0.));
#29688=DIRECTION('',(0.,0.,1.));
#29689=DIRECTION('',(0.302489701112138,0.953152653419739,0.));
#29690=DIRECTION('',(0.,0.,-1.));
#29691=DIRECTION('',(0.302489701112138,0.953152653419739,0.));
#29692=DIRECTION('center_axis',(0.,0.,1.));
#29693=DIRECTION('ref_axis',(1.,0.,0.));
#29694=DIRECTION('center_axis',(0.,0.,1.));
#29695=DIRECTION('ref_axis',(1.,0.,0.));
#29696=DIRECTION('',(0.610244747132677,-0.792212943972121,0.));
#29697=DIRECTION('center_axis',(0.792212943972121,0.610244747132677,0.));
#29698=DIRECTION('ref_axis',(0.610244747132677,-0.792212943972121,0.));
#29699=DIRECTION('',(0.,0.,-1.));
#29700=DIRECTION('',(0.610244747132677,-0.792212943972121,0.));
#29701=DIRECTION('center_axis',(0.,0.,-1.));
#29702=DIRECTION('ref_axis',(-1.,0.,0.));
#29703=DIRECTION('center_axis',(0.,0.,-1.));
#29704=DIRECTION('ref_axis',(1.,0.,0.));
#29705=DIRECTION('center_axis',(-0.792212943972121,0.610244747132677,0.));
#29706=DIRECTION('ref_axis',(0.610244747132677,0.792212943972121,0.));
#29707=DIRECTION('',(0.,0.,1.));
#29708=DIRECTION('',(0.610244747132677,0.792212943972121,0.));
#29709=DIRECTION('',(0.,0.,-1.));
#29710=DIRECTION('',(0.610244747132677,0.792212943972121,0.));
#29711=DIRECTION('center_axis',(0.,0.,1.));
#29712=DIRECTION('ref_axis',(1.,0.,0.));
#29713=DIRECTION('center_axis',(0.,0.,1.));
#29714=DIRECTION('ref_axis',(1.,0.,0.));
#29715=DIRECTION('',(0.302489701112144,-0.953152653419737,0.));
#29716=DIRECTION('center_axis',(0.953152653419737,0.302489701112144,0.));
#29717=DIRECTION('ref_axis',(0.302489701112144,-0.953152653419737,0.));
#29718=DIRECTION('',(0.,0.,-1.));
#29719=DIRECTION('',(0.302489701112144,-0.953152653419737,0.));
#29720=DIRECTION('center_axis',(0.,0.,-1.));
#29721=DIRECTION('ref_axis',(-1.,0.,0.));
#29722=DIRECTION('center_axis',(0.,0.,-1.));
#29723=DIRECTION('ref_axis',(1.,0.,0.));
#29724=DIRECTION('center_axis',(-0.535720661663633,0.844395270395731,0.));
#29725=DIRECTION('ref_axis',(0.844395270395731,0.535720661663633,0.));
#29726=DIRECTION('',(0.,0.,1.));
#29727=DIRECTION('',(0.844395270395731,0.535720661663633,0.));
#29728=DIRECTION('',(0.,0.,-1.));
#29729=DIRECTION('',(0.844395270395731,0.535720661663633,0.));
#29730=DIRECTION('center_axis',(0.,0.,1.));
#29731=DIRECTION('ref_axis',(1.,0.,0.));
#29732=DIRECTION('center_axis',(0.,0.,1.));
#29733=DIRECTION('ref_axis',(1.,0.,0.));
#29734=DIRECTION('',(-0.0417500671350428,-0.99912808582995,0.));
#29735=DIRECTION('center_axis',(0.99912808582995,-0.0417500671350428,0.));
#29736=DIRECTION('ref_axis',(-0.0417500671350428,-0.99912808582995,0.));
#29737=DIRECTION('',(0.,0.,-1.));
#29738=DIRECTION('',(-0.0417500671350428,-0.99912808582995,0.));
#29739=DIRECTION('center_axis',(0.,0.,-1.));
#29740=DIRECTION('ref_axis',(-1.,0.,0.));
#29741=DIRECTION('center_axis',(0.,0.,-1.));
#29742=DIRECTION('ref_axis',(1.,0.,0.));
#29743=DIRECTION('center_axis',(-0.214612561163593,0.976699262102108,0.));
#29744=DIRECTION('ref_axis',(0.976699262102108,0.214612561163593,0.));
#29745=DIRECTION('',(0.,0.,1.));
#29746=DIRECTION('',(0.976699262102108,0.214612561163593,0.));
#29747=DIRECTION('',(0.,0.,-1.));
#29748=DIRECTION('',(0.976699262102108,0.214612561163593,0.));
#29749=DIRECTION('center_axis',(0.,0.,1.));
#29750=DIRECTION('ref_axis',(1.,0.,0.));
#29751=DIRECTION('center_axis',(0.,0.,1.));
#29752=DIRECTION('ref_axis',(1.,0.,0.));
#29753=DIRECTION('',(-0.38095416112038,-0.924593925528968,0.));
#29754=DIRECTION('center_axis',(0.924593925528968,-0.38095416112038,0.));
#29755=DIRECTION('ref_axis',(-0.38095416112038,-0.924593925528968,0.));
#29756=DIRECTION('',(0.,0.,-1.));
#29757=DIRECTION('',(-0.38095416112038,-0.924593925528968,0.));
#29758=DIRECTION('center_axis',(0.,0.,-1.));
#29759=DIRECTION('ref_axis',(-1.,0.,0.));
#29760=DIRECTION('center_axis',(0.,0.,-1.));
#29761=DIRECTION('ref_axis',(1.,0.,0.));
#29762=DIRECTION('center_axis',(0.132380981556845,0.991198908253054,0.));
#29763=DIRECTION('ref_axis',(0.991198908253054,-0.132380981556845,0.));
#29764=DIRECTION('',(0.,0.,1.));
#29765=DIRECTION('',(0.991198908253054,-0.132380981556845,0.));
#29766=DIRECTION('',(0.,0.,-1.));
#29767=DIRECTION('',(0.991198908253054,-0.132380981556845,0.));
#29768=DIRECTION('center_axis',(0.,0.,1.));
#29769=DIRECTION('ref_axis',(1.,0.,0.));
#29770=DIRECTION('center_axis',(0.,0.,1.));
#29771=DIRECTION('ref_axis',(1.,0.,0.));
#29772=DIRECTION('',(-0.674209560989967,-0.738540092256145,0.));
#29773=DIRECTION('center_axis',(0.738540092256145,-0.674209560989967,0.));
#29774=DIRECTION('ref_axis',(-0.674209560989967,-0.738540092256145,0.));
#29775=DIRECTION('',(0.,0.,-1.));
#29776=DIRECTION('',(-0.674209560989967,-0.738540092256145,0.));
#29777=DIRECTION('center_axis',(0.,0.,-1.));
#29778=DIRECTION('ref_axis',(-1.,0.,0.));
#29779=DIRECTION('center_axis',(0.,0.,-1.));
#29780=DIRECTION('ref_axis',(1.,0.,0.));
#29781=DIRECTION('center_axis',(0.463407424166319,0.886145337530779,0.));
#29782=DIRECTION('ref_axis',(0.886145337530779,-0.463407424166319,0.));
#29783=DIRECTION('',(0.,0.,1.));
#29784=DIRECTION('',(0.886145337530779,-0.463407424166319,0.));
#29785=DIRECTION('',(0.,0.,-1.));
#29786=DIRECTION('',(0.886145337530779,-0.463407424166319,0.));
#29787=DIRECTION('center_axis',(0.,0.,1.));
#29788=DIRECTION('ref_axis',(1.,0.,0.));
#29789=DIRECTION('center_axis',(0.,0.,1.));
#29790=DIRECTION('ref_axis',(1.,0.,0.));
#29791=DIRECTION('',(-0.886145337530779,-0.463407424166319,0.));
#29792=DIRECTION('center_axis',(0.,0.,1.));
#29793=DIRECTION('ref_axis',(1.,0.,0.));
#29794=DIRECTION('center_axis',(0.463407424166319,-0.886145337530779,0.));
#29795=DIRECTION('ref_axis',(-0.886145337530779,-0.463407424166319,0.));
#29796=DIRECTION('',(0.,0.,-1.));
#29797=DIRECTION('',(-0.886145337530779,-0.463407424166319,0.));
#29798=DIRECTION('center_axis',(0.,0.,-1.));
#29799=DIRECTION('ref_axis',(-1.,0.,0.));
#29800=DIRECTION('center_axis',(0.,0.,-1.));
#29801=DIRECTION('ref_axis',(1.,0.,0.));
#29802=DIRECTION('center_axis',(0.,0.,-1.));
#29803=DIRECTION('ref_axis',(1.,0.,0.));
#29804=DIRECTION('center_axis',(0.610244747132677,0.792212943972121,0.));
#29805=DIRECTION('ref_axis',(0.792212943972121,-0.610244747132677,0.));
#29806=DIRECTION('',(0.,0.,1.));
#29807=DIRECTION('',(0.792212943972121,-0.610244747132677,0.));
#29808=DIRECTION('',(0.,0.,-1.));
#29809=DIRECTION('',(0.792212943972121,-0.610244747132677,0.));
#29810=DIRECTION('center_axis',(0.,0.,1.));
#29811=DIRECTION('ref_axis',(1.,0.,0.));
#29812=DIRECTION('center_axis',(0.,0.,1.));
#29813=DIRECTION('ref_axis',(1.,0.,0.));
#29814=DIRECTION('',(-0.953152653419738,-0.302489701112141,0.));
#29815=DIRECTION('center_axis',(0.302489701112141,-0.953152653419738,0.));
#29816=DIRECTION('ref_axis',(-0.953152653419738,-0.302489701112141,0.));
#29817=DIRECTION('',(0.,0.,-1.));
#29818=DIRECTION('',(-0.953152653419738,-0.302489701112141,0.));
#29819=DIRECTION('center_axis',(0.,0.,-1.));
#29820=DIRECTION('ref_axis',(-1.,0.,0.));
#29821=DIRECTION('center_axis',(0.,0.,-1.));
#29822=DIRECTION('ref_axis',(1.,0.,0.));
#29823=DIRECTION('center_axis',(0.844395270395734,0.535720661663628,0.));
#29824=DIRECTION('ref_axis',(0.535720661663628,-0.844395270395734,0.));
#29825=DIRECTION('',(0.,0.,1.));
#29826=DIRECTION('',(0.535720661663628,-0.844395270395734,0.));
#29827=DIRECTION('',(0.,0.,-1.));
#29828=DIRECTION('',(0.535720661663628,-0.844395270395734,0.));
#29829=DIRECTION('center_axis',(0.,0.,1.));
#29830=DIRECTION('ref_axis',(1.,0.,0.));
#29831=DIRECTION('center_axis',(0.,0.,1.));
#29832=DIRECTION('ref_axis',(1.,0.,0.));
#29833=DIRECTION('',(-0.99912808582995,0.0417500671350472,0.));
#29834=DIRECTION('center_axis',(-0.0417500671350472,-0.99912808582995,0.));
#29835=DIRECTION('ref_axis',(-0.99912808582995,0.0417500671350472,0.));
#29836=DIRECTION('',(0.,0.,-1.));
#29837=DIRECTION('',(-0.99912808582995,0.0417500671350472,0.));
#29838=DIRECTION('center_axis',(0.,0.,-1.));
#29839=DIRECTION('ref_axis',(-1.,0.,0.));
#29840=DIRECTION('center_axis',(0.,0.,-1.));
#29841=DIRECTION('ref_axis',(1.,0.,0.));
#29842=DIRECTION('center_axis',(0.976699262102109,0.214612561163593,0.));
#29843=DIRECTION('ref_axis',(0.214612561163593,-0.976699262102109,0.));
#29844=DIRECTION('',(0.,0.,1.));
#29845=DIRECTION('',(0.214612561163593,-0.976699262102109,0.));
#29846=DIRECTION('',(0.,0.,-1.));
#29847=DIRECTION('',(0.214612561163593,-0.976699262102109,0.));
#29848=DIRECTION('center_axis',(0.,0.,1.));
#29849=DIRECTION('ref_axis',(1.,0.,0.));
#29850=DIRECTION('center_axis',(0.,0.,1.));
#29851=DIRECTION('ref_axis',(1.,0.,0.));
#29852=DIRECTION('',(-0.924593925528968,0.38095416112038,0.));
#29853=DIRECTION('center_axis',(-0.38095416112038,-0.924593925528968,0.));
#29854=DIRECTION('ref_axis',(-0.924593925528968,0.38095416112038,0.));
#29855=DIRECTION('',(0.,0.,-1.));
#29856=DIRECTION('',(-0.924593925528968,0.38095416112038,0.));
#29857=DIRECTION('center_axis',(0.,0.,-1.));
#29858=DIRECTION('ref_axis',(-1.,0.,0.));
#29859=DIRECTION('center_axis',(0.,0.,-1.));
#29860=DIRECTION('ref_axis',(1.,0.,0.));
#29861=DIRECTION('center_axis',(0.991198908253054,-0.132380981556846,0.));
#29862=DIRECTION('ref_axis',(-0.132380981556846,-0.991198908253054,0.));
#29863=DIRECTION('',(0.,0.,1.));
#29864=DIRECTION('',(-0.132380981556846,-0.991198908253054,0.));
#29865=DIRECTION('',(0.,0.,-1.));
#29866=DIRECTION('',(-0.132380981556846,-0.991198908253054,0.));
#29867=DIRECTION('center_axis',(0.,0.,1.));
#29868=DIRECTION('ref_axis',(1.,0.,0.));
#29869=DIRECTION('center_axis',(0.,0.,1.));
#29870=DIRECTION('ref_axis',(1.,0.,0.));
#29871=DIRECTION('',(-0.738540092256146,0.674209560989966,0.));
#29872=DIRECTION('center_axis',(-0.674209560989966,-0.738540092256146,0.));
#29873=DIRECTION('ref_axis',(-0.738540092256146,0.674209560989966,0.));
#29874=DIRECTION('',(0.,0.,-1.));
#29875=DIRECTION('',(-0.738540092256146,0.674209560989966,0.));
#29876=DIRECTION('center_axis',(0.,0.,-1.));
#29877=DIRECTION('ref_axis',(-1.,0.,0.));
#29878=DIRECTION('center_axis',(0.,0.,-1.));
#29879=DIRECTION('ref_axis',(1.,0.,0.));
#29880=DIRECTION('center_axis',(0.886145337530778,-0.46340742416632,0.));
#29881=DIRECTION('ref_axis',(-0.46340742416632,-0.886145337530778,0.));
#29882=DIRECTION('',(0.,0.,1.));
#29883=DIRECTION('',(-0.46340742416632,-0.886145337530778,0.));
#29884=DIRECTION('',(0.,0.,-1.));
#29885=DIRECTION('',(-0.46340742416632,-0.886145337530778,0.));
#29886=DIRECTION('center_axis',(0.,0.,1.));
#29887=DIRECTION('ref_axis',(1.,0.,0.));
#29888=DIRECTION('center_axis',(0.,0.,1.));
#29889=DIRECTION('ref_axis',(1.,0.,0.));
#29890=DIRECTION('',(-0.46340742416632,0.886145337530778,0.));
#29891=DIRECTION('center_axis',(-0.886145337530778,-0.46340742416632,0.));
#29892=DIRECTION('ref_axis',(-0.46340742416632,0.886145337530778,0.));
#29893=DIRECTION('',(0.,0.,-1.));
#29894=DIRECTION('',(-0.46340742416632,0.886145337530778,0.));
#29895=DIRECTION('center_axis',(0.,0.,-1.));
#29896=DIRECTION('ref_axis',(-1.,0.,0.));
#29897=DIRECTION('center_axis',(0.,0.,-1.));
#29898=DIRECTION('ref_axis',(1.,0.,0.));
#29899=DIRECTION('center_axis',(0.674209560989967,-0.738540092256145,0.));
#29900=DIRECTION('ref_axis',(-0.738540092256145,-0.674209560989967,0.));
#29901=DIRECTION('',(0.,0.,1.));
#29902=DIRECTION('',(-0.738540092256145,-0.674209560989967,0.));
#29903=DIRECTION('',(0.,0.,-1.));
#29904=DIRECTION('',(-0.738540092256145,-0.674209560989967,0.));
#29905=DIRECTION('center_axis',(0.,0.,1.));
#29906=DIRECTION('ref_axis',(1.,0.,0.));
#29907=DIRECTION('center_axis',(0.,0.,1.));
#29908=DIRECTION('ref_axis',(1.,0.,0.));
#29909=DIRECTION('',(-0.132380981556847,0.991198908253054,0.));
#29910=DIRECTION('center_axis',(-0.991198908253054,-0.132380981556847,0.));
#29911=DIRECTION('ref_axis',(-0.132380981556847,0.991198908253054,0.));
#29912=DIRECTION('',(0.,0.,-1.));
#29913=DIRECTION('',(-0.132380981556847,0.991198908253054,0.));
#29914=DIRECTION('center_axis',(0.,0.,-1.));
#29915=DIRECTION('ref_axis',(-1.,0.,0.));
#29916=DIRECTION('center_axis',(0.,0.,-1.));
#29917=DIRECTION('ref_axis',(1.,0.,0.));
#29918=DIRECTION('center_axis',(0.380954161120379,-0.924593925528969,0.));
#29919=DIRECTION('ref_axis',(-0.924593925528969,-0.380954161120379,0.));
#29920=DIRECTION('',(0.,0.,1.));
#29921=DIRECTION('',(-0.924593925528969,-0.380954161120379,0.));
#29922=DIRECTION('',(0.,0.,-1.));
#29923=DIRECTION('',(-0.924593925528969,-0.380954161120379,0.));
#29924=DIRECTION('center_axis',(0.,0.,1.));
#29925=DIRECTION('ref_axis',(1.,0.,0.));
#29926=DIRECTION('center_axis',(0.,0.,1.));
#29927=DIRECTION('ref_axis',(1.,0.,0.));
#29928=DIRECTION('',(0.214612561163592,0.976699262102109,0.));
#29929=DIRECTION('center_axis',(-0.976699262102109,0.214612561163592,0.));
#29930=DIRECTION('ref_axis',(0.214612561163592,0.976699262102109,0.));
#29931=DIRECTION('',(0.,0.,-1.));
#29932=DIRECTION('',(0.214612561163592,0.976699262102109,0.));
#29933=DIRECTION('center_axis',(0.,0.,-1.));
#29934=DIRECTION('ref_axis',(-1.,0.,0.));
#29935=DIRECTION('center_axis',(0.,0.,-1.));
#29936=DIRECTION('ref_axis',(1.,0.,0.));
#29937=DIRECTION('center_axis',(0.0417500671350458,-0.99912808582995,0.));
#29938=DIRECTION('ref_axis',(-0.99912808582995,-0.0417500671350458,0.));
#29939=DIRECTION('',(0.,0.,1.));
#29940=DIRECTION('',(-0.99912808582995,-0.0417500671350458,0.));
#29941=DIRECTION('',(0.,0.,-1.));
#29942=DIRECTION('',(-0.99912808582995,-0.0417500671350458,0.));
#29943=DIRECTION('center_axis',(0.,0.,1.));
#29944=DIRECTION('ref_axis',(1.,0.,0.));
#29945=DIRECTION('center_axis',(0.,0.,1.));
#29946=DIRECTION('ref_axis',(1.,0.,0.));
#29947=DIRECTION('',(0.535720661663629,0.844395270395733,0.));
#29948=DIRECTION('center_axis',(-0.844395270395733,0.535720661663629,0.));
#29949=DIRECTION('ref_axis',(0.535720661663629,0.844395270395733,0.));
#29950=DIRECTION('',(0.,0.,-1.));
#29951=DIRECTION('',(0.535720661663629,0.844395270395733,0.));
#29952=DIRECTION('center_axis',(0.,0.,-1.));
#29953=DIRECTION('ref_axis',(-1.,0.,0.));
#29954=DIRECTION('center_axis',(0.,0.,-1.));
#29955=DIRECTION('ref_axis',(1.,0.,0.));
#29956=DIRECTION('center_axis',(-0.302489701112142,-0.953152653419738,0.));
#29957=DIRECTION('ref_axis',(-0.953152653419738,0.302489701112142,0.));
#29958=DIRECTION('',(0.,0.,1.));
#29959=DIRECTION('',(-0.953152653419738,0.302489701112142,0.));
#29960=DIRECTION('',(0.,0.,-1.));
#29961=DIRECTION('',(-0.953152653419738,0.302489701112142,0.));
#29962=DIRECTION('center_axis',(0.,0.,1.));
#29963=DIRECTION('ref_axis',(1.,0.,0.));
#29964=DIRECTION('center_axis',(0.,0.,1.));
#29965=DIRECTION('ref_axis',(1.,0.,0.));
#29966=DIRECTION('',(0.792212943972123,0.610244747132675,0.));
#29967=DIRECTION('center_axis',(-0.610244747132675,0.792212943972123,0.));
#29968=DIRECTION('ref_axis',(0.792212943972123,0.610244747132675,0.));
#29969=DIRECTION('',(0.,0.,-1.));
#29970=DIRECTION('',(0.792212943972123,0.610244747132675,0.));
#29971=DIRECTION('center_axis',(0.,0.,-1.));
#29972=DIRECTION('ref_axis',(-1.,0.,0.));
#29973=DIRECTION('center_axis',(0.,0.,-1.));
#29974=DIRECTION('ref_axis',(1.,0.,0.));
#29975=DIRECTION('center_axis',(-0.132380981556845,-0.991198908253054,0.));
#29976=DIRECTION('ref_axis',(-0.991198908253054,0.132380981556845,0.));
#29977=DIRECTION('',(0.,0.,1.));
#29978=DIRECTION('',(-0.991198908253054,0.132380981556845,0.));
#29979=DIRECTION('',(0.,0.,-1.));
#29980=DIRECTION('',(-0.991198908253054,0.132380981556845,0.));
#29981=DIRECTION('center_axis',(0.,0.,1.));
#29982=DIRECTION('ref_axis',(1.,0.,0.));
#29983=DIRECTION('center_axis',(0.,0.,1.));
#29984=DIRECTION('ref_axis',(1.,0.,0.));
#29985=DIRECTION('',(0.674209560989966,0.738540092256146,0.));
#29986=DIRECTION('center_axis',(-0.738540092256146,0.674209560989966,0.));
#29987=DIRECTION('ref_axis',(0.674209560989966,0.738540092256146,0.));
#29988=DIRECTION('',(0.,0.,-1.));
#29989=DIRECTION('',(0.674209560989966,0.738540092256146,0.));
#29990=DIRECTION('center_axis',(0.,0.,-1.));
#29991=DIRECTION('ref_axis',(-1.,0.,0.));
#29992=DIRECTION('center_axis',(0.,0.,-1.));
#29993=DIRECTION('ref_axis',(1.,0.,0.));
#29994=DIRECTION('center_axis',(0.214612561163592,-0.976699262102109,0.));
#29995=DIRECTION('ref_axis',(-0.976699262102109,-0.214612561163592,0.));
#29996=DIRECTION('',(0.,0.,1.));
#29997=DIRECTION('',(-0.976699262102109,-0.214612561163592,0.));
#29998=DIRECTION('',(0.,0.,-1.));
#29999=DIRECTION('',(-0.976699262102109,-0.214612561163592,0.));
#30000=DIRECTION('center_axis',(0.,0.,1.));
#30001=DIRECTION('ref_axis',(1.,0.,0.));
#30002=DIRECTION('center_axis',(0.,0.,1.));
#30003=DIRECTION('ref_axis',(1.,0.,0.));
#30004=DIRECTION('',(0.380954161120378,0.924593925528969,0.));
#30005=DIRECTION('center_axis',(-0.924593925528969,0.380954161120378,0.));
#30006=DIRECTION('ref_axis',(0.380954161120378,0.924593925528969,0.));
#30007=DIRECTION('',(0.,0.,-1.));
#30008=DIRECTION('',(0.380954161120378,0.924593925528969,0.));
#30009=DIRECTION('center_axis',(0.,0.,-1.));
#30010=DIRECTION('ref_axis',(-1.,0.,0.));
#30011=DIRECTION('center_axis',(0.,0.,-1.));
#30012=DIRECTION('ref_axis',(1.,0.,0.));
#30013=DIRECTION('center_axis',(0.53572066166363,-0.844395270395733,0.));
#30014=DIRECTION('ref_axis',(-0.844395270395733,-0.53572066166363,0.));
#30015=DIRECTION('',(0.,0.,1.));
#30016=DIRECTION('',(-0.844395270395733,-0.53572066166363,0.));
#30017=DIRECTION('',(0.,0.,-1.));
#30018=DIRECTION('',(-0.844395270395733,-0.53572066166363,0.));
#30019=DIRECTION('center_axis',(0.,0.,1.));
#30020=DIRECTION('ref_axis',(1.,0.,0.));
#30021=DIRECTION('center_axis',(0.,0.,1.));
#30022=DIRECTION('ref_axis',(1.,0.,0.));
#30023=DIRECTION('',(0.0417500671350451,0.99912808582995,0.));
#30024=DIRECTION('center_axis',(-0.99912808582995,0.0417500671350451,0.));
#30025=DIRECTION('ref_axis',(0.0417500671350451,0.99912808582995,0.));
#30026=DIRECTION('',(0.,0.,-1.));
#30027=DIRECTION('',(0.0417500671350451,0.99912808582995,0.));
#30028=DIRECTION('center_axis',(0.,0.,-1.));
#30029=DIRECTION('ref_axis',(-1.,0.,0.));
#30030=DIRECTION('center_axis',(0.,0.,-1.));
#30031=DIRECTION('ref_axis',(1.,0.,0.));
#30032=DIRECTION('center_axis',(0.792212943972124,-0.610244747132674,0.));
#30033=DIRECTION('ref_axis',(-0.610244747132674,-0.792212943972124,0.));
#30034=DIRECTION('',(0.,0.,1.));
#30035=DIRECTION('',(-0.610244747132674,-0.792212943972124,0.));
#30036=DIRECTION('',(0.,0.,-1.));
#30037=DIRECTION('',(-0.610244747132674,-0.792212943972124,0.));
#30038=DIRECTION('center_axis',(0.,0.,1.));
#30039=DIRECTION('ref_axis',(1.,0.,0.));
#30040=DIRECTION('center_axis',(0.,0.,1.));
#30041=DIRECTION('ref_axis',(1.,0.,0.));
#30042=DIRECTION('',(-0.302489701112143,0.953152653419738,0.));
#30043=DIRECTION('center_axis',(-0.953152653419738,-0.302489701112143,0.));
#30044=DIRECTION('ref_axis',(-0.302489701112143,0.953152653419738,0.));
#30045=DIRECTION('',(0.,0.,-1.));
#30046=DIRECTION('',(-0.302489701112143,0.953152653419738,0.));
#30047=DIRECTION('center_axis',(0.,0.,-1.));
#30048=DIRECTION('ref_axis',(-1.,0.,0.));
#30049=DIRECTION('center_axis',(0.,0.,-1.));
#30050=DIRECTION('ref_axis',(1.,0.,0.));
#30051=DIRECTION('center_axis',(0.953152653419738,-0.302489701112143,0.));
#30052=DIRECTION('ref_axis',(-0.302489701112143,-0.953152653419738,0.));
#30053=DIRECTION('',(0.,0.,1.));
#30054=DIRECTION('',(-0.302489701112143,-0.953152653419738,0.));
#30055=DIRECTION('',(0.,0.,-1.));
#30056=DIRECTION('',(-0.302489701112143,-0.953152653419738,0.));
#30057=DIRECTION('center_axis',(0.,0.,1.));
#30058=DIRECTION('ref_axis',(1.,0.,0.));
#30059=DIRECTION('center_axis',(0.,0.,1.));
#30060=DIRECTION('ref_axis',(1.,0.,0.));
#30061=DIRECTION('',(-0.610244747132675,0.792212943972123,0.));
#30062=DIRECTION('center_axis',(-0.792212943972123,-0.610244747132675,0.));
#30063=DIRECTION('ref_axis',(-0.610244747132675,0.792212943972123,0.));
#30064=DIRECTION('',(0.,0.,-1.));
#30065=DIRECTION('',(-0.610244747132675,0.792212943972123,0.));
#30066=DIRECTION('center_axis',(0.,0.,-1.));
#30067=DIRECTION('ref_axis',(-1.,0.,0.));
#30068=DIRECTION('center_axis',(0.,0.,-1.));
#30069=DIRECTION('ref_axis',(1.,0.,0.));
#30070=DIRECTION('center_axis',(0.99912808582995,0.0417500671350458,0.));
#30071=DIRECTION('ref_axis',(0.0417500671350458,-0.99912808582995,0.));
#30072=DIRECTION('',(0.,0.,1.));
#30073=DIRECTION('',(0.0417500671350458,-0.99912808582995,0.));
#30074=DIRECTION('',(0.,0.,-1.));
#30075=DIRECTION('',(0.0417500671350458,-0.99912808582995,0.));
#30076=DIRECTION('center_axis',(0.,0.,1.));
#30077=DIRECTION('ref_axis',(1.,0.,0.));
#30078=DIRECTION('center_axis',(0.,0.,1.));
#30079=DIRECTION('ref_axis',(1.,0.,0.));
#30080=DIRECTION('',(-0.844395270395734,0.535720661663629,0.));
#30081=DIRECTION('center_axis',(-0.535720661663629,-0.844395270395734,0.));
#30082=DIRECTION('ref_axis',(-0.844395270395734,0.535720661663629,0.));
#30083=DIRECTION('',(0.,0.,-1.));
#30084=DIRECTION('',(-0.844395270395734,0.535720661663629,0.));
#30085=DIRECTION('center_axis',(0.,0.,-1.));
#30086=DIRECTION('ref_axis',(-1.,0.,0.));
#30087=DIRECTION('center_axis',(0.,0.,-1.));
#30088=DIRECTION('ref_axis',(1.,0.,0.));
#30089=DIRECTION('center_axis',(0.924593925528969,0.380954161120379,0.));
#30090=DIRECTION('ref_axis',(0.380954161120379,-0.924593925528969,0.));
#30091=DIRECTION('',(0.,0.,1.));
#30092=DIRECTION('',(0.380954161120379,-0.924593925528969,0.));
#30093=DIRECTION('',(0.,0.,-1.));
#30094=DIRECTION('',(0.380954161120379,-0.924593925528969,0.));
#30095=DIRECTION('center_axis',(0.,0.,1.));
#30096=DIRECTION('ref_axis',(1.,0.,0.));
#30097=DIRECTION('center_axis',(0.,0.,1.));
#30098=DIRECTION('ref_axis',(1.,0.,0.));
#30099=DIRECTION('',(-0.976699262102109,0.214612561163589,0.));
#30100=DIRECTION('center_axis',(-0.214612561163589,-0.976699262102109,0.));
#30101=DIRECTION('ref_axis',(-0.976699262102109,0.214612561163589,0.));
#30102=DIRECTION('',(0.,0.,-1.));
#30103=DIRECTION('',(-0.976699262102109,0.214612561163589,0.));
#30104=DIRECTION('center_axis',(0.,0.,-1.));
#30105=DIRECTION('ref_axis',(-1.,0.,0.));
#30106=DIRECTION('center_axis',(0.,0.,-1.));
#30107=DIRECTION('ref_axis',(1.,0.,0.));
#30108=DIRECTION('center_axis',(0.738540092256146,0.674209560989967,0.));
#30109=DIRECTION('ref_axis',(0.674209560989967,-0.738540092256146,0.));
#30110=DIRECTION('',(0.,0.,1.));
#30111=DIRECTION('',(0.674209560989967,-0.738540092256146,0.));
#30112=DIRECTION('',(0.,0.,-1.));
#30113=DIRECTION('',(0.674209560989967,-0.738540092256146,0.));
#30114=DIRECTION('center_axis',(0.,0.,1.));
#30115=DIRECTION('ref_axis',(1.,0.,0.));
#30116=DIRECTION('center_axis',(0.,0.,1.));
#30117=DIRECTION('ref_axis',(1.,0.,0.));
#30118=DIRECTION('',(-0.991198908253054,-0.132380981556849,0.));
#30119=DIRECTION('center_axis',(0.132380981556849,-0.991198908253054,0.));
#30120=DIRECTION('ref_axis',(-0.991198908253054,-0.132380981556849,0.));
#30121=DIRECTION('',(0.,0.,-1.));
#30122=DIRECTION('',(-0.991198908253054,-0.132380981556849,0.));
#30123=DIRECTION('center_axis',(0.,0.,-1.));
#30124=DIRECTION('ref_axis',(-1.,0.,0.));
#30125=DIRECTION('center_axis',(0.,0.,-1.));
#30126=DIRECTION('ref_axis',(1.,0.,0.));
#30127=DIRECTION('center_axis',(0.,0.,1.));
#30128=DIRECTION('ref_axis',(1.,0.,0.));
#30129=DIRECTION('center_axis',(0.,0.,1.));
#30130=DIRECTION('ref_axis',(1.,0.,0.));
#30131=DIRECTION('',(-0.886145337530778,0.46340742416632,0.));
#30132=DIRECTION('',(0.886145337530778,0.46340742416632,0.));
#30133=DIRECTION('center_axis',(-0.46340742416632,-0.886145337530778,0.));
#30134=DIRECTION('ref_axis',(-0.886145337530778,0.46340742416632,0.));
#30135=DIRECTION('',(0.,0.,1.));
#30136=DIRECTION('',(-0.886145337530778,0.46340742416632,0.));
#30137=DIRECTION('',(0.,0.,-1.));
#30138=DIRECTION('center_axis',(-0.46340742416632,0.886145337530778,0.));
#30139=DIRECTION('ref_axis',(0.886145337530778,0.46340742416632,0.));
#30140=DIRECTION('',(0.,0.,-1.));
#30141=DIRECTION('',(0.886145337530778,0.46340742416632,0.));
#30142=DIRECTION('center_axis',(0.,0.,-1.));
#30143=DIRECTION('ref_axis',(-1.,0.,0.));
#30144=DIRECTION('center_axis',(0.,0.,-1.));
#30145=DIRECTION('ref_axis',(1.,0.,0.));
#30146=DIRECTION('center_axis',(0.302489701112144,0.953152653419737,0.));
#30147=DIRECTION('ref_axis',(0.953152653419737,-0.302489701112144,0.));
#30148=DIRECTION('',(0.,0.,1.));
#30149=DIRECTION('',(0.953152653419737,-0.302489701112144,0.));
#30150=DIRECTION('',(0.,0.,-1.));
#30151=DIRECTION('',(0.953152653419737,-0.302489701112144,0.));
#30152=DIRECTION('center_axis',(0.,0.,1.));
#30153=DIRECTION('ref_axis',(1.,0.,0.));
#30154=DIRECTION('center_axis',(0.,0.,1.));
#30155=DIRECTION('ref_axis',(1.,0.,0.));
#30156=DIRECTION('',(-0.792212943972123,-0.610244747132674,0.));
#30157=DIRECTION('center_axis',(0.610244747132674,-0.792212943972123,0.));
#30158=DIRECTION('ref_axis',(-0.792212943972123,-0.610244747132674,0.));
#30159=DIRECTION('',(0.,0.,-1.));
#30160=DIRECTION('',(-0.792212943972123,-0.610244747132674,0.));
#30161=DIRECTION('center_axis',(0.,0.,-1.));
#30162=DIRECTION('ref_axis',(-1.,0.,0.));
#30163=DIRECTION('center_axis',(0.,0.,-1.));
#30164=DIRECTION('ref_axis',(1.,0.,0.));
#30165=DIRECTION('center_axis',(-0.0417500671350422,0.99912808582995,0.));
#30166=DIRECTION('ref_axis',(0.99912808582995,0.0417500671350422,0.));
#30167=DIRECTION('',(0.,0.,1.));
#30168=DIRECTION('',(0.99912808582995,0.0417500671350422,0.));
#30169=DIRECTION('',(0.,0.,-1.));
#30170=DIRECTION('',(0.99912808582995,0.0417500671350422,0.));
#30171=DIRECTION('center_axis',(0.,0.,1.));
#30172=DIRECTION('ref_axis',(1.,0.,0.));
#30173=DIRECTION('center_axis',(0.,0.,1.));
#30174=DIRECTION('ref_axis',(1.,0.,0.));
#30175=DIRECTION('',(-0.53572066166363,-0.844395270395733,0.));
#30176=DIRECTION('center_axis',(0.844395270395733,-0.53572066166363,0.));
#30177=DIRECTION('ref_axis',(-0.53572066166363,-0.844395270395733,0.));
#30178=DIRECTION('',(0.,0.,-1.));
#30179=DIRECTION('',(-0.53572066166363,-0.844395270395733,0.));
#30180=DIRECTION('center_axis',(0.,0.,-1.));
#30181=DIRECTION('ref_axis',(-1.,0.,0.));
#30182=DIRECTION('center_axis',(0.,0.,-1.));
#30183=DIRECTION('ref_axis',(1.,0.,0.));
#30184=DIRECTION('center_axis',(-0.380954161120378,0.924593925528969,0.));
#30185=DIRECTION('ref_axis',(0.924593925528969,0.380954161120378,0.));
#30186=DIRECTION('',(0.,0.,1.));
#30187=DIRECTION('',(0.924593925528969,0.380954161120378,0.));
#30188=DIRECTION('',(0.,0.,-1.));
#30189=DIRECTION('',(0.924593925528969,0.380954161120378,0.));
#30190=DIRECTION('center_axis',(0.,0.,1.));
#30191=DIRECTION('ref_axis',(1.,0.,0.));
#30192=DIRECTION('center_axis',(0.,0.,1.));
#30193=DIRECTION('ref_axis',(1.,0.,0.));
#30194=DIRECTION('',(-0.214612561163591,-0.976699262102109,0.));
#30195=DIRECTION('center_axis',(0.976699262102109,-0.214612561163591,0.));
#30196=DIRECTION('ref_axis',(-0.214612561163591,-0.976699262102109,0.));
#30197=DIRECTION('',(0.,0.,-1.));
#30198=DIRECTION('',(-0.214612561163591,-0.976699262102109,0.));
#30199=DIRECTION('center_axis',(0.,0.,-1.));
#30200=DIRECTION('ref_axis',(-1.,0.,0.));
#30201=DIRECTION('center_axis',(0.,0.,-1.));
#30202=DIRECTION('ref_axis',(1.,0.,0.));
#30203=DIRECTION('center_axis',(-0.674209560989966,0.738540092256147,0.));
#30204=DIRECTION('ref_axis',(0.738540092256147,0.674209560989966,0.));
#30205=DIRECTION('',(0.,0.,1.));
#30206=DIRECTION('',(0.738540092256147,0.674209560989966,0.));
#30207=DIRECTION('',(0.,0.,-1.));
#30208=DIRECTION('',(0.738540092256147,0.674209560989966,0.));
#30209=DIRECTION('center_axis',(0.,0.,1.));
#30210=DIRECTION('ref_axis',(1.,0.,0.));
#30211=DIRECTION('center_axis',(0.,0.,1.));
#30212=DIRECTION('ref_axis',(1.,0.,0.));
#30213=DIRECTION('',(0.132380981556841,-0.991198908253055,0.));
#30214=DIRECTION('center_axis',(0.991198908253055,0.132380981556841,0.));
#30215=DIRECTION('ref_axis',(0.132380981556841,-0.991198908253055,0.));
#30216=DIRECTION('',(0.,0.,-1.));
#30217=DIRECTION('',(0.132380981556841,-0.991198908253055,0.));
#30218=DIRECTION('center_axis',(0.,0.,-1.));
#30219=DIRECTION('ref_axis',(-1.,0.,0.));
#30220=DIRECTION('center_axis',(0.,0.,-1.));
#30221=DIRECTION('ref_axis',(1.,0.,0.));
#30222=DIRECTION('center_axis',(-0.886145337530777,0.463407424166322,0.));
#30223=DIRECTION('ref_axis',(0.463407424166322,0.886145337530777,0.));
#30224=DIRECTION('',(0.,0.,1.));
#30225=DIRECTION('',(0.463407424166322,0.886145337530777,0.));
#30226=DIRECTION('',(0.,0.,-1.));
#30227=DIRECTION('',(0.463407424166322,0.886145337530777,0.));
#30228=DIRECTION('center_axis',(0.,0.,1.));
#30229=DIRECTION('ref_axis',(1.,0.,0.));
#30230=DIRECTION('center_axis',(0.,0.,1.));
#30231=DIRECTION('ref_axis',(1.,0.,0.));
#30232=DIRECTION('',(0.463407424166322,-0.886145337530777,0.));
#30233=DIRECTION('center_axis',(0.886145337530777,0.463407424166322,0.));
#30234=DIRECTION('ref_axis',(0.463407424166322,-0.886145337530777,0.));
#30235=DIRECTION('',(0.,0.,-1.));
#30236=DIRECTION('',(0.463407424166322,-0.886145337530777,0.));
#30237=DIRECTION('center_axis',(0.,0.,-1.));
#30238=DIRECTION('ref_axis',(-1.,0.,0.));
#30239=DIRECTION('center_axis',(0.,0.,-1.));
#30240=DIRECTION('ref_axis',(1.,0.,0.));
#30241=DIRECTION('center_axis',(-0.991198908253054,0.132380981556848,0.));
#30242=DIRECTION('ref_axis',(0.132380981556848,0.991198908253054,0.));
#30243=DIRECTION('',(0.,0.,1.));
#30244=DIRECTION('',(0.132380981556848,0.991198908253054,0.));
#30245=DIRECTION('',(0.,0.,-1.));
#30246=DIRECTION('',(0.132380981556848,0.991198908253054,0.));
#30247=DIRECTION('center_axis',(0.,0.,1.));
#30248=DIRECTION('ref_axis',(1.,0.,0.));
#30249=DIRECTION('center_axis',(0.,0.,1.));
#30250=DIRECTION('ref_axis',(1.,0.,0.));
#30251=DIRECTION('',(0.738540092256143,-0.67420956098997,0.));
#30252=DIRECTION('center_axis',(0.67420956098997,0.738540092256143,0.));
#30253=DIRECTION('ref_axis',(0.738540092256143,-0.67420956098997,0.));
#30254=DIRECTION('',(0.,0.,-1.));
#30255=DIRECTION('',(0.738540092256143,-0.67420956098997,0.));
#30256=DIRECTION('center_axis',(0.,0.,-1.));
#30257=DIRECTION('ref_axis',(-1.,0.,0.));
#30258=DIRECTION('center_axis',(0.,0.,-1.));
#30259=DIRECTION('ref_axis',(1.,0.,0.));
#30260=DIRECTION('center_axis',(-0.976699262102109,-0.214612561163589,0.));
#30261=DIRECTION('ref_axis',(-0.214612561163589,0.976699262102109,0.));
#30262=DIRECTION('',(0.,0.,1.));
#30263=DIRECTION('',(-0.214612561163589,0.976699262102109,0.));
#30264=DIRECTION('',(0.,0.,-1.));
#30265=DIRECTION('',(-0.214612561163589,0.976699262102109,0.));
#30266=DIRECTION('center_axis',(0.,0.,1.));
#30267=DIRECTION('ref_axis',(1.,0.,0.));
#30268=DIRECTION('center_axis',(0.,0.,1.));
#30269=DIRECTION('ref_axis',(1.,0.,0.));
#30270=DIRECTION('',(0.92459392552897,-0.380954161120377,0.));
#30271=DIRECTION('center_axis',(0.380954161120377,0.92459392552897,0.));
#30272=DIRECTION('ref_axis',(0.92459392552897,-0.380954161120377,0.));
#30273=DIRECTION('',(0.,0.,-1.));
#30274=DIRECTION('',(0.92459392552897,-0.380954161120377,0.));
#30275=DIRECTION('center_axis',(0.,0.,-1.));
#30276=DIRECTION('ref_axis',(-1.,0.,0.));
#30277=DIRECTION('center_axis',(0.,0.,-1.));
#30278=DIRECTION('ref_axis',(1.,0.,0.));
#30279=DIRECTION('center_axis',(-0.844395270395731,-0.535720661663633,0.));
#30280=DIRECTION('ref_axis',(-0.535720661663633,0.844395270395731,0.));
#30281=DIRECTION('',(0.,0.,1.));
#30282=DIRECTION('',(-0.535720661663633,0.844395270395731,0.));
#30283=DIRECTION('',(0.,0.,-1.));
#30284=DIRECTION('',(-0.535720661663633,0.844395270395731,0.));
#30285=DIRECTION('center_axis',(0.,0.,1.));
#30286=DIRECTION('ref_axis',(1.,0.,0.));
#30287=DIRECTION('center_axis',(0.,0.,1.));
#30288=DIRECTION('ref_axis',(1.,0.,0.));
#30289=DIRECTION('',(0.99912808582995,-0.0417500671350428,0.));
#30290=DIRECTION('center_axis',(0.0417500671350428,0.99912808582995,0.));
#30291=DIRECTION('ref_axis',(0.99912808582995,-0.0417500671350428,0.));
#30292=DIRECTION('',(0.,0.,-1.));
#30293=DIRECTION('',(0.99912808582995,-0.0417500671350428,0.));
#30294=DIRECTION('center_axis',(0.,0.,-1.));
#30295=DIRECTION('ref_axis',(-1.,0.,0.));
#30296=DIRECTION('center_axis',(0.,0.,-1.));
#30297=DIRECTION('ref_axis',(1.,0.,0.));
#30298=DIRECTION('center_axis',(-0.610244747132677,-0.792212943972121,0.));
#30299=DIRECTION('ref_axis',(-0.792212943972121,0.610244747132677,0.));
#30300=DIRECTION('',(0.,0.,1.));
#30301=DIRECTION('',(-0.792212943972121,0.610244747132677,0.));
#30302=DIRECTION('',(0.,0.,-1.));
#30303=DIRECTION('',(-0.792212943972121,0.610244747132677,0.));
#30304=DIRECTION('center_axis',(0.,0.,1.));
#30305=DIRECTION('ref_axis',(1.,0.,0.));
#30306=DIRECTION('center_axis',(0.,0.,1.));
#30307=DIRECTION('ref_axis',(1.,0.,0.));
#30308=DIRECTION('',(0.953152653419737,0.302489701112144,0.));
#30309=DIRECTION('center_axis',(-0.302489701112144,0.953152653419737,0.));
#30310=DIRECTION('ref_axis',(0.953152653419737,0.302489701112144,0.));
#30311=DIRECTION('',(0.,0.,-1.));
#30312=DIRECTION('',(0.953152653419737,0.302489701112144,0.));
#30313=DIRECTION('center_axis',(0.,0.,-1.));
#30314=DIRECTION('ref_axis',(-1.,0.,0.));
#30315=DIRECTION('center_axis',(0.,0.,-1.));
#30316=DIRECTION('ref_axis',(1.,0.,0.));
#30317=DIRECTION('center_axis',(0.,0.,-1.));
#30318=DIRECTION('ref_axis',(-1.,0.,0.));
#30319=DIRECTION('center_axis',(0.,0.,1.));
#30320=DIRECTION('ref_axis',(1.,0.,0.));
#30321=DIRECTION('center_axis',(0.,0.,1.));
#30322=DIRECTION('ref_axis',(1.,0.,0.));
#30323=DIRECTION('',(0.707106781186545,8.6595605623549E-17,-0.70710678118655));
#30324=DIRECTION('center_axis',(0.,0.,1.));
#30325=DIRECTION('ref_axis',(1.,0.,0.));
#30326=DIRECTION('center_axis',(0.,0.,1.));
#30327=DIRECTION('ref_axis',(1.,0.,0.));
#30328=DIRECTION('',(0.707106781186548,8.65956056235494E-17,-0.707106781186547));
#30329=DIRECTION('center_axis',(0.,0.,1.));
#30330=DIRECTION('ref_axis',(1.,0.,0.));
#30331=DIRECTION('center_axis',(0.,0.,1.));
#30332=DIRECTION('ref_axis',(1.,0.,0.));
#30333=DIRECTION('center_axis',(0.,0.,1.));
#30334=DIRECTION('ref_axis',(1.,0.,0.));
#30335=DIRECTION('center_axis',(0.,0.,1.));
#30336=DIRECTION('ref_axis',(1.,0.,0.));
#30337=DIRECTION('center_axis',(0.,0.,1.));
#30338=DIRECTION('ref_axis',(1.,0.,0.));
#30339=DIRECTION('center_axis',(0.,0.,1.));
#30340=DIRECTION('ref_axis',(1.,0.,0.));
#30341=DIRECTION('center_axis',(0.,0.,1.));
#30342=DIRECTION('ref_axis',(1.,0.,0.));
#30343=DIRECTION('center_axis',(0.,0.,1.));
#30344=DIRECTION('ref_axis',(1.,0.,0.));
#30345=DIRECTION('center_axis',(0.,0.,1.));
#30346=DIRECTION('ref_axis',(1.,0.,0.));
#30347=DIRECTION('center_axis',(0.,0.,1.));
#30348=DIRECTION('ref_axis',(1.,0.,0.));
#30349=DIRECTION('center_axis',(0.,0.,1.));
#30350=DIRECTION('ref_axis',(1.,0.,0.));
#30351=DIRECTION('center_axis',(0.,0.,1.));
#30352=DIRECTION('ref_axis',(1.,0.,0.));
#30353=DIRECTION('center_axis',(0.,0.,1.));
#30354=DIRECTION('ref_axis',(1.,0.,0.));
#30355=DIRECTION('center_axis',(0.,0.,1.));
#30356=DIRECTION('ref_axis',(1.,0.,0.));
#30357=DIRECTION('center_axis',(0.,0.,1.));
#30358=DIRECTION('ref_axis',(1.,0.,0.));
#30359=DIRECTION('center_axis',(0.,0.,1.));
#30360=DIRECTION('ref_axis',(1.,0.,0.));
#30361=DIRECTION('center_axis',(0.,0.,1.));
#30362=DIRECTION('ref_axis',(1.,0.,0.));
#30363=DIRECTION('',(0.,0.,-1.));
#30364=DIRECTION('center_axis',(0.,0.,1.));
#30365=DIRECTION('ref_axis',(1.,0.,0.));
#30366=DIRECTION('center_axis',(0.,0.,1.));
#30367=DIRECTION('ref_axis',(1.,0.,0.));
#30368=DIRECTION('center_axis',(0.,0.,1.));
#30369=DIRECTION('ref_axis',(1.,0.,0.));
#30370=DIRECTION('center_axis',(0.,0.,1.));
#30371=DIRECTION('ref_axis',(1.,0.,0.));
#30372=DIRECTION('center_axis',(0.,0.,1.));
#30373=DIRECTION('ref_axis',(1.,0.,0.));
#30374=DIRECTION('center_axis',(0.,0.,1.));
#30375=DIRECTION('ref_axis',(1.,0.,0.));
#30376=DIRECTION('center_axis',(0.,0.,1.));
#30377=DIRECTION('ref_axis',(1.,0.,0.));
#30378=DIRECTION('center_axis',(0.,0.,1.));
#30379=DIRECTION('ref_axis',(1.,0.,0.));
#30380=DIRECTION('center_axis',(0.,0.,1.));
#30381=DIRECTION('ref_axis',(1.,0.,0.));
#30382=DIRECTION('center_axis',(0.,0.,1.));
#30383=DIRECTION('ref_axis',(1.,0.,0.));
#30384=DIRECTION('center_axis',(0.,0.,1.));
#30385=DIRECTION('ref_axis',(1.,0.,0.));
#30386=DIRECTION('center_axis',(0.,0.,1.));
#30387=DIRECTION('ref_axis',(1.,0.,0.));
#30388=DIRECTION('center_axis',(0.,0.,1.));
#30389=DIRECTION('ref_axis',(1.,0.,0.));
#30390=DIRECTION('center_axis',(0.,0.,1.));
#30391=DIRECTION('ref_axis',(1.,0.,0.));
#30392=DIRECTION('center_axis',(0.,0.,1.));
#30393=DIRECTION('ref_axis',(1.,0.,0.));
#30394=DIRECTION('center_axis',(0.,0.,1.));
#30395=DIRECTION('ref_axis',(1.,0.,0.));
#30396=DIRECTION('center_axis',(0.,0.,1.));
#30397=DIRECTION('ref_axis',(1.,0.,0.));
#30398=DIRECTION('center_axis',(0.,0.,1.));
#30399=DIRECTION('ref_axis',(1.,0.,0.));
#30400=DIRECTION('center_axis',(0.,0.,1.));
#30401=DIRECTION('ref_axis',(1.,0.,0.));
#30402=DIRECTION('center_axis',(0.,0.,1.));
#30403=DIRECTION('ref_axis',(1.,0.,0.));
#30404=DIRECTION('center_axis',(0.,0.,-1.));
#30405=DIRECTION('ref_axis',(1.,0.,0.));
#30406=DIRECTION('center_axis',(0.,0.,1.));
#30407=DIRECTION('ref_axis',(1.,0.,0.));
#30408=DIRECTION('',(-0.707106781186547,-8.65956056235493E-17,-0.707106781186548));
#30409=DIRECTION('center_axis',(0.,0.,1.));
#30410=DIRECTION('ref_axis',(1.,0.,0.));
#30411=DIRECTION('axis',(0.,0.,1.));
#30412=DIRECTION('refdir',(1.,0.,0.));
#30413=DIRECTION('center_axis',(0.,0.,1.));
#30414=DIRECTION('ref_axis',(0.16099551660105,-0.986955137599659,0.));
#30415=DIRECTION('',(0.,0.,1.));
#30416=DIRECTION('center_axis',(0.,0.,1.));
#30417=DIRECTION('ref_axis',(1.,2.60858704573983E-14,0.));
#30418=DIRECTION('center_axis',(0.,0.,1.));
#30419=DIRECTION('ref_axis',(1.,2.60858704573983E-14,0.));
#30420=DIRECTION('',(0.,0.,1.));
#30421=DIRECTION('center_axis',(0.,0.,1.));
#30422=DIRECTION('ref_axis',(1.,2.60858704573983E-14,0.));
#30423=DIRECTION('',(0.,0.,1.));
#30424=DIRECTION('center_axis',(0.,0.,1.));
#30425=DIRECTION('ref_axis',(1.,2.60858704573983E-14,0.));
#30426=DIRECTION('',(0.,0.,1.));
#30427=DIRECTION('center_axis',(0.,0.,1.));
#30428=DIRECTION('ref_axis',(1.,2.60858704573983E-14,0.));
#30429=DIRECTION('',(0.,0.,1.));
#30430=DIRECTION('center_axis',(0.,0.,1.));
#30431=DIRECTION('ref_axis',(1.,2.60858704573983E-14,0.));
#30432=DIRECTION('',(0.,0.,1.));
#30433=DIRECTION('center_axis',(0.,0.,1.));
#30434=DIRECTION('ref_axis',(1.,2.60858704573983E-14,0.));
#30435=DIRECTION('',(0.,0.,1.));
#30436=DIRECTION('center_axis',(0.,0.,1.));
#30437=DIRECTION('ref_axis',(1.,2.60858704573983E-14,0.));
#30438=DIRECTION('',(0.,0.,1.));
#30439=DIRECTION('center_axis',(0.,0.,-1.));
#30440=DIRECTION('ref_axis',(1.,2.60858704573983E-14,0.));
#30441=DIRECTION('center_axis',(0.,0.,1.));
#30442=DIRECTION('ref_axis',(1.,0.,0.));
#30443=DIRECTION('',(0.,0.,-1.));
#30444=DIRECTION('center_axis',(0.,0.,-1.));
#30445=DIRECTION('ref_axis',(1.,0.,0.));
#30446=DIRECTION('center_axis',(0.,0.,1.));
#30447=DIRECTION('ref_axis',(1.,0.,0.));
#30448=DIRECTION('',(0.,0.,-1.));
#30449=DIRECTION('center_axis',(0.,0.,1.));
#30450=DIRECTION('ref_axis',(1.,0.,0.));
#30451=DIRECTION('',(0.,0.,-1.));
#30452=DIRECTION('center_axis',(0.,0.,1.));
#30453=DIRECTION('ref_axis',(1.,0.,0.));
#30454=DIRECTION('',(0.,0.,-1.));
#30455=DIRECTION('center_axis',(0.,0.,1.));
#30456=DIRECTION('ref_axis',(1.,0.,0.));
#30457=DIRECTION('',(0.,0.,-1.));
#30458=DIRECTION('center_axis',(0.,0.,1.));
#30459=DIRECTION('ref_axis',(1.,0.,0.));
#30460=DIRECTION('',(0.,0.,-1.));
#30461=DIRECTION('center_axis',(0.,0.,1.));
#30462=DIRECTION('ref_axis',(1.,0.,0.));
#30463=DIRECTION('',(0.,0.,-1.));
#30464=DIRECTION('center_axis',(0.,0.,1.));
#30465=DIRECTION('ref_axis',(1.,0.,0.));
#30466=DIRECTION('',(0.,0.,-1.));
#30467=DIRECTION('center_axis',(0.,0.,1.));
#30468=DIRECTION('ref_axis',(1.,0.,0.));
#30469=DIRECTION('',(0.,0.,-1.));
#30470=DIRECTION('center_axis',(0.,0.,1.));
#30471=DIRECTION('ref_axis',(-0.503961258530209,-0.863726258661069,0.));
#30472=DIRECTION('',(0.,0.,1.));
#30473=DIRECTION('center_axis',(0.,0.,1.));
#30474=DIRECTION('ref_axis',(1.,3.61234163283715E-14,0.));
#30475=DIRECTION('center_axis',(0.,0.,1.));
#30476=DIRECTION('ref_axis',(1.,3.61234163283715E-14,0.));
#30477=DIRECTION('',(0.,0.,1.));
#30478=DIRECTION('center_axis',(0.,0.,1.));
#30479=DIRECTION('ref_axis',(1.,3.61234163283715E-14,0.));
#30480=DIRECTION('',(0.,0.,1.));
#30481=DIRECTION('center_axis',(0.,0.,1.));
#30482=DIRECTION('ref_axis',(1.,3.61234163283715E-14,0.));
#30483=DIRECTION('',(0.,0.,1.));
#30484=DIRECTION('center_axis',(0.,0.,1.));
#30485=DIRECTION('ref_axis',(1.,3.61234163283715E-14,0.));
#30486=DIRECTION('',(0.,0.,1.));
#30487=DIRECTION('center_axis',(0.,0.,1.));
#30488=DIRECTION('ref_axis',(1.,3.61234163283715E-14,0.));
#30489=DIRECTION('',(0.,0.,1.));
#30490=DIRECTION('center_axis',(0.,0.,1.));
#30491=DIRECTION('ref_axis',(1.,3.61234163283715E-14,0.));
#30492=DIRECTION('',(0.,0.,1.));
#30493=DIRECTION('center_axis',(0.,0.,1.));
#30494=DIRECTION('ref_axis',(1.,3.61234163283715E-14,0.));
#30495=DIRECTION('',(0.,0.,1.));
#30496=DIRECTION('center_axis',(0.,0.,1.));
#30497=DIRECTION('ref_axis',(1.,3.61234163283715E-14,0.));
#30498=DIRECTION('',(0.,0.,1.));
#30499=DIRECTION('center_axis',(0.,0.,1.));
#30500=DIRECTION('ref_axis',(1.,0.,0.));
#30501=DIRECTION('center_axis',(0.,0.,-1.));
#30502=DIRECTION('ref_axis',(1.,0.,0.));
#30503=DIRECTION('center_axis',(0.,0.,-1.));
#30504=DIRECTION('ref_axis',(1.,0.,0.));
#30505=DIRECTION('center_axis',(0.,0.,1.));
#30506=DIRECTION('ref_axis',(0.888919796417206,0.458062872908941,0.));
#30507=DIRECTION('center_axis',(0.,0.,-1.));
#30508=DIRECTION('ref_axis',(1.,3.61234163283715E-14,0.));
#30509=DIRECTION('center_axis',(0.,0.,1.));
#30510=DIRECTION('ref_axis',(1.,0.,0.));
#30511=DIRECTION('center_axis',(0.,0.,-1.));
#30512=DIRECTION('ref_axis',(1.,0.,0.));
#30513=DIRECTION('center_axis',(0.,0.,1.));
#30514=DIRECTION('ref_axis',(1.,0.,0.));
#30515=DIRECTION('center_axis',(0.,0.,1.));
#30516=DIRECTION('ref_axis',(1.,0.,0.));
#30517=DIRECTION('center_axis',(0.,0.,1.));
#30518=DIRECTION('ref_axis',(1.,0.,0.));
#30519=DIRECTION('center_axis',(0.,0.,-1.));
#30520=DIRECTION('ref_axis',(1.,2.60858704573983E-14,0.));
#30521=DIRECTION('center_axis',(0.,0.,1.));
#30522=DIRECTION('ref_axis',(-0.997062769070685,0.0765887363330772,0.));
#30523=DIRECTION('center_axis',(0.,0.,1.));
#30524=DIRECTION('ref_axis',(1.,0.,0.));
#30525=DIRECTION('center_axis',(0.,0.,-1.));
#30526=DIRECTION('ref_axis',(1.,0.,0.));
#30527=DIRECTION('',(-0.866025403784439,-1.06057523872491E-16,0.5));
#30528=DIRECTION('center_axis',(0.5,-0.866025403784439,0.));
#30529=DIRECTION('ref_axis',(0.866025403784439,0.5,0.));
#30530=DIRECTION('',(0.,0.,1.));
#30531=DIRECTION('',(0.,0.,1.));
#30532=DIRECTION('center_axis',(1.,-3.49629579342466E-16,0.));
#30533=DIRECTION('ref_axis',(3.49629579342466E-16,1.,0.));
#30534=DIRECTION('',(0.,0.,1.));
#30535=DIRECTION('center_axis',(0.5,0.866025403784439,0.));
#30536=DIRECTION('ref_axis',(-0.866025403784439,0.5,0.));
#30537=DIRECTION('',(0.,0.,1.));
#30538=DIRECTION('center_axis',(0.,0.,-1.));
#30539=DIRECTION('ref_axis',(1.,0.,0.));
#30540=DIRECTION('',(0.866025403784439,1.06057523872491E-16,0.5));
#30541=DIRECTION('center_axis',(0.,0.,1.));
#30542=DIRECTION('ref_axis',(1.,0.,0.));
#30543=DIRECTION('center_axis',(-0.5,0.866025403784439,0.));
#30544=DIRECTION('ref_axis',(-0.866025403784439,-0.5,0.));
#30545=DIRECTION('',(0.,0.,1.));
#30546=DIRECTION('center_axis',(0.,0.,1.));
#30547=DIRECTION('ref_axis',(1.,0.,0.));
#30548=DIRECTION('center_axis',(0.,0.,1.));
#30549=DIRECTION('ref_axis',(1.,0.,0.));
#30550=DIRECTION('center_axis',(0.,0.,-1.));
#30551=DIRECTION('ref_axis',(1.,0.,0.));
#30552=DIRECTION('center_axis',(0.,0.,1.));
#30553=DIRECTION('ref_axis',(1.,0.,0.));
#30554=DIRECTION('center_axis',(0.,0.,-1.));
#30555=DIRECTION('ref_axis',(1.,0.,0.));
#30556=DIRECTION('center_axis',(0.,0.,1.));
#30557=DIRECTION('ref_axis',(1.,0.,0.));
#30558=DIRECTION('center_axis',(0.,0.,1.));
#30559=DIRECTION('ref_axis',(1.,0.,0.));
#30560=DIRECTION('center_axis',(-0.5,-0.866025403784439,0.));
#30561=DIRECTION('ref_axis',(0.866025403784439,-0.5,0.));
#30562=DIRECTION('',(0.,0.,1.));
#30563=DIRECTION('center_axis',(-1.,0.,0.));
#30564=DIRECTION('ref_axis',(0.,-1.,0.));
#30565=DIRECTION('center_axis',(0.,0.,1.));
#30566=DIRECTION('ref_axis',(1.,0.,0.));
#30567=DIRECTION('',(0.,0.,-1.));
#30568=DIRECTION('center_axis',(0.,0.,1.));
#30569=DIRECTION('ref_axis',(1.,0.,0.));
#30570=DIRECTION('center_axis',(0.,0.,1.));
#30571=DIRECTION('ref_axis',(1.,0.,0.));
#30572=DIRECTION('center_axis',(0.,0.,1.));
#30573=DIRECTION('ref_axis',(1.,0.,0.));
#30574=DIRECTION('',(0.,0.,-1.));
#30575=DIRECTION('center_axis',(0.,0.,-1.));
#30576=DIRECTION('ref_axis',(-1.,0.,0.));
#30577=DIRECTION('center_axis',(0.,0.,1.));
#30578=DIRECTION('ref_axis',(1.,0.,0.));
#30579=DIRECTION('center_axis',(0.,0.,1.));
#30580=DIRECTION('ref_axis',(1.,0.,0.));
#30581=DIRECTION('',(0.707106781186547,8.65956056235493E-17,-0.707106781186548));
#30582=DIRECTION('center_axis',(0.,0.,1.));
#30583=DIRECTION('ref_axis',(1.,0.,0.));
#30584=DIRECTION('center_axis',(0.,0.,1.));
#30585=DIRECTION('ref_axis',(1.,0.,0.));
#30586=DIRECTION('center_axis',(0.,0.,1.));
#30587=DIRECTION('ref_axis',(1.,0.,0.));
#30588=DIRECTION('',(0.,0.,-1.));
#30589=DIRECTION('center_axis',(0.,0.,-1.));
#30590=DIRECTION('ref_axis',(1.,0.,0.));
#30591=DIRECTION('center_axis',(0.,0.,1.));
#30592=DIRECTION('ref_axis',(1.,0.,0.));
#30593=DIRECTION('',(-0.707106781186545,-8.6595605623549E-17,-0.70710678118655));
#30594=DIRECTION('center_axis',(0.,0.,1.));
#30595=DIRECTION('ref_axis',(1.,0.,0.));
#30596=DIRECTION('center_axis',(0.,0.,1.));
#30597=DIRECTION('ref_axis',(1.,0.,0.));
#30598=DIRECTION('center_axis',(0.,0.,1.));
#30599=DIRECTION('ref_axis',(1.,0.,0.));
#30600=DIRECTION('',(0.207911690817759,2.54618386665283E-17,-0.978147600733806));
#30601=DIRECTION('',(-1.,3.82264778138917E-298,-2.22044604925031E-16));
#30602=DIRECTION('',(-2.22044604925031E-16,0.,1.));
#30603=DIRECTION('',(-0.965925826289069,0.,0.258819045102521));
#30604=DIRECTION('',(0.258819045102521,0.,0.965925826289069));
#30605=DIRECTION('',(-0.965925826289069,0.,0.258819045102521));
#30606=DIRECTION('',(0.258819045102521,3.08148791101958E-33,0.965925826289068));
#30607=DIRECTION('',(-1.,3.82264778138917E-298,-2.22044604925031E-16));
#30608=DIRECTION('',(-2.22044604925031E-16,0.,1.));
#30609=DIRECTION('',(-1.,0.,-2.22044604925031E-16));
#30610=DIRECTION('',(-2.22044604925031E-16,0.,1.));
#30611=DIRECTION('',(-1.,3.82264778138917E-298,-2.22044604925031E-16));
#30612=DIRECTION('',(-2.22044604925031E-16,0.,1.));
#30613=DIRECTION('',(-1.,3.82264778138917E-298,-2.22044604925031E-16));
#30614=DIRECTION('',(-2.22044604925031E-16,0.,1.));
#30615=DIRECTION('',(-1.,3.82264778138917E-298,-2.22044604925031E-16));
#30616=DIRECTION('',(-2.22044604925031E-16,0.,1.));
#30617=DIRECTION('',(-1.,0.,-2.22044604925031E-16));
#30618=DIRECTION('',(-2.22044604925031E-16,0.,1.));
#30619=DIRECTION('',(-1.,3.82264778138917E-298,-2.22044604925031E-16));
#30620=DIRECTION('',(-2.22044604925031E-16,0.,1.));
#30621=DIRECTION('',(-1.,0.,-2.22044604925031E-16));
#30622=DIRECTION('',(-2.22044604925031E-16,0.,1.));
#30623=DIRECTION('',(1.,-1.22464679914735E-16,2.22044604925031E-16));
#30624=DIRECTION('',(-2.22044604925031E-16,0.,1.));
#30625=DIRECTION('',(0.,1.,0.));
#30626=DIRECTION('',(-1.,0.,-2.22044604925031E-16));
#30627=DIRECTION('',(-2.22044604925031E-16,0.,1.));
#30628=DIRECTION('',(-1.,0.,-2.22044604925031E-16));
#30629=DIRECTION('',(0.,1.,0.));
#30630=DIRECTION('',(-1.,0.,-2.22044604925031E-16));
#30631=DIRECTION('',(-1.,3.82264778138917E-298,-2.22044604925031E-16));
#30632=DIRECTION('',(-2.22044604925031E-16,0.,1.));
#30633=DIRECTION('',(-1.,3.82264778138917E-298,-2.22044604925031E-16));
#30634=DIRECTION('',(-2.22044604925031E-16,0.,1.));
#30635=DIRECTION('',(-1.,0.,-2.22044604925031E-16));
#30636=DIRECTION('',(-2.22044604925031E-16,0.,1.));
#30637=DIRECTION('',(-1.,0.,-2.22044604925031E-16));
#30638=DIRECTION('',(-2.22044604925031E-16,0.,1.));
#30639=DIRECTION('',(-1.,0.,-2.22044604925031E-16));
#30640=DIRECTION('',(-2.22044604925031E-16,0.,1.));
#30641=DIRECTION('',(-1.,6.84227765783602E-48,-2.22044604925031E-16));
#30642=DIRECTION('',(-1.70096035727369E-16,0.642787609686539,0.766044443118978));
#30643=DIRECTION('',(-1.,6.16297582203916E-33,-2.22044604925031E-16));
#30644=DIRECTION('',(-3.85576410060052E-17,0.984807753012208,0.173648177666931));
#30645=DIRECTION('',(-1.,4.10536659470161E-47,-2.22044604925031E-16));
#30646=DIRECTION('',(1.11022302462516E-16,0.866025403784439,-0.5));
#30647=DIRECTION('',(-1.,1.23259516440783E-32,-2.22044604925031E-16));
#30648=DIRECTION('',(2.08653676733374E-16,0.342020143325669,-0.939692620785908));
#30649=DIRECTION('',(-1.,4.51590325417177E-47,-2.22044604925031E-16));
#30650=DIRECTION('',(2.08653676733374E-16,-0.342020143325669,-0.939692620785908));
#30651=DIRECTION('',(-1.,1.23259516440783E-32,-2.22044604925031E-16));
#30652=DIRECTION('',(1.11022302462516E-16,-0.866025403784438,-0.5));
#30653=DIRECTION('',(-1.,3.42113882891801E-47,-2.22044604925031E-16));
#30654=DIRECTION('',(-3.85576410060051E-17,-0.984807753012208,0.17364817766693));
#30655=DIRECTION('',(-1.,3.69778549322349E-32,-2.22044604925031E-16));
#30656=DIRECTION('',(-1.70096035727369E-16,-0.642787609686539,0.766044443118978));
#30657=DIRECTION('',(-0.965925826289069,2.29601093151022E-17,0.258819045102521));
#30658=DIRECTION('',(0.198266891274146,0.642787609686539,0.739942111693848));
#30659=DIRECTION('',(-0.965925826289069,-4.8121474944411E-19,0.258819045102521));
#30660=DIRECTION('',(0.0449434555275478,0.984807753012208,0.167731259496521));
#30661=DIRECTION('',(-0.965925826289069,2.589981594696E-17,0.258819045102521));
#30662=DIRECTION('',(-0.12940952255126,0.866025403784439,-0.482962913144534));
#30663=DIRECTION('',(-0.965925826289069,-1.72879940387092E-17,0.258819045102521));
#30664=DIRECTION('',(-0.243210346801694,0.342020143325669,-0.907673371190369));
#30665=DIRECTION('',(-0.965925826289069,1.53988719822115E-17,0.258819045102521));
#30666=DIRECTION('',(-0.243210346801694,-0.342020143325669,-0.907673371190369));
#30667=DIRECTION('',(-0.965925826289069,5.67211527639298E-18,0.258819045102521));
#30668=DIRECTION('',(-0.12940952255126,-0.866025403784438,-0.482962913144534));
#30669=DIRECTION('',(-0.965925826289069,-2.38820527658119E-18,0.258819045102521));
#30670=DIRECTION('',(0.0449434555275476,-0.984807753012208,0.16773125949652));
#30671=DIRECTION('',(-0.965925826289069,-9.62429498888215E-18,0.258819045102521));
#30672=DIRECTION('',(0.198266891274146,-0.642787609686539,0.739942111693848));
#30673=DIRECTION('',(1.,-1.22464679914735E-16,2.22044604925031E-16));
#30674=DIRECTION('',(-2.22044604925031E-16,0.,1.));
#30675=DIRECTION('',(1.,-1.22464679914735E-16,2.22044604925031E-16));
#30676=DIRECTION('',(-2.22044604925031E-16,0.,1.));
#30677=DIRECTION('',(-1.,3.82264778138917E-298,-2.22044604925031E-16));
#30678=DIRECTION('',(-2.22044604925031E-16,0.,1.));
#30679=DIRECTION('',(1.,-1.22464679914735E-16,2.22044604925031E-16));
#30680=DIRECTION('',(-2.22044604925031E-16,0.,1.));
#30681=DIRECTION('',(1.,-1.22464679914735E-16,2.22044604925031E-16));
#30682=DIRECTION('',(-2.22044604925031E-16,0.,1.));
#30683=DIRECTION('',(1.,-1.22464679914735E-16,2.22044604925031E-16));
#30684=DIRECTION('',(-2.22044604925031E-16,0.,1.));
#30685=DIRECTION('',(1.,-1.22464679914735E-16,2.22044604925031E-16));
#30686=DIRECTION('',(-2.22044604925031E-16,0.,1.));
#30687=DIRECTION('',(1.,-1.22464679914735E-16,2.22044604925031E-16));
#30688=DIRECTION('',(-2.22044604925031E-16,0.,1.));
#30689=DIRECTION('',(0.,-1.,0.));
#30690=DIRECTION('',(-1.,0.,-2.22044604925031E-16));
#30691=CARTESIAN_POINT('',(0.,0.,0.));
#30692=CARTESIAN_POINT('',(0.,0.,0.));
#30693=CARTESIAN_POINT('Origin',(2.02684561068023,-1.70072540437507,-0.28));
#30694=CARTESIAN_POINT('',(1.37684561068023,-1.70072540437507,-0.295));
#30695=CARTESIAN_POINT('Origin',(2.02684561068023,-1.70072540437507,-0.295));
#30696=CARTESIAN_POINT('',(1.40684561068023,-1.70072540437507,-0.265));
#30697=CARTESIAN_POINT('',(1.39184561068023,-1.70072540437507,-0.28));
#30698=CARTESIAN_POINT('Origin',(2.02684561068023,-1.70072540437507,-0.265));
#30699=CARTESIAN_POINT('Origin',(2.02684561068023,-1.70072540437507,-0.295));
#30700=CARTESIAN_POINT('',(1.40684561068023,-1.70072540437507,-0.025));
#30701=CARTESIAN_POINT('',(1.40684561068023,-1.70072540437507,-0.295));
#30702=CARTESIAN_POINT('Origin',(2.02684561068023,-1.70072540437507,-0.025));
#30703=CARTESIAN_POINT('Origin',(3.4,0.,-0.295));
#30704=CARTESIAN_POINT('',(-3.4,-4.163799117101E-16,-0.295));
#30705=CARTESIAN_POINT('Origin',(0.,0.,-0.295));
#30706=CARTESIAN_POINT('',(-3.13629421039049,0.904937086210529,-0.295));
#30707=CARTESIAN_POINT('Origin',(-2.48629421039049,0.904937086210529,-0.295));
#30708=CARTESIAN_POINT('',(1.99585903453311,7.96020419445779E-17,-0.295));
#30709=CARTESIAN_POINT('Origin',(2.64585903453311,0.,-0.295));
#30710=CARTESIAN_POINT('',(-3.13629421039049,-0.904937086210529,-0.295));
#30711=CARTESIAN_POINT('Origin',(-2.48629421039049,-0.904937086210529,-0.295));
#30712=CARTESIAN_POINT('',(-0.190551400289742,2.6056624905856,-0.295));
#30713=CARTESIAN_POINT('Origin',(0.459448599710258,2.6056624905856,-0.295));
#30714=CARTESIAN_POINT('',(-1.57765648986083,-1.93207197046211E-16,-0.295));
#30715=CARTESIAN_POINT('Origin',(0.,0.,-0.295));
#30716=CARTESIAN_POINT('',(-0.190551400289743,-2.6056624905856,-0.295));
#30717=CARTESIAN_POINT('Origin',(0.459448599710257,-2.6056624905856,-0.295));
#30718=CARTESIAN_POINT('',(-1.97292951726656,-2.29138113873824,-0.295));
#30719=CARTESIAN_POINT('Origin',(-1.32292951726656,-2.29138113873824,-0.295));
#30720=CARTESIAN_POINT('',(1.37684561068023,1.70072540437507,-0.295));
#30721=CARTESIAN_POINT('Origin',(2.02684561068023,1.70072540437507,-0.295));
#30722=CARTESIAN_POINT('',(-1.97292951726655,2.29138113873824,-0.295));
#30723=CARTESIAN_POINT('Origin',(-1.32292951726655,2.29138113873824,-0.295));
#30724=CARTESIAN_POINT('Origin',(2.02684561068023,-1.70072540437507,-0.01));
#30725=CARTESIAN_POINT('',(1.37684561068023,-1.70072540437507,0.005));
#30726=CARTESIAN_POINT('Origin',(2.02684561068023,-1.70072540437507,0.005));
#30727=CARTESIAN_POINT('',(1.39184561068023,-1.70072540437507,-0.01));
#30728=CARTESIAN_POINT('Origin',(1.60499221181911,0.,0.005));
#30729=CARTESIAN_POINT('',(-3.4,-4.163799117101E-16,0.00499999999999989));
#30730=CARTESIAN_POINT('Origin',(0.,0.,0.005));
#30731=CARTESIAN_POINT('',(-3.13629421039049,0.904937086210529,0.005));
#30732=CARTESIAN_POINT('Origin',(-2.48629421039049,0.904937086210529,0.005));
#30733=CARTESIAN_POINT('',(1.99585903453311,-7.96020419445779E-17,0.005));
#30734=CARTESIAN_POINT('Origin',(2.64585903453311,0.,0.005));
#30735=CARTESIAN_POINT('',(-3.13629421039049,-0.904937086210529,0.005));
#30736=CARTESIAN_POINT('Origin',(-2.48629421039049,-0.904937086210529,0.005));
#30737=CARTESIAN_POINT('',(-0.190551400289742,2.6056624905856,0.005));
#30738=CARTESIAN_POINT('Origin',(0.459448599710258,2.6056624905856,0.005));
#30739=CARTESIAN_POINT('',(-1.60499221181911,-1.9655485748607E-16,0.005));
#30740=CARTESIAN_POINT('Origin',(0.,0.,0.005));
#30741=CARTESIAN_POINT('',(-0.190551400289743,-2.6056624905856,0.005));
#30742=CARTESIAN_POINT('Origin',(0.459448599710257,-2.6056624905856,0.005));
#30743=CARTESIAN_POINT('',(-1.97292951726656,-2.29138113873824,0.005));
#30744=CARTESIAN_POINT('Origin',(-1.32292951726656,-2.29138113873824,0.005));
#30745=CARTESIAN_POINT('',(1.37684561068023,1.70072540437507,0.005));
#30746=CARTESIAN_POINT('Origin',(2.02684561068023,1.70072540437507,0.005));
#30747=CARTESIAN_POINT('',(-1.97292951726655,2.29138113873824,0.005));
#30748=CARTESIAN_POINT('Origin',(-1.32292951726655,2.29138113873824,0.005));
#30749=CARTESIAN_POINT('Origin',(-2.48629421039049,0.904937086210529,-0.28));
#30750=CARTESIAN_POINT('',(-3.10629421039049,0.904937086210529,-0.265));
#30751=CARTESIAN_POINT('',(-3.12129421039049,0.904937086210529,-0.28));
#30752=CARTESIAN_POINT('Origin',(-2.48629421039049,0.904937086210529,-0.265));
#30753=CARTESIAN_POINT('Origin',(-2.48629421039049,0.904937086210529,-0.295));
#30754=CARTESIAN_POINT('',(-3.10629421039049,0.904937086210529,-0.025));
#30755=CARTESIAN_POINT('',(-3.10629421039049,0.904937086210529,-0.295));
#30756=CARTESIAN_POINT('Origin',(-2.48629421039049,0.904937086210529,-0.025));
#30757=CARTESIAN_POINT('Origin',(-2.48629421039049,0.904937086210529,-0.01));
#30758=CARTESIAN_POINT('',(-3.12129421039049,0.904937086210529,-0.01));
#30759=CARTESIAN_POINT('Origin',(-1.32292951726655,2.29138113873824,-0.28));
#30760=CARTESIAN_POINT('',(-1.94292951726655,2.29138113873824,-0.265));
#30761=CARTESIAN_POINT('',(-1.95792951726655,2.29138113873824,-0.28));
#30762=CARTESIAN_POINT('Origin',(-1.32292951726655,2.29138113873824,-0.265));
#30763=CARTESIAN_POINT('Origin',(-1.32292951726655,2.29138113873824,-0.295));
#30764=CARTESIAN_POINT('',(-1.94292951726655,2.29138113873824,-0.025));
#30765=CARTESIAN_POINT('',(-1.94292951726655,2.29138113873824,-0.295));
#30766=CARTESIAN_POINT('Origin',(-1.32292951726655,2.29138113873824,-0.025));
#30767=CARTESIAN_POINT('Origin',(-1.32292951726655,2.29138113873824,-0.01));
#30768=CARTESIAN_POINT('',(-1.95792951726655,2.29138113873824,-0.01));
#30769=CARTESIAN_POINT('Origin',(2.64585903453311,0.,-0.28));
#30770=CARTESIAN_POINT('',(2.02585903453311,-7.59281015471359E-17,-0.265));
#30771=CARTESIAN_POINT('',(2.01085903453311,7.77650717458569E-17,-0.28));
#30772=CARTESIAN_POINT('Origin',(2.64585903453311,0.,-0.265));
#30773=CARTESIAN_POINT('Origin',(2.64585903453311,0.,-0.295));
#30774=CARTESIAN_POINT('',(2.02585903453311,7.59281015471359E-17,-0.025));
#30775=CARTESIAN_POINT('',(2.02585903453311,-7.59281015471359E-17,-0.295));
#30776=CARTESIAN_POINT('Origin',(2.64585903453311,0.,-0.025));
#30777=CARTESIAN_POINT('Origin',(2.64585903453311,0.,-0.01));
#30778=CARTESIAN_POINT('',(2.01085903453311,-7.77650717458569E-17,-0.01));
#30779=CARTESIAN_POINT('Origin',(2.02684561068023,1.70072540437507,-0.28));
#30780=CARTESIAN_POINT('',(1.40684561068023,1.70072540437507,-0.265));
#30781=CARTESIAN_POINT('',(1.39184561068023,1.70072540437507,-0.28));
#30782=CARTESIAN_POINT('Origin',(2.02684561068023,1.70072540437507,-0.265));
#30783=CARTESIAN_POINT('Origin',(2.02684561068023,1.70072540437507,-0.295));
#30784=CARTESIAN_POINT('',(1.40684561068023,1.70072540437507,-0.025));
#30785=CARTESIAN_POINT('',(1.40684561068023,1.70072540437507,-0.295));
#30786=CARTESIAN_POINT('Origin',(2.02684561068023,1.70072540437507,-0.025));
#30787=CARTESIAN_POINT('Origin',(2.02684561068023,1.70072540437507,-0.01));
#30788=CARTESIAN_POINT('',(1.39184561068023,1.70072540437507,-0.01));
#30789=CARTESIAN_POINT('Origin',(-2.48629421039049,-0.904937086210529,-0.28));
#30790=CARTESIAN_POINT('',(-3.10629421039049,-0.904937086210529,-0.265));
#30791=CARTESIAN_POINT('',(-3.12129421039049,-0.904937086210529,-0.28));
#30792=CARTESIAN_POINT('Origin',(-2.48629421039049,-0.904937086210529,-0.265));
#30793=CARTESIAN_POINT('Origin',(-2.48629421039049,-0.904937086210529,-0.295));
#30794=CARTESIAN_POINT('',(-3.10629421039049,-0.904937086210529,-0.025));
#30795=CARTESIAN_POINT('',(-3.10629421039049,-0.904937086210529,-0.295));
#30796=CARTESIAN_POINT('Origin',(-2.48629421039049,-0.904937086210529,-0.025));
#30797=CARTESIAN_POINT('Origin',(-2.48629421039049,-0.904937086210529,-0.01));
#30798=CARTESIAN_POINT('',(-3.12129421039049,-0.904937086210529,-0.01));
#30799=CARTESIAN_POINT('Origin',(-1.32292951726656,-2.29138113873824,-0.28));
#30800=CARTESIAN_POINT('',(-1.94292951726656,-2.29138113873824,-0.265));
#30801=CARTESIAN_POINT('',(-1.95792951726656,-2.29138113873824,-0.28));
#30802=CARTESIAN_POINT('Origin',(-1.32292951726656,-2.29138113873824,-0.265));
#30803=CARTESIAN_POINT('Origin',(-1.32292951726656,-2.29138113873824,-0.295));
#30804=CARTESIAN_POINT('',(-1.94292951726656,-2.29138113873824,-0.025));
#30805=CARTESIAN_POINT('',(-1.94292951726656,-2.29138113873824,-0.295));
#30806=CARTESIAN_POINT('Origin',(-1.32292951726656,-2.29138113873824,-0.025));
#30807=CARTESIAN_POINT('Origin',(-1.32292951726656,-2.29138113873824,-0.01));
#30808=CARTESIAN_POINT('',(-1.95792951726656,-2.29138113873824,-0.01));
#30809=CARTESIAN_POINT('Origin',(0.459448599710258,2.6056624905856,-0.28));
#30810=CARTESIAN_POINT('',(-0.160551400289742,2.6056624905856,-0.265));
#30811=CARTESIAN_POINT('',(-0.175551400289742,2.6056624905856,-0.28));
#30812=CARTESIAN_POINT('Origin',(0.459448599710258,2.6056624905856,-0.265));
#30813=CARTESIAN_POINT('Origin',(0.459448599710258,2.6056624905856,-0.295));
#30814=CARTESIAN_POINT('',(-0.160551400289742,2.6056624905856,-0.025));
#30815=CARTESIAN_POINT('',(-0.160551400289742,2.6056624905856,-0.295));
#30816=CARTESIAN_POINT('Origin',(0.459448599710258,2.6056624905856,-0.025));
#30817=CARTESIAN_POINT('Origin',(0.459448599710258,2.6056624905856,-0.01));
#30818=CARTESIAN_POINT('',(-0.175551400289742,2.6056624905856,-0.01));
#30819=CARTESIAN_POINT('Origin',(0.459448599710257,-2.6056624905856,-0.28));
#30820=CARTESIAN_POINT('',(-0.160551400289743,-2.6056624905856,-0.265));
#30821=CARTESIAN_POINT('',(-0.175551400289743,-2.6056624905856,-0.28));
#30822=CARTESIAN_POINT('Origin',(0.459448599710257,-2.6056624905856,-0.265));
#30823=CARTESIAN_POINT('Origin',(0.459448599710257,-2.6056624905856,-0.295));
#30824=CARTESIAN_POINT('',(-0.160551400289743,-2.6056624905856,-0.025));
#30825=CARTESIAN_POINT('',(-0.160551400289743,-2.6056624905856,-0.295));
#30826=CARTESIAN_POINT('Origin',(0.459448599710257,-2.6056624905856,-0.025));
#30827=CARTESIAN_POINT('Origin',(0.459448599710257,-2.6056624905856,-0.01));
#30828=CARTESIAN_POINT('',(-0.175551400289743,-2.6056624905856,-0.01));
#30829=CARTESIAN_POINT('Origin',(-1.77635683940025E-15,0.,8.32667268468867E-17));
#30830=CARTESIAN_POINT('Origin',(-1.77635683940025E-15,0.,8.32667268468867E-17));
#30831=CARTESIAN_POINT('Origin',(0.,0.,-0.27));
#30832=CARTESIAN_POINT('',(-3.45,-4.22503145705837E-16,-0.245));
#30833=CARTESIAN_POINT('Origin',(0.,0.,-0.245));
#30834=CARTESIAN_POINT('',(-3.425,-4.19441528707968E-16,-0.27));
#30835=CARTESIAN_POINT('Origin',(0.,0.,-0.145));
#30836=CARTESIAN_POINT('',(-3.45,-4.22503145705837E-16,-0.045));
#30837=CARTESIAN_POINT('Origin',(0.,0.,-0.045));
#30838=CARTESIAN_POINT('',(-3.45,-4.22503145705837E-16,-0.145));
#30839=CARTESIAN_POINT('Origin',(0.,0.,-0.02));
#30840=CARTESIAN_POINT('',(-3.425,-4.19441528707968E-16,-0.02));
#30841=CARTESIAN_POINT('',(0.,0.,0.));
#30842=CARTESIAN_POINT('Origin',(0.,0.,-5.38349528305703));
#30843=CARTESIAN_POINT('',(-1.49,-1.82472373072956E-16,-4.7));
#30844=CARTESIAN_POINT('Origin',(0.,0.,-4.7));
#30845=CARTESIAN_POINT('',(-1.49,-1.82472373072956E-16,-6.06699056611406));
#30846=CARTESIAN_POINT('',(-1.49,-1.82472373072956E-16,-5.38349528305703));
#30847=CARTESIAN_POINT('Origin',(0.,0.,-6.06699056611406));
#30848=CARTESIAN_POINT('Origin',(1.61,0.,-4.7));
#30849=CARTESIAN_POINT('',(-1.61,-1.97168134662724E-16,-4.7));
#30850=CARTESIAN_POINT('Origin',(0.,0.,-4.7));
#30851=CARTESIAN_POINT('Origin',(0.,0.,-4.68));
#30852=CARTESIAN_POINT('',(-1.65,-2.02066721859313E-16,-4.66));
#30853=CARTESIAN_POINT('Origin',(0.,0.,-4.66));
#30854=CARTESIAN_POINT('',(-1.63,-1.99617428261019E-16,-4.68));
#30855=CARTESIAN_POINT('Origin',(0.,0.,-4.555));
#30856=CARTESIAN_POINT('',(-1.65,-2.02066721859313E-16,-4.45));
#30857=CARTESIAN_POINT('Origin',(0.,0.,-4.45));
#30858=CARTESIAN_POINT('',(-1.65,-2.02066721859313E-16,-4.555));
#30859=CARTESIAN_POINT('Origin',(1.295,0.,-4.45));
#30860=CARTESIAN_POINT('',(-1.295,-1.58591760489582E-16,-4.45));
#30861=CARTESIAN_POINT('Origin',(0.,0.,-4.45));
#30862=CARTESIAN_POINT('Origin',(0.,0.,-4.47));
#30863=CARTESIAN_POINT('',(-1.255,-1.53693173292993E-16,-4.49));
#30864=CARTESIAN_POINT('',(-1.275,-1.56142466891288E-16,-4.47));
#30865=CARTESIAN_POINT('Origin',(0.,0.,-4.49));
#30866=CARTESIAN_POINT('Origin',(0.,0.,-5.85));
#30867=CARTESIAN_POINT('',(-1.255,-1.53693173292993E-16,-7.21));
#30868=CARTESIAN_POINT('',(-1.255,-1.53693173292993E-16,-5.85));
#30869=CARTESIAN_POINT('Origin',(0.,0.,-7.21));
#30870=CARTESIAN_POINT('Origin',(0.,0.,-7.23));
#30871=CARTESIAN_POINT('',(-1.295,-1.58591760489582E-16,-7.25));
#30872=CARTESIAN_POINT('',(-1.275,-1.56142466891288E-16,-7.23));
#30873=CARTESIAN_POINT('Origin',(0.,0.,-7.25));
#30874=CARTESIAN_POINT('Origin',(1.48323969741913,0.,-7.25));
#30875=CARTESIAN_POINT('',(-1.48323969741913,-1.81644474781263E-16,-7.25));
#30876=CARTESIAN_POINT('Origin',(0.,0.,-7.25));
#30877=CARTESIAN_POINT('Origin',(2.22044604925031E-16,0.,-6.65));
#30878=CARTESIAN_POINT('Origin',(2.22044604925031E-16,0.,-6.65));
#30879=CARTESIAN_POINT('',(0.,0.,0.));
#30880=CARTESIAN_POINT('Origin',(3.2,-0.3,-9.2));
#30881=CARTESIAN_POINT('',(3.90850354995361,-0.3,-9.2));
#30882=CARTESIAN_POINT('',(3.98873413503583,-0.3,-9.12));
#30883=CARTESIAN_POINT('Ctrl Pts',(3.90850354995361,-0.3,-9.2));
#30884=CARTESIAN_POINT('Ctrl Pts',(3.94821363792151,-0.3,-9.16040637250214));
#30885=CARTESIAN_POINT('Ctrl Pts',(3.98873413503583,-0.3,-9.12));
#30886=CARTESIAN_POINT('',(3.2,-0.3,-9.2));
#30887=CARTESIAN_POINT('',(3.56,-0.3,-9.2));
#30888=CARTESIAN_POINT('',(3.2,-0.3,-8.13377950492769));
#30889=CARTESIAN_POINT('',(3.2,-0.3,-9.2));
#30890=CARTESIAN_POINT('',(3.52930206283097,-0.299999999999879,-8.22201572672916));
#30891=CARTESIAN_POINT('',(4.23327756188404,-0.3,-8.41064539319172));
#30892=CARTESIAN_POINT('',(3.58747822293044,-0.299999999999851,-8.29761887140429));
#30893=CARTESIAN_POINT('Ctrl Pts',(3.58747822293042,-0.299999999999999,
-8.29761887140429));
#30894=CARTESIAN_POINT('Ctrl Pts',(3.57778261485426,-0.299999999999999,
-8.28501838269504));
#30895=CARTESIAN_POINT('Ctrl Pts',(3.56808690015176,-0.300000000000001,
-8.2724180070262));
#30896=CARTESIAN_POINT('Ctrl Pts',(3.54869482834287,-0.300000000000001,
-8.2472169321301));
#30897=CARTESIAN_POINT('Ctrl Pts',(3.53899853098755,-0.300000000000002,
-8.23461631057127));
#30898=CARTESIAN_POINT('Ctrl Pts',(3.52930206283095,-0.300000000000002,
-8.22201572672915));
#30899=CARTESIAN_POINT('',(3.58747822293042,-0.3,-8.6));
#30900=CARTESIAN_POINT('',(3.58747822293042,-0.3,-6.8));
#30901=CARTESIAN_POINT('',(3.92856207791095,-0.3,-8.6));
#30902=CARTESIAN_POINT('',(3.4,-0.3,-8.6));
#30903=CARTESIAN_POINT('',(3.98873413503583,-0.3,-8.66));
#30904=CARTESIAN_POINT('',(3.95864810647339,-0.3,-8.63));
#30905=CARTESIAN_POINT('',(3.98873413503583,-0.3,-8.89));
#30906=CARTESIAN_POINT('Origin',(4.1,0.3,-9.2));
#30907=CARTESIAN_POINT('',(3.98873413503583,0.3,-9.12));
#30908=CARTESIAN_POINT('',(3.90850354995361,0.3,-9.2));
#30909=CARTESIAN_POINT('Ctrl Pts',(3.98873413503583,0.3,-9.12));
#30910=CARTESIAN_POINT('Ctrl Pts',(3.94821363792151,0.3,-9.16040637250214));
#30911=CARTESIAN_POINT('Ctrl Pts',(3.90850354995361,0.3,-9.2));
#30912=CARTESIAN_POINT('',(3.98873413503583,0.3,-8.66));
#30913=CARTESIAN_POINT('',(3.98873413503583,0.3,-8.89));
#30914=CARTESIAN_POINT('',(3.92856207791095,0.3,-8.6));
#30915=CARTESIAN_POINT('',(3.95864810647339,0.3,-8.63));
#30916=CARTESIAN_POINT('',(3.58747822293042,0.3,-8.6));
#30917=CARTESIAN_POINT('',(3.85,0.3,-8.6));
#30918=CARTESIAN_POINT('',(3.58747822293156,0.299999999993159,-8.29761887140459));
#30919=CARTESIAN_POINT('',(3.58747822293042,0.3,-6.8));
#30920=CARTESIAN_POINT('',(3.52930206283204,0.299999999993599,-8.22201572672944));
#30921=CARTESIAN_POINT('Ctrl Pts',(3.52930206283095,0.300000000000001,-8.22201572672915));
#30922=CARTESIAN_POINT('Ctrl Pts',(3.53899853259429,0.300000000000001,-8.23461631265923));
#30923=CARTESIAN_POINT('Ctrl Pts',(3.54869483155032,0.300000000000001,-8.24721693629827));
#30924=CARTESIAN_POINT('Ctrl Pts',(3.56808690349722,0.300000000000001,-8.2724180113739));
#30925=CARTESIAN_POINT('Ctrl Pts',(3.57778261657339,0.299999999999999,-8.28501838492923));
#30926=CARTESIAN_POINT('Ctrl Pts',(3.58747822293042,0.299999999999999,-8.29761887140429));
#30927=CARTESIAN_POINT('',(3.2,0.3,-8.13377950492769));
#30928=CARTESIAN_POINT('',(4.65313327773554,0.3,-8.52314539319172));
#30929=CARTESIAN_POINT('',(3.2,0.3,-9.2));
#30930=CARTESIAN_POINT('',(3.2,0.3,-9.2));
#30931=CARTESIAN_POINT('',(4.01,0.3,-9.2));
#30932=CARTESIAN_POINT('Origin',(3.2,0.3,-9.2));
#30933=CARTESIAN_POINT('',(3.2,0.15,-8.13377950492769));
#30934=CARTESIAN_POINT('',(3.2,0.15,-9.2));
#30935=CARTESIAN_POINT('Origin',(3.92,0.,-9.2));
#30936=CARTESIAN_POINT('Origin',(0.,0.,-9.2));
#30937=CARTESIAN_POINT('',(1.85,-2.2655965784226E-16,-9.2));
#30938=CARTESIAN_POINT('Origin',(0.,0.,-9.2));
#30939=CARTESIAN_POINT('Origin',(0.,0.,-9.16));
#30940=CARTESIAN_POINT('Origin',(0.,0.,-9.12));
#30941=CARTESIAN_POINT('Ctrl Pts',(3.58747822293043,-0.299999999999847,
-8.29761887140429));
#30942=CARTESIAN_POINT('Ctrl Pts',(3.54359058486425,-0.824819819394348,
-8.28591130419311));
#30943=CARTESIAN_POINT('Ctrl Pts',(3.22201167914007,-1.85462953693043,-8.20013753826912));
#30944=CARTESIAN_POINT('Ctrl Pts',(2.12984786621321,-3.04615572678008,-7.90851029361343));
#30945=CARTESIAN_POINT('Ctrl Pts',(0.638165371196739,-3.66186103320656,
-7.50952634922024));
#30946=CARTESIAN_POINT('Ctrl Pts',(-0.970794977809144,-3.58699051730416,
-7.0783176016057));
#30947=CARTESIAN_POINT('Ctrl Pts',(-2.39520557608279,-2.84138111621991,
-6.69582652891509));
#30948=CARTESIAN_POINT('Ctrl Pts',(-3.36945925169178,-1.56555438904003,
-6.43378922985514));
#30949=CARTESIAN_POINT('Ctrl Pts',(-3.6,-0.521978420795187,-6.37172499639606));
#30950=CARTESIAN_POINT('Ctrl Pts',(-3.6,1.15784830776718E-15,-6.37172499639606));
#30951=CARTESIAN_POINT('Ctrl Pts',(3.56826802079061,-0.297839652204228,
-8.27246655006857));
#30952=CARTESIAN_POINT('Ctrl Pts',(3.52475967172772,-0.81888729728801,-8.2608432497174));
#30953=CARTESIAN_POINT('Ctrl Pts',(3.20600009782036,-1.84143224327734,-8.17569390742104));
#30954=CARTESIAN_POINT('Ctrl Pts',(2.12230631674708,-3.02629090956407,-7.88599714528684));
#30955=CARTESIAN_POINT('Ctrl Pts',(0.640141493156845,-3.64055636684028,
-7.48932639476278));
#30956=CARTESIAN_POINT('Ctrl Pts',(-0.960725860124494,-3.56849488474166,
-7.06031586596521));
#30957=CARTESIAN_POINT('Ctrl Pts',(-2.37955235373569,-2.82823993196693,
-6.67959485067365));
#30958=CARTESIAN_POINT('Ctrl Pts',(-3.35076472884238,-1.55884475475421,
-6.41870140344638));
#30959=CARTESIAN_POINT('Ctrl Pts',(-3.58068148347422,-0.519743282796945,
-6.35690137729811));
#30960=CARTESIAN_POINT('Ctrl Pts',(-3.58068148347422,1.15118890346963E-15,
-6.35690137729811));
#30961=CARTESIAN_POINT('Ctrl Pts',(3.54905781865079,-0.295679304408609,
-8.24731422873286));
#30962=CARTESIAN_POINT('Ctrl Pts',(3.50592875859118,-0.812954775181674,
-8.23577519524169));
#30963=CARTESIAN_POINT('Ctrl Pts',(3.18998851650066,-1.82823494962424,-8.15125027657294));
#30964=CARTESIAN_POINT('Ctrl Pts',(2.11476476728094,-3.00642609234806,-7.86348399696027));
#30965=CARTESIAN_POINT('Ctrl Pts',(0.642117615116952,-3.61925170047399,
-7.46912644030531));
#30966=CARTESIAN_POINT('Ctrl Pts',(-0.950656742439843,-3.54999925217916,
-7.04231413032472));
#30967=CARTESIAN_POINT('Ctrl Pts',(-2.36389913138858,-2.81509874771395,
-6.6633631724322));
#30968=CARTESIAN_POINT('Ctrl Pts',(-3.33207020599299,-1.5521351204684,-6.40361357703761));
#30969=CARTESIAN_POINT('Ctrl Pts',(-3.56136296694844,-0.517508144798703,
-6.34207775820016));
#30970=CARTESIAN_POINT('Ctrl Pts',(-3.56136296694844,1.14452949917207E-15,
-6.34207775820016));
#30971=CARTESIAN_POINT('Ctrl Pts',(3.52984761651097,-0.29351895661299,-8.22216190739714));
#30972=CARTESIAN_POINT('Ctrl Pts',(3.48709784545464,-0.807022253075337,
-8.21070714076598));
#30973=CARTESIAN_POINT('Ctrl Pts',(3.17397693518095,-1.81503765597115,-8.12680664572484));
#30974=CARTESIAN_POINT('Ctrl Pts',(2.10722321781481,-2.98656127513204,-7.84097084863369));
#30975=CARTESIAN_POINT('Ctrl Pts',(0.644093737077059,-3.59794703410771,
-7.44892648584784));
#30976=CARTESIAN_POINT('Ctrl Pts',(-0.940587624755193,-3.53150361961666,
-7.02431239468424));
#30977=CARTESIAN_POINT('Ctrl Pts',(-2.34824590904148,-2.80195756346098,
-6.64713149419075));
#30978=CARTESIAN_POINT('Ctrl Pts',(-3.31337568314359,-1.54542548618259,
-6.38852575062885));
#30979=CARTESIAN_POINT('Ctrl Pts',(-3.54204445042266,-0.515273006800461,
-6.32725413910221));
#30980=CARTESIAN_POINT('Ctrl Pts',(-3.54204445042266,1.13787009487452E-15,
-6.32725413910221));
#30981=CARTESIAN_POINT('',(-3.54204445042266,4.33265761729611E-16,-6.32725413910221));
#30982=CARTESIAN_POINT('Ctrl Pts',(3.52930197713685,-0.299999992182585,
-8.22201570376749));
#30983=CARTESIAN_POINT('Ctrl Pts',(3.48577865853309,-0.811262373829621,
-8.21035366569568));
#30984=CARTESIAN_POINT('Ctrl Pts',(3.17248084817531,-1.81668067931843,-8.12640577041987));
#30985=CARTESIAN_POINT('Ctrl Pts',(2.10722321781481,-2.98656127513204,-7.84097084863369));
#30986=CARTESIAN_POINT('Ctrl Pts',(0.644093737077059,-3.59794703410771,
-7.44892648584784));
#30987=CARTESIAN_POINT('Ctrl Pts',(-0.940587624755193,-3.53150361961666,
-7.02431239468424));
#30988=CARTESIAN_POINT('Ctrl Pts',(-2.34824590904148,-2.80195756346098,
-6.64713149419075));
#30989=CARTESIAN_POINT('Ctrl Pts',(-3.31337568314359,-1.54542548618259,
-6.38852575062885));
#30990=CARTESIAN_POINT('Ctrl Pts',(-3.54204445042266,-0.515273006800461,
-6.32725413910221));
#30991=CARTESIAN_POINT('Ctrl Pts',(-3.54204445042266,1.13787009487452E-15,
-6.32725413910221));
#30992=CARTESIAN_POINT('',(-3.6,-4.40872847693047E-16,-6.37172499639606));
#30993=CARTESIAN_POINT('',(-3.6,1.15784830776718E-15,-6.37172499639606));
#30994=CARTESIAN_POINT('Ctrl Pts',(-3.6,1.15784830776718E-15,-6.37172499639606));
#30995=CARTESIAN_POINT('Ctrl Pts',(-3.6,-0.521978420795187,-6.37172499639606));
#30996=CARTESIAN_POINT('Ctrl Pts',(-3.36945925169178,-1.56555438904003,
-6.43378922985514));
#30997=CARTESIAN_POINT('Ctrl Pts',(-2.39520557608279,-2.84138111621991,
-6.69582652891509));
#30998=CARTESIAN_POINT('Ctrl Pts',(-0.970794977809144,-3.58699051730416,
-7.0783176016057));
#30999=CARTESIAN_POINT('Ctrl Pts',(0.638165371196739,-3.66186103320656,
-7.50952634922024));
#31000=CARTESIAN_POINT('Ctrl Pts',(2.12984786621321,-3.04615572678008,-7.90851029361343));
#31001=CARTESIAN_POINT('Ctrl Pts',(3.22201167914007,-1.85462953693043,-8.20013753826912));
#31002=CARTESIAN_POINT('Ctrl Pts',(3.54359058486425,-0.824819819394348,
-8.28591130419311));
#31003=CARTESIAN_POINT('Ctrl Pts',(3.58747822293043,-0.299999999999847,
-8.29761887140429));
#31004=CARTESIAN_POINT('Origin',(0.,0.,-9.175));
#31005=CARTESIAN_POINT('',(1.8,2.20436423846524E-16,-9.15));
#31006=CARTESIAN_POINT('',(1.825,-2.23498040844392E-16,-9.175));
#31007=CARTESIAN_POINT('',(-1.8,-2.20436423846524E-16,-9.15));
#31008=CARTESIAN_POINT('Origin',(0.,0.,-9.15));
#31009=CARTESIAN_POINT('Origin',(0.,0.,-9.15));
#31010=CARTESIAN_POINT('Origin',(0.,0.,-7.1));
#31011=CARTESIAN_POINT('',(-1.8,5.78924153883589E-16,-6.85403354277208));
#31012=CARTESIAN_POINT('Ctrl Pts',(-1.8,5.78924153883589E-16,-6.85403354277208));
#31013=CARTESIAN_POINT('Ctrl Pts',(-1.8,0.26687426398062,-6.85403354277208));
#31014=CARTESIAN_POINT('Ctrl Pts',(-1.67940772680176,0.799740126243808,
-6.88664705235894));
#31015=CARTESIAN_POINT('Ctrl Pts',(-1.11413450545355,1.51982118043229,-7.03926580415177));
#31016=CARTESIAN_POINT('Ctrl Pts',(-0.334475738167088,1.83326108962433,
-7.24892365218508));
#31017=CARTESIAN_POINT('Ctrl Pts',(0.573750176357548,1.77351582314255,-7.49212349822523));
#31018=CARTESIAN_POINT('Ctrl Pts',(1.22793100737407,1.40256541091616,-7.66657535429114));
#31019=CARTESIAN_POINT('Ctrl Pts',(1.74830857687837,0.648316915010969,-7.80494537493236));
#31020=CARTESIAN_POINT('Ctrl Pts',(1.86228369146514,-0.0991722029991063,
-7.83518501898388));
#31021=CARTESIAN_POINT('Ctrl Pts',(1.58921257783203,-0.975508826078887,
-7.76267099529992));
#31022=CARTESIAN_POINT('Ctrl Pts',(1.0724332556989,-1.52476364806832,-7.62518482796827));
#31023=CARTESIAN_POINT('Ctrl Pts',(0.305930130124348,-1.81739157595408,
-7.42046869575053));
#31024=CARTESIAN_POINT('Ctrl Pts',(-0.429751697338143,-1.81110956273029,
-7.22333465973037));
#31025=CARTESIAN_POINT('Ctrl Pts',(-1.17066142134837,-1.44648931941929,
-7.02399504594777));
#31026=CARTESIAN_POINT('Ctrl Pts',(-1.6794416245078,-0.800547883395893,
-6.88664347771834));
#31027=CARTESIAN_POINT('Ctrl Pts',(-1.8,-0.26687426398062,-6.85403354277208));
#31028=CARTESIAN_POINT('Ctrl Pts',(-1.8,-2.20436423846524E-16,-6.85403354277208));
#31029=CARTESIAN_POINT('',(-1.8,-2.20436423846524E-16,-7.1));
#31030=CARTESIAN_POINT('Ctrl Pts',(-3.6,1.15784830776718E-15,-6.37172499639606));
#31031=CARTESIAN_POINT('Ctrl Pts',(-3.6,0.521978420795508,-6.37172499639606));
#31032=CARTESIAN_POINT('Ctrl Pts',(-3.3694145818453,1.56557914338224,-6.4338013249984));
#31033=CARTESIAN_POINT('Ctrl Pts',(-2.39509191806484,2.84110705316819,-6.69585623025017));
#31034=CARTESIAN_POINT('Ctrl Pts',(-0.970891104391535,3.58753956045663,
-7.07829389448567));
#31035=CARTESIAN_POINT('Ctrl Pts',(0.638073973195017,3.66128730235917,-7.50949972707459));
#31036=CARTESIAN_POINT('Ctrl Pts',(2.13014841105312,3.04667385631827,-7.90859191608972));
#31037=CARTESIAN_POINT('Ctrl Pts',(3.22176591600978,1.85431823154204,-8.20007153069477));
#31038=CARTESIAN_POINT('Ctrl Pts',(3.54359058486578,0.824819819388012,-8.28591130419351));
#31039=CARTESIAN_POINT('Ctrl Pts',(3.587478222931,0.299999999993108,-8.29761887140444));
#31040=CARTESIAN_POINT('Ctrl Pts',(-3.58068148347422,9.16320792421322E-16,
-6.35690137729811));
#31041=CARTESIAN_POINT('Ctrl Pts',(-3.58068148347422,0.519743282797265,
-6.35690137729811));
#31042=CARTESIAN_POINT('Ctrl Pts',(-3.3507196921498,1.55886868196113,-6.4187135549211));
#31043=CARTESIAN_POINT('Ctrl Pts',(-2.37944049713545,2.82796548033986,-6.67962432039998));
#31044=CARTESIAN_POINT('Ctrl Pts',(-0.960817466988908,3.56904327507393,
-7.06029268659327));
#31045=CARTESIAN_POINT('Ctrl Pts',(0.640044730645557,3.63998643185216,-7.48929904590942));
#31046=CARTESIAN_POINT('Ctrl Pts',(2.1226102634193,3.0267995387376,-7.88607931537165));
#31047=CARTESIAN_POINT('Ctrl Pts',(3.20575390993616,1.8411284699177,-8.17562783788156));
#31048=CARTESIAN_POINT('Ctrl Pts',(3.52475967172923,0.81888729728172,-8.2608432497178));
#31049=CARTESIAN_POINT('Ctrl Pts',(3.56826802079117,0.297839652197537,-8.27246655006872));
#31050=CARTESIAN_POINT('Ctrl Pts',(-3.56136296694844,6.74793277075467E-16,
-6.34207775820016));
#31051=CARTESIAN_POINT('Ctrl Pts',(-3.56136296694844,0.517508144799021,
-6.34207775820016));
#31052=CARTESIAN_POINT('Ctrl Pts',(-3.33202480245431,1.55215822054003,-6.4036257848438));
#31053=CARTESIAN_POINT('Ctrl Pts',(-2.36378907620607,2.81482390751152,-6.66339241054979));
#31054=CARTESIAN_POINT('Ctrl Pts',(-0.950743829586281,3.55054698969123,
-7.04229147870087));
#31055=CARTESIAN_POINT('Ctrl Pts',(0.642015488096099,3.61868556134514,-7.46909836474424));
#31056=CARTESIAN_POINT('Ctrl Pts',(2.11507211578549,3.00692522115694,-7.86356671465357));
#31057=CARTESIAN_POINT('Ctrl Pts',(3.18974190386254,1.82793870829337,-8.15118414506835));
#31058=CARTESIAN_POINT('Ctrl Pts',(3.50592875859267,0.812954775175428,-8.23577519524209));
#31059=CARTESIAN_POINT('Ctrl Pts',(3.54905781865134,0.295679304401967,-8.247314228733));
#31060=CARTESIAN_POINT('Ctrl Pts',(-3.54204445042266,4.33265761729611E-16,
-6.32725413910221));
#31061=CARTESIAN_POINT('Ctrl Pts',(-3.54204445042266,0.515273006800777,
-6.32725413910221));
#31062=CARTESIAN_POINT('Ctrl Pts',(-3.31332991275881,1.54544775911892,-6.3885380147665));
#31063=CARTESIAN_POINT('Ctrl Pts',(-2.34813765527668,2.80168233468319,-6.6471605006996));
#31064=CARTESIAN_POINT('Ctrl Pts',(-0.940670192183654,3.53205070430853,
-7.02429027080846));
#31065=CARTESIAN_POINT('Ctrl Pts',(0.643986245546639,3.59738469083813,-7.44889768357907));
#31066=CARTESIAN_POINT('Ctrl Pts',(2.10753396815167,2.98705090357626,-7.8410541139355));
#31067=CARTESIAN_POINT('Ctrl Pts',(3.17372989778892,1.81474894666904,-8.12674045225515));
#31068=CARTESIAN_POINT('Ctrl Pts',(3.48709784545612,0.807022253069137,-8.21070714076638));
#31069=CARTESIAN_POINT('Ctrl Pts',(3.52984761651152,0.293518956606396,-8.22216190739728));
#31070=CARTESIAN_POINT('Ctrl Pts',(3.587478222931,0.299999999993108,-8.29761887140444));
#31071=CARTESIAN_POINT('Ctrl Pts',(3.54359058486578,0.824819819388012,-8.28591130419351));
#31072=CARTESIAN_POINT('Ctrl Pts',(3.22176591600978,1.85431823154204,-8.20007153069477));
#31073=CARTESIAN_POINT('Ctrl Pts',(2.13014841105312,3.04667385631827,-7.90859191608972));
#31074=CARTESIAN_POINT('Ctrl Pts',(0.638073973195017,3.66128730235917,-7.50949972707459));
#31075=CARTESIAN_POINT('Ctrl Pts',(-0.970891104391535,3.58753956045663,
-7.07829389448567));
#31076=CARTESIAN_POINT('Ctrl Pts',(-2.39509191806484,2.84110705316819,-6.69585623025017));
#31077=CARTESIAN_POINT('Ctrl Pts',(-3.3694145818453,1.56557914338224,-6.4338013249984));
#31078=CARTESIAN_POINT('Ctrl Pts',(-3.6,0.521978420795508,-6.37172499639606));
#31079=CARTESIAN_POINT('Ctrl Pts',(-3.6,1.15784830776718E-15,-6.37172499639606));
#31080=CARTESIAN_POINT('Ctrl Pts',(-3.54204445042266,4.33265761729611E-16,
-6.32725413910221));
#31081=CARTESIAN_POINT('Ctrl Pts',(-3.54204445042266,0.515273006800777,
-6.32725413910221));
#31082=CARTESIAN_POINT('Ctrl Pts',(-3.31332991275881,1.54544775911892,-6.3885380147665));
#31083=CARTESIAN_POINT('Ctrl Pts',(-2.34813765527668,2.80168233468319,-6.6471605006996));
#31084=CARTESIAN_POINT('Ctrl Pts',(-0.940670192183654,3.53205070430853,
-7.02429027080846));
#31085=CARTESIAN_POINT('Ctrl Pts',(0.643986245546639,3.59738469083813,-7.44889768357907));
#31086=CARTESIAN_POINT('Ctrl Pts',(2.10753396815167,2.98705090357626,-7.8410541139355));
#31087=CARTESIAN_POINT('Ctrl Pts',(3.1722345914494,1.81639306338274,-8.12633978612904));
#31088=CARTESIAN_POINT('Ctrl Pts',(3.48577762046219,0.811261167252587,-8.21035338754543));
#31089=CARTESIAN_POINT('Ctrl Pts',(3.52930197000342,0.299999991525393,-8.22201570185609));
#31090=CARTESIAN_POINT('Origin',(5.,0.,-8.61608805130371));
#31091=CARTESIAN_POINT('',(-1.85795554957734,-2.2804350980996E-16,-6.77850440006593));
#31092=CARTESIAN_POINT('Ctrl Pts',(-1.85795554957734,-2.2804350980996E-16,
-6.77850440006593));
#31093=CARTESIAN_POINT('Ctrl Pts',(-1.85795554957734,-0.278571987572876,
-6.77850440006593));
#31094=CARTESIAN_POINT('Ctrl Pts',(-1.73080482781577,-0.835578184689179,
-6.81257433327898));
#31095=CARTESIAN_POINT('Ctrl Pts',(-1.19721215014567,-1.50451692895392,
-6.95555006034784));
#31096=CARTESIAN_POINT('Ctrl Pts',(-0.426813297908517,-1.87546640869451,
-7.16197781065465));
#31097=CARTESIAN_POINT('Ctrl Pts',(0.331666591879056,-1.87496444295698,
-7.36521188459848));
#31098=CARTESIAN_POINT('Ctrl Pts',(1.11729788835015,-1.56749433429653,-7.57572115603652));
#31099=CARTESIAN_POINT('Ctrl Pts',(1.64373118835486,-1.00063243714026,-7.71677853364164));
#31100=CARTESIAN_POINT('Ctrl Pts',(1.9212206160491,-0.101532313150842,-7.79113160170048));
#31101=CARTESIAN_POINT('Ctrl Pts',(1.80554343537535,0.664494087294352,-7.76013599455624));
#31102=CARTESIAN_POINT('Ctrl Pts',(1.27579391161014,1.44087268677251,-7.61819003747258));
#31103=CARTESIAN_POINT('Ctrl Pts',(0.607000118700147,1.82734856002952,-7.4389872807594));
#31104=CARTESIAN_POINT('Ctrl Pts',(-0.328153427773111,1.89732786062517,
-7.18841364318279));
#31105=CARTESIAN_POINT('Ctrl Pts',(-1.13784193049475,1.5804395186218,-6.97145826275776));
#31106=CARTESIAN_POINT('Ctrl Pts',(-1.73081608572944,0.834748528063086,
-6.8125713167301));
#31107=CARTESIAN_POINT('Ctrl Pts',(-1.85795554957734,0.278571987572876,
-6.77850440006593));
#31108=CARTESIAN_POINT('Ctrl Pts',(-1.85795554957734,2.2804350980996E-16,
-6.77850440006593));
#31109=CARTESIAN_POINT('Origin',(0.,0.,-6.8));
#31110=CARTESIAN_POINT('Origin',(0.,0.,-8.6));
#31111=CARTESIAN_POINT('Ctrl Pts',(-1.8,-2.20436423846524E-16,-6.85403354277208));
#31112=CARTESIAN_POINT('Ctrl Pts',(-1.8,-0.26687426398062,-6.85403354277208));
#31113=CARTESIAN_POINT('Ctrl Pts',(-1.6794416245078,-0.800547883395893,
-6.88664347771834));
#31114=CARTESIAN_POINT('Ctrl Pts',(-1.17066142134837,-1.44648931941929,
-7.02399504594777));
#31115=CARTESIAN_POINT('Ctrl Pts',(-0.429751697338143,-1.81110956273029,
-7.22333465973037));
#31116=CARTESIAN_POINT('Ctrl Pts',(0.305930130124348,-1.81739157595408,
-7.42046869575053));
#31117=CARTESIAN_POINT('Ctrl Pts',(1.0724332556989,-1.52476364806832,-7.62518482796827));
#31118=CARTESIAN_POINT('Ctrl Pts',(1.58921257783203,-0.975508826078887,
-7.76267099529992));
#31119=CARTESIAN_POINT('Ctrl Pts',(1.86228369146514,-0.0991722029991063,
-7.83518501898388));
#31120=CARTESIAN_POINT('Ctrl Pts',(1.74830857687837,0.648316915010969,-7.80494537493236));
#31121=CARTESIAN_POINT('Ctrl Pts',(1.22793100737407,1.40256541091616,-7.66657535429114));
#31122=CARTESIAN_POINT('Ctrl Pts',(0.573750176357548,1.77351582314255,-7.49212349822523));
#31123=CARTESIAN_POINT('Ctrl Pts',(-0.334475738167088,1.83326108962433,
-7.24892365218508));
#31124=CARTESIAN_POINT('Ctrl Pts',(-1.11413450545355,1.51982118043229,-7.03926580415177));
#31125=CARTESIAN_POINT('Ctrl Pts',(-1.67940772680176,0.799740126243808,
-6.88664705235894));
#31126=CARTESIAN_POINT('Ctrl Pts',(-1.8,0.26687426398062,-6.85403354277208));
#31127=CARTESIAN_POINT('Ctrl Pts',(-1.8,5.78924153883589E-16,-6.85403354277208));
#31128=CARTESIAN_POINT('Ctrl Pts',(-1.81931851652578,-2.22972119167669E-16,
-6.82885716187003));
#31129=CARTESIAN_POINT('Ctrl Pts',(-1.81931851652578,-0.270773505178038,
-6.82885716187003));
#31130=CARTESIAN_POINT('Ctrl Pts',(-1.69656269227712,-0.812224650493655,
-6.86195376290522));
#31131=CARTESIAN_POINT('Ctrl Pts',(-1.17951166428081,-1.46583185593083,
-7.00118005074779));
#31132=CARTESIAN_POINT('Ctrl Pts',(-0.428772230861601,-1.83256184471836,
-7.20288237670513));
#31133=CARTESIAN_POINT('Ctrl Pts',(0.314508950709251,-1.83658253162171,
-7.40204975869984));
#31134=CARTESIAN_POINT('Ctrl Pts',(1.08738813324932,-1.53900721014439,-7.60869693732435));
#31135=CARTESIAN_POINT('Ctrl Pts',(1.60738544800631,-0.983883363099342,
-7.74737350808049));
#31136=CARTESIAN_POINT('Ctrl Pts',(1.88192933299313,-0.0999589063830184,
-7.82050054655608));
#31137=CARTESIAN_POINT('Ctrl Pts',(1.76738686304403,0.653709305772098,-7.79000891480699));
#31138=CARTESIAN_POINT('Ctrl Pts',(1.24388530878609,1.41533450286828,-7.65044691535163));
#31139=CARTESIAN_POINT('Ctrl Pts',(0.584833490471748,1.79146006877154,-7.47441142573662));
#31140=CARTESIAN_POINT('Ctrl Pts',(-0.332368301369096,1.85461667995794,
-7.22875364918432));
#31141=CARTESIAN_POINT('Ctrl Pts',(-1.12203698046728,1.54002729316212,-7.01666329035377));
#31142=CARTESIAN_POINT('Ctrl Pts',(-1.69654384644432,0.811409593516901,
-6.86195514048266));
#31143=CARTESIAN_POINT('Ctrl Pts',(-1.81931851652578,0.270773505178039,
-6.82885716187003));
#31144=CARTESIAN_POINT('Ctrl Pts',(-1.81931851652578,4.61963939192379E-16,
-6.82885716187003));
#31145=CARTESIAN_POINT('Ctrl Pts',(-1.83863703305156,-2.25507814488814E-16,
-6.80368078096798));
#31146=CARTESIAN_POINT('Ctrl Pts',(-1.83863703305156,-0.274672746375458,
-6.80368078096798));
#31147=CARTESIAN_POINT('Ctrl Pts',(-1.71368376004645,-0.823901417591417,
-6.83726404809209));
#31148=CARTESIAN_POINT('Ctrl Pts',(-1.18836190721324,-1.48517439244238,
-6.97836505554782));
#31149=CARTESIAN_POINT('Ctrl Pts',(-0.427792764385059,-1.85401412670644,
-7.18243009367989));
#31150=CARTESIAN_POINT('Ctrl Pts',(0.323087771294154,-1.85577348728935,
-7.38363082164916));
#31151=CARTESIAN_POINT('Ctrl Pts',(1.10234301079973,-1.55325077222046,-7.59220904668044));
#31152=CARTESIAN_POINT('Ctrl Pts',(1.62555831818059,-0.9922579001198,-7.73207602086106));
#31153=CARTESIAN_POINT('Ctrl Pts',(1.90157497452111,-0.10074560976693,-7.80581607412828));
#31154=CARTESIAN_POINT('Ctrl Pts',(1.78646514920969,0.659101696533225,-7.77507245468161));
#31155=CARTESIAN_POINT('Ctrl Pts',(1.25983961019812,1.42810359482039,-7.6343184764121));
#31156=CARTESIAN_POINT('Ctrl Pts',(0.595916804585947,1.80940431440053,-7.45669935324801));
#31157=CARTESIAN_POINT('Ctrl Pts',(-0.330260864571104,1.87597227029155,
-7.20858364618355));
#31158=CARTESIAN_POINT('Ctrl Pts',(-1.12993945548101,1.56023340589196,-6.99406077655577));
#31159=CARTESIAN_POINT('Ctrl Pts',(-1.71367996608688,0.823079060789994,
-6.83726322860638));
#31160=CARTESIAN_POINT('Ctrl Pts',(-1.83863703305156,0.274672746375458,
-6.80368078096798));
#31161=CARTESIAN_POINT('Ctrl Pts',(-1.83863703305156,3.4500372450117E-16,
-6.80368078096798));
#31162=CARTESIAN_POINT('Ctrl Pts',(-1.85795554957734,-2.2804350980996E-16,
-6.77850440006593));
#31163=CARTESIAN_POINT('Ctrl Pts',(-1.85795554957734,-0.278571987572876,
-6.77850440006593));
#31164=CARTESIAN_POINT('Ctrl Pts',(-1.73080482781577,-0.835578184689179,
-6.81257433327898));
#31165=CARTESIAN_POINT('Ctrl Pts',(-1.19721215014567,-1.50451692895392,
-6.95555006034784));
#31166=CARTESIAN_POINT('Ctrl Pts',(-0.426813297908517,-1.87546640869451,
-7.16197781065465));
#31167=CARTESIAN_POINT('Ctrl Pts',(0.331666591879056,-1.87496444295698,
-7.36521188459848));
#31168=CARTESIAN_POINT('Ctrl Pts',(1.11729788835015,-1.56749433429653,-7.57572115603652));
#31169=CARTESIAN_POINT('Ctrl Pts',(1.64373118835486,-1.00063243714026,-7.71677853364164));
#31170=CARTESIAN_POINT('Ctrl Pts',(1.9212206160491,-0.101532313150842,-7.79113160170048));
#31171=CARTESIAN_POINT('Ctrl Pts',(1.80554343537535,0.664494087294352,-7.76013599455624));
#31172=CARTESIAN_POINT('Ctrl Pts',(1.27579391161014,1.44087268677251,-7.61819003747258));
#31173=CARTESIAN_POINT('Ctrl Pts',(0.607000118700147,1.82734856002952,-7.4389872807594));
#31174=CARTESIAN_POINT('Ctrl Pts',(-0.328153427773111,1.89732786062517,
-7.18841364318279));
#31175=CARTESIAN_POINT('Ctrl Pts',(-1.13784193049475,1.5804395186218,-6.97145826275776));
#31176=CARTESIAN_POINT('Ctrl Pts',(-1.73081608572944,0.834748528063086,
-6.8125713167301));
#31177=CARTESIAN_POINT('Ctrl Pts',(-1.85795554957734,0.278571987572876,
-6.77850440006593));
#31178=CARTESIAN_POINT('Ctrl Pts',(-1.85795554957734,2.2804350980996E-16,
-6.77850440006593));
#31179=CARTESIAN_POINT('',(-1.8,-2.20436423846524E-16,-6.85403354277208));
#31180=CARTESIAN_POINT('Origin',(0.,0.,-8.89));
#31181=CARTESIAN_POINT('Origin',(0.,0.,-8.66));
#31182=CARTESIAN_POINT('Origin',(0.,0.,-8.63));
#31183=CARTESIAN_POINT('Origin',(0.,0.,-8.6));
#31184=CARTESIAN_POINT('Origin',(3.6,0.,-8.6));
#31185=CARTESIAN_POINT('',(0.,0.,0.));
#31186=CARTESIAN_POINT('Origin',(0.,0.,-2.));
#31187=CARTESIAN_POINT('',(-1.61995291789844,0.00336117355255646,-2.));
#31188=CARTESIAN_POINT('',(-1.38002598764053,0.00249727018375272,-2.));
#31189=CARTESIAN_POINT('Ctrl Pts',(-1.61995291789844,0.00336117355255575,
-2.));
#31190=CARTESIAN_POINT('Ctrl Pts',(-1.61549424307396,0.162481506613328,
-2.));
#31191=CARTESIAN_POINT('Ctrl Pts',(-1.58875419089395,0.318012758496866,
-1.9999999999982));
#31192=CARTESIAN_POINT('Ctrl Pts',(-1.49275027839831,0.601309372298675,
-1.9999999999982));
#31193=CARTESIAN_POINT('Ctrl Pts',(-1.42966216744865,0.727509819034175,
-2.));
#31194=CARTESIAN_POINT('Ctrl Pts',(-1.24263066606898,1.00185310345563,-2.));
#31195=CARTESIAN_POINT('Ctrl Pts',(-1.10452674883175,1.14075648283468,-2.));
#31196=CARTESIAN_POINT('Ctrl Pts',(-0.812893641026086,1.33182547339981,
-2.));
#31197=CARTESIAN_POINT('Ctrl Pts',(-0.695845885242561,1.37569431979837,
-2.));
#31198=CARTESIAN_POINT('Ctrl Pts',(-0.600973807488825,1.39942220003299,
-2.));
#31199=CARTESIAN_POINT('Ctrl Pts',(-0.58060683846439,1.40270563705104,-2.));
#31200=CARTESIAN_POINT('Ctrl Pts',(-0.562399803406437,1.40311353681833,
-2.));
#31201=CARTESIAN_POINT('Ctrl Pts',(-0.557327933391125,1.40297057403271,
-2.));
#31202=CARTESIAN_POINT('Ctrl Pts',(-0.551673715306211,1.40166051391577,
-2.));
#31203=CARTESIAN_POINT('Ctrl Pts',(-0.550045660231946,1.40114098270715,
-2.));
#31204=CARTESIAN_POINT('Ctrl Pts',(-0.547931698369792,1.39993820927597,
-2.));
#31205=CARTESIAN_POINT('Ctrl Pts',(-0.547229470490149,1.39941927367039,
-2.));
#31206=CARTESIAN_POINT('Ctrl Pts',(-0.5462173517456,1.39827575338564,-2.));
#31207=CARTESIAN_POINT('Ctrl Pts',(-0.545868566103154,1.39771288260701,
-2.));
#31208=CARTESIAN_POINT('Ctrl Pts',(-0.545387398917564,1.3963939753859,-2.));
#31209=CARTESIAN_POINT('Ctrl Pts',(-0.545296117033786,1.39567565836781,
-2.));
#31210=CARTESIAN_POINT('Ctrl Pts',(-0.545376025403559,1.39384190830807,
-2.));
#31211=CARTESIAN_POINT('Ctrl Pts',(-0.545702512867774,1.39273799453804,
-2.00000000000012));
#31212=CARTESIAN_POINT('Ctrl Pts',(-0.547062395356521,1.38953579204815,
-2.00000000000012));
#31213=CARTESIAN_POINT('Ctrl Pts',(-0.548723311267636,1.38718205745838,
-2.));
#31214=CARTESIAN_POINT('Ctrl Pts',(-0.555563352310482,1.37927028912354,
-2.));
#31215=CARTESIAN_POINT('Ctrl Pts',(-0.563225688718851,1.37271906642457,
-2.));
#31216=CARTESIAN_POINT('Ctrl Pts',(-0.597143575123905,1.34688019040191,
-2.));
#31217=CARTESIAN_POINT('Ctrl Pts',(-0.634475174910193,1.32279953682347,
-1.99999999999601));
#31218=CARTESIAN_POINT('Ctrl Pts',(-0.773754982438386,1.22649039949967,
-1.99999999999601));
#31219=CARTESIAN_POINT('Ctrl Pts',(-0.90401491384939,1.12926273899443,-2.00000000000043));
#31220=CARTESIAN_POINT('Ctrl Pts',(-1.13965675392752,0.850355239559298,
-2.00000000000043));
#31221=CARTESIAN_POINT('Ctrl Pts',(-1.22749032481239,0.702921990413554,
-1.99999999999073));
#31222=CARTESIAN_POINT('Ctrl Pts',(-1.34378737767206,0.396439291894907,
-1.99999999999073));
#31223=CARTESIAN_POINT('Ctrl Pts',(-1.38452169713765,0.218480430629212,
-2.));
#31224=CARTESIAN_POINT('Ctrl Pts',(-1.38002598764053,0.00249727018375276,
-2.));
#31225=CARTESIAN_POINT('',(-0.749999176389368,0.000228736659435569,-2.));
#31226=CARTESIAN_POINT('Origin',(-1.5,7.2997163869104E-15,-2.09));
#31227=CARTESIAN_POINT('',(-1.64973702763284,0.000250310089940087,-2.09887467748946));
#31228=CARTESIAN_POINT('Origin',(-1.5,7.2997163869104E-15,-2.09));
#31229=CARTESIAN_POINT('Origin',(-1.5,7.2997163869104E-15,-2.09));
#31230=CARTESIAN_POINT('Origin',(0.,0.,-4.45));
#31231=CARTESIAN_POINT('',(1.61995291789861,0.00336117354644825,-4.45));
#31232=CARTESIAN_POINT('',(0.551181637679476,1.40145119755991,-4.44999999999997));
#31233=CARTESIAN_POINT('Ctrl Pts',(1.61995291789861,0.00336117354644749,
-4.45));
#31234=CARTESIAN_POINT('Ctrl Pts',(1.61528760482228,0.169855973259341,-4.45));
#31235=CARTESIAN_POINT('Ctrl Pts',(1.58623246551132,0.3322543098989,-4.45000000000239));
#31236=CARTESIAN_POINT('Ctrl Pts',(1.48200312795181,0.626180370842875,-4.45000000000239));
#31237=CARTESIAN_POINT('Ctrl Pts',(1.41386708572138,0.756188302107039,-4.45));
#31238=CARTESIAN_POINT('Ctrl Pts',(1.21256653981921,1.03640064697837,-4.45));
#31239=CARTESIAN_POINT('Ctrl Pts',(1.07053138485629,1.16765933441729,-4.45));
#31240=CARTESIAN_POINT('Ctrl Pts',(0.793916964682515,1.33970036291334,-4.45));
#31241=CARTESIAN_POINT('Ctrl Pts',(0.685050094788204,1.37914609751066,-4.45));
#31242=CARTESIAN_POINT('Ctrl Pts',(0.597251719842088,1.40004655942463,-4.45));
#31243=CARTESIAN_POINT('Ctrl Pts',(0.578519790624767,1.40289555289961,-4.45));
#31244=CARTESIAN_POINT('Ctrl Pts',(0.561493394806395,1.40308177478702,-4.45));
#31245=CARTESIAN_POINT('Ctrl Pts',(0.556741538198221,1.40288720515261,-4.45));
#31246=CARTESIAN_POINT('Ctrl Pts',(0.552311123311035,1.40179794647584,-4.45));
#31247=CARTESIAN_POINT('Ctrl Pts',(0.551743404220043,1.40163840793096,-4.45));
#31248=CARTESIAN_POINT('Ctrl Pts',(0.551181637679889,1.40145119755868,-4.45));
#31249=CARTESIAN_POINT('',(1.38002598764047,0.00249727018076643,-4.45));
#31250=CARTESIAN_POINT('',(0.749999176389352,0.000228736664649523,-4.45));
#31251=CARTESIAN_POINT('Ctrl Pts',(0.551181637679889,1.40145119755868,-4.45));
#31252=CARTESIAN_POINT('Ctrl Pts',(0.550257759386119,1.40114331236624,-4.45));
#31253=CARTESIAN_POINT('Ctrl Pts',(0.549350029564563,1.40076043740895,-4.45));
#31254=CARTESIAN_POINT('Ctrl Pts',(0.547815734993885,1.39985605892706,-4.45));
#31255=CARTESIAN_POINT('Ctrl Pts',(0.547138554067502,1.39933713661373,-4.45));
#31256=CARTESIAN_POINT('Ctrl Pts',(0.546158473208201,1.39819032015798,-4.45));
#31257=CARTESIAN_POINT('Ctrl Pts',(0.545822053337169,1.39762167328648,-4.45));
#31258=CARTESIAN_POINT('Ctrl Pts',(0.54536469712454,1.39628540347643,-4.45));
#31259=CARTESIAN_POINT('Ctrl Pts',(0.54528822880981,1.39555505046602,-4.45));
#31260=CARTESIAN_POINT('Ctrl Pts',(0.545406200377944,1.3936835057743,-4.45));
#31261=CARTESIAN_POINT('Ctrl Pts',(0.545764203801092,1.39255134723921,-4.4499999999995));
#31262=CARTESIAN_POINT('Ctrl Pts',(0.547413677033348,1.38883263821314,-4.4499999999995));
#31263=CARTESIAN_POINT('Ctrl Pts',(0.549725166268199,1.38580722469121,-4.45));
#31264=CARTESIAN_POINT('Ctrl Pts',(0.570820183212706,1.36368371960921,-4.45));
#31265=CARTESIAN_POINT('Ctrl Pts',(0.618842346650772,1.33360936522388,-4.45));
#31266=CARTESIAN_POINT('Ctrl Pts',(0.77375649475805,1.22648928125047,-4.45));
#31267=CARTESIAN_POINT('Ctrl Pts',(0.904015969469336,1.12926165467428,-4.45000000000126));
#31268=CARTESIAN_POINT('Ctrl Pts',(1.13965686376268,0.850354965350669,-4.45000000000126));
#31269=CARTESIAN_POINT('Ctrl Pts',(1.22749013747112,0.702922208817644,-4.45));
#31270=CARTESIAN_POINT('Ctrl Pts',(1.34378724077005,0.39643990907693,-4.45));
#31271=CARTESIAN_POINT('Ctrl Pts',(1.38452170468453,0.218480793454572,-4.45));
#31272=CARTESIAN_POINT('Ctrl Pts',(1.38002598764047,0.00249727018076639,
-4.45));
#31273=CARTESIAN_POINT('Origin',(1.5,2.69411970987176E-17,-4.36));
#31274=CARTESIAN_POINT('Origin',(1.5,2.69411970987176E-17,-4.36));
#31275=CARTESIAN_POINT('Ctrl Pts',(1.49998243058588,0.00487945268456504,
-4.50992061443582));
#31276=CARTESIAN_POINT('Ctrl Pts',(1.49941141170999,0.163465252269264,-4.50475906983506));
#31277=CARTESIAN_POINT('Ctrl Pts',(1.45186405026655,0.468260659554012,-4.49443439156157));
#31278=CARTESIAN_POINT('Ctrl Pts',(1.24285849641208,0.886559230778761,-4.47894878298098));
#31279=CARTESIAN_POINT('Ctrl Pts',(0.914832037666938,1.22538627239788,-4.46342570918691));
#31280=CARTESIAN_POINT('Ctrl Pts',(0.362526476214984,1.52015190223001,-4.44275032349895));
#31281=CARTESIAN_POINT('Ctrl Pts',(-0.450285458827622,1.54477765231458,
-4.41673352060185));
#31282=CARTESIAN_POINT('Ctrl Pts',(-1.26358566414186,1.00029259499041,-4.38579230410963));
#31283=CARTESIAN_POINT('Ctrl Pts',(-1.61297063863451,0.0851696210599042,
-4.35408217822798));
#31284=CARTESIAN_POINT('Ctrl Pts',(-1.36691769149066,-0.86636719535778,
-4.32382427572184));
#31285=CARTESIAN_POINT('Ctrl Pts',(-0.740664712301201,-1.39406711347056,
-4.29568368658589));
#31286=CARTESIAN_POINT('Ctrl Pts',(-0.123568561445898,-1.54231629531191,
-4.27827259231965));
#31287=CARTESIAN_POINT('Ctrl Pts',(0.477570602247783,-1.50045464230821,
-4.25010620760684));
#31288=CARTESIAN_POINT('Ctrl Pts',(1.12799462557692,-1.14561364539286,-4.21523812123688));
#31289=CARTESIAN_POINT('Ctrl Pts',(1.56388513724472,-0.389673012803625,
-4.17546007003578));
#31290=CARTESIAN_POINT('Ctrl Pts',(1.5433188232119,0.410763669941787,-4.13857735821636));
#31291=CARTESIAN_POINT('Ctrl Pts',(1.19490853879333,1.03893941579882,-4.10508910882579));
#31292=CARTESIAN_POINT('Ctrl Pts',(0.681279880783051,1.43269210784687,-4.07487536403218));
#31293=CARTESIAN_POINT('Ctrl Pts',(0.051646821861207,1.58859643745763,-4.04459309324451));
#31294=CARTESIAN_POINT('Ctrl Pts',(-0.588862535961304,1.47930900476985,
-4.01426969238989));
#31295=CARTESIAN_POINT('Ctrl Pts',(-1.13322870809872,1.1225062752352,-3.98388228335323));
#31296=CARTESIAN_POINT('Ctrl Pts',(-1.4902067993283,0.576759659588736,-3.95344539501966));
#31297=CARTESIAN_POINT('Ctrl Pts',(-1.58102020223693,0.0400740757948976,
-3.92803411508518));
#31298=CARTESIAN_POINT('Ctrl Pts',(-1.52052962309553,-0.384828263720139,
-3.90767925424071));
#31299=CARTESIAN_POINT('Ctrl Pts',(-1.3748830928401,-0.788957250234775,
-3.88730621071591));
#31300=CARTESIAN_POINT('Ctrl Pts',(-1.0423371162911,-1.22218867468557,-3.86180720794638));
#31301=CARTESIAN_POINT('Ctrl Pts',(-0.467378790598492,-1.53972799805516,
-3.83115568482052));
#31302=CARTESIAN_POINT('Ctrl Pts',(0.187274531141039,-1.60068158914455,
-3.80045226057647));
#31303=CARTESIAN_POINT('Ctrl Pts',(0.883096272461548,-1.37238382842803,
-3.76628010013367));
#31304=CARTESIAN_POINT('Ctrl Pts',(1.45542862121288,-0.785128737057825,
-3.72861800828645));
#31305=CARTESIAN_POINT('Ctrl Pts',(1.62183852895481,-0.0567398924127903,
-3.69430530328978));
#31306=CARTESIAN_POINT('Ctrl Pts',(1.51242393883133,0.515046269014153,-3.66681113832745));
#31307=CARTESIAN_POINT('Ctrl Pts',(1.25371395215128,1.0371419048164,-3.63928782397711));
#31308=CARTESIAN_POINT('Ctrl Pts',(0.679041108905056,1.51956040430477,-3.60482953394523));
#31309=CARTESIAN_POINT('Ctrl Pts',(-0.213247562120534,1.65433450298338,
-3.56339447382386));
#31310=CARTESIAN_POINT('Ctrl Pts',(-1.04680323812526,1.30346814108,-3.52187569315801));
#31311=CARTESIAN_POINT('Ctrl Pts',(-1.57557751626781,0.567442201034068,
-3.48027478133792));
#31312=CARTESIAN_POINT('Ctrl Pts',(-1.64318830952972,-0.337637019006298,
-3.43859332018342));
#31313=CARTESIAN_POINT('Ctrl Pts',(-1.22844519515377,-1.14714492715669,
-3.39683307764518));
#31314=CARTESIAN_POINT('Ctrl Pts',(-0.451245980735406,-1.62215680765017,
-3.35499576544402));
#31315=CARTESIAN_POINT('Ctrl Pts',(0.461841974941765,-1.62319460304399,
-3.31308315566976));
#31316=CARTESIAN_POINT('Ctrl Pts',(1.17649440309474,-1.18543555842648,-3.27459582000513));
#31317=CARTESIAN_POINT('Ctrl Pts',(1.5636738872075,-0.54221871976191,-3.23955517618414));
#31318=CARTESIAN_POINT('Ctrl Pts',(1.65231581225766,0.128238780519003,-3.20797910267182));
#31319=CARTESIAN_POINT('Ctrl Pts',(1.46493973472583,0.779138006438161,-3.17636441807156));
#31320=CARTESIAN_POINT('Ctrl Pts',(1.03253139188493,1.30136595938992,-3.14471191495533));
#31321=CARTESIAN_POINT('Ctrl Pts',(0.426609970086491,1.60751024918497,-3.11302251069183));
#31322=CARTESIAN_POINT('Ctrl Pts',(-0.251933879032834,1.64584505089144,
-3.08129700553233));
#31323=CARTESIAN_POINT('Ctrl Pts',(-0.889905805470703,1.40942555957253,
-3.04953632759992));
#31324=CARTESIAN_POINT('Ctrl Pts',(-1.38068331350981,0.937053401938582,
-3.01774135131172));
#31325=CARTESIAN_POINT('Ctrl Pts',(-1.64184179716058,0.307317409087506,
-2.98591300518706));
#31326=CARTESIAN_POINT('Ctrl Pts',(-1.62957916709941,-0.37530803509689,
-2.95405221275351));
#31327=CARTESIAN_POINT('Ctrl Pts',(-1.34474730528677,-0.996034495385219,
-2.92215989404433));
#31328=CARTESIAN_POINT('Ctrl Pts',(-0.778879409529726,-1.50350912987896,
-2.88668999089474));
#31329=CARTESIAN_POINT('Ctrl Pts',(0.0452156959044932,-1.71370006437942,
-2.84763094470004));
#31330=CARTESIAN_POINT('Ctrl Pts',(0.785100365893931,-1.486208751186,-2.81208062847635));
#31331=CARTESIAN_POINT('Ctrl Pts',(1.24161679713701,-1.09259013745182,-2.7836165314676));
#31332=CARTESIAN_POINT('Ctrl Pts',(1.49217131201598,-0.716178712962469,
-2.76225639002869));
#31333=CARTESIAN_POINT('Ctrl Pts',(1.63085414425123,-0.285537734548898,
-2.7408855262812));
#31334=CARTESIAN_POINT('Ctrl Pts',(1.65475200752033,0.317728375257333,-2.7123738937245));
#31335=CARTESIAN_POINT('Ctrl Pts',(1.37145521865962,1.04076278423927,-2.67671479060714));
#31336=CARTESIAN_POINT('Ctrl Pts',(0.69041646931577,1.55777895441666,-2.63743464573646));
#31337=CARTESIAN_POINT('Ctrl Pts',(-0.0643948515707663,1.68574777587918,
-2.6017316079884));
#31338=CARTESIAN_POINT('Ctrl Pts',(-0.733422672005601,1.52073388540773,
-2.56950115646222));
#31339=CARTESIAN_POINT('Ctrl Pts',(-1.28085476582717,1.10113604465525,-2.53741554342871));
#31340=CARTESIAN_POINT('Ctrl Pts',(-1.61517951924605,0.4975562304161,-2.50499073603886));
#31341=CARTESIAN_POINT('Ctrl Pts',(-1.68029840248005,-0.189791143389858,
-2.47314557601871));
#31342=CARTESIAN_POINT('Ctrl Pts',(-1.46497737904047,-0.846156793246451,
-2.44020210847229));
#31343=CARTESIAN_POINT('Ctrl Pts',(-1.00508021286665,-1.36188270355857,
-2.40899190246463));
#31344=CARTESIAN_POINT('Ctrl Pts',(-0.507582321376923,-1.59058364540096,
-2.38240038156976));
#31345=CARTESIAN_POINT('Ctrl Pts',(-0.115985349294589,-1.64889286597431,
-2.36303576958252));
#31346=CARTESIAN_POINT('Ctrl Pts',(0.223158570335046,-1.64681924620263,
-2.349562123073));
#31347=CARTESIAN_POINT('Ctrl Pts',(0.806901355148856,-1.50671742388011,
-2.33231544041505));
#31348=CARTESIAN_POINT('Ctrl Pts',(1.48644477626825,-0.934917871941825,
-2.30237235343056));
#31349=CARTESIAN_POINT('Ctrl Pts',(1.75362331696032,0.0983401101520701,
-2.26920259215576));
#31350=CARTESIAN_POINT('Ctrl Pts',(1.37388207698597,1.09486845045221,-2.23481640537456));
#31351=CARTESIAN_POINT('Ctrl Pts',(0.486437491100621,1.68918937268853,-2.20098350021554));
#31352=CARTESIAN_POINT('Ctrl Pts',(-0.402275175720241,1.66276347810902,
-2.172565595614));
#31353=CARTESIAN_POINT('Ctrl Pts',(-1.0075498708897,1.33971834323449,-2.14990060001603));
#31354=CARTESIAN_POINT('Ctrl Pts',(-1.36740441992316,0.968073875003734,
-2.13287342310861));
#31355=CARTESIAN_POINT('Ctrl Pts',(-1.59664060478066,0.509453342147398,
-2.11589441486025));
#31356=CARTESIAN_POINT('Ctrl Pts',(-1.64911395659225,0.173292258411803,
-2.10450673116507));
#31357=CARTESIAN_POINT('Ctrl Pts',(-1.64973702763284,0.000250310089940127,
-2.09887467748946));
#31358=CARTESIAN_POINT('Ctrl Pts',(1.45510282646556,0.00471785498059619,
-4.50992061443582));
#31359=CARTESIAN_POINT('Ctrl Pts',(1.45454752466905,0.158938640195152,-4.50490113940505));
#31360=CARTESIAN_POINT('Ctrl Pts',(1.40849772159958,0.454254551280147,-4.4948981491038));
#31361=CARTESIAN_POINT('Ctrl Pts',(1.20562360660865,0.860308403854419,-4.47986552905065));
#31362=CARTESIAN_POINT('Ctrl Pts',(0.887402599021796,1.18901004224185,-4.4648071396859));
#31363=CARTESIAN_POINT('Ctrl Pts',(0.351571093928312,1.47496328750251,-4.44474869215259));
#31364=CARTESIAN_POINT('Ctrl Pts',(-0.437170053702789,1.49892968332643,
-4.41950289723679));
#31365=CARTESIAN_POINT('Ctrl Pts',(-1.22639094877331,0.970527058656368,
-4.38947856346812));
#31366=CARTESIAN_POINT('Ctrl Pts',(-1.56553430420601,0.0823976185849323,
-4.35870345993953));
#31367=CARTESIAN_POINT('Ctrl Pts',(-1.32668502908212,-0.841248004046866,
-4.3293339124924));
#31368=CARTESIAN_POINT('Ctrl Pts',(-0.718804245962794,-1.3535248584667,
-4.30201769448259));
#31369=CARTESIAN_POINT('Ctrl Pts',(-0.119616083437381,-1.49748731273866,
-4.28511330421243));
#31370=CARTESIAN_POINT('Ctrl Pts',(0.464392315734694,-1.45682492507003,
-4.25775092153805));
#31371=CARTESIAN_POINT('Ctrl Pts',(1.09590581605906,-1.11228111397,-4.22389805157936));
#31372=CARTESIAN_POINT('Ctrl Pts',(1.51943003519238,-0.377938979423637,
-4.18525403699039));
#31373=CARTESIAN_POINT('Ctrl Pts',(1.49945180577348,0.399795741367386,-4.14941989597277));
#31374=CARTESIAN_POINT('Ctrl Pts',(1.16087569397544,1.01030847094984,-4.11687476750201));
#31375=CARTESIAN_POINT('Ctrl Pts',(0.661597764502885,1.3930744361422,-4.08750627336111));
#31376=CARTESIAN_POINT('Ctrl Pts',(0.0494009166153912,1.54468470898889,
-4.05806288385645));
#31377=CARTESIAN_POINT('Ctrl Pts',(-0.573489867817984,1.43841917455019,
-4.02857543250609));
#31378=CARTESIAN_POINT('Ctrl Pts',(-1.1030291321629,1.09136473006051,-3.99901773693845));
#31379=CARTESIAN_POINT('Ctrl Pts',(-1.45037403297912,0.560371410645132,
-3.96940462755079));
#31380=CARTESIAN_POINT('Ctrl Pts',(-1.53876993207835,0.0380711920125209,
-3.94467586616708));
#31381=CARTESIAN_POINT('Ctrl Pts',(-1.47988735353637,-0.375559805356409,
-3.92486153483449));
#31382=CARTESIAN_POINT('Ctrl Pts',(-1.33809000327692,-0.769022130747614,
-3.90502683865905));
#31383=CARTESIAN_POINT('Ctrl Pts',(-1.01429688563516,-1.19088230653178,
-3.88019939660311));
#31384=CARTESIAN_POINT('Ctrl Pts',(-0.454279919642091,-1.50020353066735,
-3.85034542265613));
#31385=CARTESIAN_POINT('Ctrl Pts',(0.183559018927454,-1.55960563373112,
-3.82043199601657));
#31386=CARTESIAN_POINT('Ctrl Pts',(0.861714986247691,-1.33714723859362,
-3.78713056579467));
#31387=CARTESIAN_POINT('Ctrl Pts',(1.4197478806152,-0.764603217162326,-3.75041228389878));
#31388=CARTESIAN_POINT('Ctrl Pts',(1.58212224236173,-0.0541615033134914,
-3.71694606817844));
#31389=CARTESIAN_POINT('Ctrl Pts',(1.47536678436316,0.503744741559664,-3.69012109357611));
#31390=CARTESIAN_POINT('Ctrl Pts',(1.2228858711314,1.01330066058605,-3.66325987802185));
#31391=CARTESIAN_POINT('Ctrl Pts',(0.661929474527082,1.48426168834351,-3.62962626014974));
#31392=CARTESIAN_POINT('Ctrl Pts',(-0.209612810380294,1.61597543556883,
-3.58915502450247));
#31393=CARTESIAN_POINT('Ctrl Pts',(-1.02416860071843,1.27316933612582,-3.54858706369704));
#31394=CARTESIAN_POINT('Ctrl Pts',(-1.54118963552779,0.553614476292706,
-3.50791814852041));
#31395=CARTESIAN_POINT('Ctrl Pts',(-1.60738332573138,-0.331738430311634,
-3.46714639909406));
#31396=CARTESIAN_POINT('Ctrl Pts',(-1.2015636321068,-1.12400675283059,-3.42628185077074));
#31397=CARTESIAN_POINT('Ctrl Pts',(-0.440570504989179,-1.58916985286069,
-3.38531848879486));
#31398=CARTESIAN_POINT('Ctrl Pts',(0.454033404816424,-1.5902877858928,-3.34425700144878));
#31399=CARTESIAN_POINT('Ctrl Pts',(1.15461602494958,-1.16119312150655,-3.30653178058679));
#31400=CARTESIAN_POINT('Ctrl Pts',(1.53440095120327,-0.530368167453922,
-3.27216645108545));
#31401=CARTESIAN_POINT('Ctrl Pts',(1.62139701755051,0.127469077736369,-3.24118754526318));
#31402=CARTESIAN_POINT('Ctrl Pts',(1.4375012114545,0.766409474357195,-3.21015627916876));
#31403=CARTESIAN_POINT('Ctrl Pts',(1.01287850477676,1.27928217401078,-3.17907466398971));
#31404=CARTESIAN_POINT('Ctrl Pts',(0.417585531284891,1.58009332728318,-3.14794269660965));
#31405=CARTESIAN_POINT('Ctrl Pts',(-0.24937400777572,1.61780796260654,-3.11676146483555));
#31406=CARTESIAN_POINT('Ctrl Pts',(-0.876750747439923,1.38534894722237,
-3.08553114835378));
#31407=CARTESIAN_POINT('Ctrl Pts',(-1.3596198640501,0.920645586859557,-3.05425345678686));
#31408=CARTESIAN_POINT('Ctrl Pts',(-1.61669866354154,0.300811039804161,
-3.0229270383574));
#31409=CARTESIAN_POINT('Ctrl Pts',(-1.60467642728968,-0.37137754361641,
-2.99155741605365));
#31410=CARTESIAN_POINT('Ctrl Pts',(-1.32404618183457,-0.982979421915755,
-2.96013498111486));
#31411=CARTESIAN_POINT('Ctrl Pts',(-0.766355189816308,-1.48322023143898,
-2.92517889171936));
#31412=CARTESIAN_POINT('Ctrl Pts',(0.0464056028336514,-1.69056552793571,
-2.88665889726854));
#31413=CARTESIAN_POINT('Ctrl Pts',(0.776600509199771,-1.46615811326241,
-2.85157844149717));
#31414=CARTESIAN_POINT('Ctrl Pts',(1.22735642696635,-1.07750731629039,-2.82347612838631));
#31415=CARTESIAN_POINT('Ctrl Pts',(1.47484842707153,-0.705728194344337,
-2.80237963780291));
#31416=CARTESIAN_POINT('Ctrl Pts',(1.61187698899787,-0.280233965655355,
-2.78126552591687));
#31417=CARTESIAN_POINT('Ctrl Pts',(1.63552656943133,0.316004400180914,-2.75308837711847));
#31418=CARTESIAN_POINT('Ctrl Pts',(1.35542815699613,1.03097669758719,-2.71783039275668));
#31419=CARTESIAN_POINT('Ctrl Pts',(0.681591813741207,1.54267081583712,-2.67896420633375));
#31420=CARTESIAN_POINT('Ctrl Pts',(-0.0657304674736995,1.66938144289853,
-2.64361972146493));
#31421=CARTESIAN_POINT('Ctrl Pts',(-0.728459598467511,1.50597117974898,
-2.61169604658853));
#31422=CARTESIAN_POINT('Ctrl Pts',(-1.27108164157649,1.09009694581586,-2.5798958762368));
#31423=CARTESIAN_POINT('Ctrl Pts',(-1.60263472112972,0.491587080445162,
-2.5477443377726));
#31424=CARTESIAN_POINT('Ctrl Pts',(-1.66730050026108,-0.190309275946086,
-2.51615578492575));
#31425=CARTESIAN_POINT('Ctrl Pts',(-1.4535316170482,-0.841935362299378,
-2.48345101010048));
#31426=CARTESIAN_POINT('Ctrl Pts',(-0.99697781119108,-1.35401375496871,
-2.45246871933706));
#31427=CARTESIAN_POINT('Ctrl Pts',(-0.502281440075284,-1.58146609712131,
-2.42602723665317));
#31428=CARTESIAN_POINT('Ctrl Pts',(-0.113329985518638,-1.63932913604753,
-2.40679514213764));
#31429=CARTESIAN_POINT('Ctrl Pts',(0.223307236973708,-1.637305094972,-2.39342050361475));
#31430=CARTESIAN_POINT('Ctrl Pts',(0.803850375083042,-1.49798534345799,
-2.3762688644909));
#31431=CARTESIAN_POINT('Ctrl Pts',(1.48000174465472,-0.929188506823542,
-2.34648398480332));
#31432=CARTESIAN_POINT('Ctrl Pts',(1.74598338432573,0.099297463661904,-2.31347001378341));
#31433=CARTESIAN_POINT('Ctrl Pts',(1.36789648672402,1.09184682624234,-2.27922670008243));
#31434=CARTESIAN_POINT('Ctrl Pts',(0.483572804326568,1.68418169796343,-2.24551390979881));
#31435=CARTESIAN_POINT('Ctrl Pts',(-0.402469297378992,1.65792813194365,
-2.21718495505266));
#31436=CARTESIAN_POINT('Ctrl Pts',(-1.00627030119693,1.33568637362211,-2.19457630535992));
#31437=CARTESIAN_POINT('Ctrl Pts',(-1.36531073202229,0.964891234942623,
-2.17758876089345));
#31438=CARTESIAN_POINT('Ctrl Pts',(-1.59412943474217,0.507099713140616,
-2.16064102435677));
#31439=CARTESIAN_POINT('Ctrl Pts',(-1.64646343907663,0.171569527018422,
-2.14927588835418));
#31440=CARTESIAN_POINT('Ctrl Pts',(-1.64708558907132,-0.00121662450613402,
-2.14365216018176));
#31441=CARTESIAN_POINT('Ctrl Pts',(1.36564437383322,0.00299830309728786,
-4.46698500844523));
#31442=CARTESIAN_POINT('Ctrl Pts',(1.36512056166741,0.14847365365975,-4.46225017397578));
#31443=CARTESIAN_POINT('Ctrl Pts',(1.32205588817515,0.424821325024859,-4.4528904930609));
#31444=CARTESIAN_POINT('Ctrl Pts',(1.13146568593075,0.806300079699337,-4.43876647060324));
#31445=CARTESIAN_POINT('Ctrl Pts',(0.83303740744264,1.11453898701874,-4.42464625577753));
#31446=CARTESIAN_POINT('Ctrl Pts',(0.330622404965623,1.38259481072421,-4.40583938673523));
#31447=CARTESIAN_POINT('Ctrl Pts',(-0.408938205861571,1.4051285585363,-4.38216721772983));
#31448=CARTESIAN_POINT('Ctrl Pts',(-1.14843067370881,0.909838347394963,
-4.35403399920661));
#31449=CARTESIAN_POINT('Ctrl Pts',(-1.4660714086033,0.0779076896382552,
-4.32520462684135));
#31450=CARTESIAN_POINT('Ctrl Pts',(-1.24240261126513,-0.786987507711687,
-4.29770408534344));
#31451=CARTESIAN_POINT('Ctrl Pts',(-0.673251260258778,-1.26651394510792,
-4.27213127287878));
#31452=CARTESIAN_POINT('Ctrl Pts',(-0.112548063135537,-1.40121802635335,
-4.2563114471826));
#31453=CARTESIAN_POINT('Ctrl Pts',(0.433526818334189,-1.36318411131058,
-4.23072532326754));
#31454=CARTESIAN_POINT('Ctrl Pts',(1.02460410701995,-1.04076477994048,-4.19904097395093));
#31455=CARTESIAN_POINT('Ctrl Pts',(1.4205924658604,-0.353935013756109,-4.16290176943614));
#31456=CARTESIAN_POINT('Ctrl Pts',(1.40193814029895,0.373333431475129,-4.12939036340684));
#31457=CARTESIAN_POINT('Ctrl Pts',(1.08535118686797,0.944116541019827,-4.09896301989612));
#31458=CARTESIAN_POINT('Ctrl Pts',(0.618607011932545,1.3019369871989,-4.071507266218));
#31459=CARTESIAN_POINT('Ctrl Pts',(0.0463502533893912,1.44364451385337,
-4.04398496829799));
#31460=CARTESIAN_POINT('Ctrl Pts',(-0.535875961508617,1.34430992342794,
-4.01642164873276));
#31461=CARTESIAN_POINT('Ctrl Pts',(-1.03082420319812,1.01991657951941,-3.98879394504289));
#31462=CARTESIAN_POINT('Ctrl Pts',(-1.35547970359203,0.5236067565516,-3.96111443236515));
#31463=CARTESIAN_POINT('Ctrl Pts',(-1.43810340325584,0.0354024237288245,
-3.93799920689023));
#31464=CARTESIAN_POINT('Ctrl Pts',(-1.38306440274653,-0.351224607303122,
-3.91947818309481));
#31465=CARTESIAN_POINT('Ctrl Pts',(-1.25051960963485,-0.719009372353289,
-3.90093755375014));
#31466=CARTESIAN_POINT('Ctrl Pts',(-0.9478237995269,-1.11338159222678,-3.87772690939149));
#31467=CARTESIAN_POINT('Ctrl Pts',(-0.424254634930679,-1.40256973512589,
-3.84981484028182));
#31468=CARTESIAN_POINT('Ctrl Pts',(0.172150116742664,-1.45812247657558,
-3.82184372666044));
#31469=CARTESIAN_POINT('Ctrl Pts',(0.806355645673129,-1.2500776649494,-3.7906986514273));
#31470=CARTESIAN_POINT('Ctrl Pts',(1.32834851019025,-0.714563943681758,
-3.75635262109906));
#31471=CARTESIAN_POINT('Ctrl Pts',(1.48028559286423,-0.0498447353164157,
-3.72503879231576));
#31472=CARTESIAN_POINT('Ctrl Pts',(1.38038560298628,0.472284190050553,-3.69993305552108));
#31473=CARTESIAN_POINT('Ctrl Pts',(1.14406395494764,0.949230241536377,-3.67479026498734));
#31474=CARTESIAN_POINT('Ctrl Pts',(0.618830831732985,1.39024534500437,-3.64329428001503));
#31475=CARTESIAN_POINT('Ctrl Pts',(-0.197498799202977,1.5136521612102,-3.60538582641974));
#31476=CARTESIAN_POINT('Ctrl Pts',(-0.960858723113836,1.192449871528,-3.5673659492302));
#31477=CARTESIAN_POINT('Ctrl Pts',(-1.44565750094265,0.517835447084338,
-3.52923274996662));
#31478=CARTESIAN_POINT('Ctrl Pts',(-1.50781755081897,-0.312675262246022,
-3.49098527721761));
#31479=CARTESIAN_POINT('Ctrl Pts',(-1.12694040401255,-1.05636654813868,
-3.45262377784345));
#31480=CARTESIAN_POINT('Ctrl Pts',(-0.412229663537864,-1.49333759815456,
-3.4141470035369));
#31481=CARTESIAN_POINT('Ctrl Pts',(0.428529887771001,-1.49443789364399,
-3.37555425331632));
#31482=CARTESIAN_POINT('Ctrl Pts',(1.08747468318201,-1.0909564983591,-3.34007136060003));
#31483=CARTESIAN_POINT('Ctrl Pts',(1.44490170910797,-0.497305657233017,
-3.30772907336355));
#31484=CARTESIAN_POINT('Ctrl Pts',(1.52686081915866,0.122132658888342,-3.27855553874415));
#31485=CARTESIAN_POINT('Ctrl Pts',(1.35362676450459,0.72414602415009,-3.24931620216265));
#31486=CARTESIAN_POINT('Ctrl Pts',(0.953336978464486,1.20768860107748,-3.22001110046922));
#31487=CARTESIAN_POINT('Ctrl Pts',(0.391777207851056,1.49149646372825,-3.19064014526287));
#31488=CARTESIAN_POINT('Ctrl Pts',(-0.237812469329778,1.5271364309313,-3.16120332898548));
#31489=CARTESIAN_POINT('Ctrl Pts',(-0.830452510837174,1.30759332277035,
-3.13170067053968));
#31490=CARTESIAN_POINT('Ctrl Pts',(-1.28691377096919,0.868353783196376,
-3.10213215114974));
#31491=CARTESIAN_POINT('Ctrl Pts',(-1.5301383889915,0.282059188023131,-3.07249793743809));
#31492=CARTESIAN_POINT('Ctrl Pts',(-1.51878600906589,-0.354268344444937,
-3.04279785637424));
#31493=CARTESIAN_POINT('Ctrl Pts',(-1.2530203435885,-0.93363236576551,-3.01303256849989));
#31494=CARTESIAN_POINT('Ctrl Pts',(-0.724301057338272,-1.40791234860284,
-2.97988677408191));
#31495=CARTESIAN_POINT('Ctrl Pts',(0.0468746538144823,-1.60479660643063,
-2.94333378242155));
#31496=CARTESIAN_POINT('Ctrl Pts',(0.740522856114257,-1.39169559570181,
-2.91000702535252));
#31497=CARTESIAN_POINT('Ctrl Pts',(1.16907313648626,-1.02223809055501,-2.8832883223016));
#31498=CARTESIAN_POINT('Ctrl Pts',(1.40448788238127,-0.668614463283503,
-2.86322030241676));
#31499=CARTESIAN_POINT('Ctrl Pts',(1.53492200943615,-0.263670870959058,
-2.84312433060443));
#31500=CARTESIAN_POINT('Ctrl Pts',(1.5574480684303,0.304104721328589,-2.81628922451734));
#31501=CARTESIAN_POINT('Ctrl Pts',(1.29062037388942,0.985613785912805,-2.78268149268605));
#31502=CARTESIAN_POINT('Ctrl Pts',(0.647699213853048,1.47393931268053,-2.74559209089865));
#31503=CARTESIAN_POINT('Ctrl Pts',(-0.0661637106574882,1.59508465851339,
-2.71182558541953));
#31504=CARTESIAN_POINT('Ctrl Pts',(-0.699830879117748,1.43887216823776,
-2.6812977430018));
#31505=CARTESIAN_POINT('Ctrl Pts',(-1.21911543936887,1.04100749299459,-2.6508681567748));
#31506=CARTESIAN_POINT('Ctrl Pts',(-1.53673793949955,0.46767973597802,-2.62006378969118));
#31507=CARTESIAN_POINT('Ctrl Pts',(-1.59885321468961,-0.186031386396118,
-2.58977995398835));
#31508=CARTESIAN_POINT('Ctrl Pts',(-1.39361588679409,-0.811583371395079,
-2.55837730926266));
#31509=CARTESIAN_POINT('Ctrl Pts',(-0.955435913036199,-1.30328784573889,
-2.52863536138063));
#31510=CARTESIAN_POINT('Ctrl Pts',(-0.479035310509762,-1.52243375827867,
-2.50316549095361));
#31511=CARTESIAN_POINT('Ctrl Pts',(-0.105466661007127,-1.57792184412725,
-2.48469593502962));
#31512=CARTESIAN_POINT('Ctrl Pts',(0.217459005539878,-1.57604331226605,
-2.47186352960145));
#31513=CARTESIAN_POINT('Ctrl Pts',(0.776496300339425,-1.44190782037182,
-2.45534243468637));
#31514=CARTESIAN_POINT('Ctrl Pts',(1.42844800473285,-0.893763424640342,
-2.42662776775306));
#31515=CARTESIAN_POINT('Ctrl Pts',(1.68511325308991,0.0984259617408266,
-2.39477486791059));
#31516=CARTESIAN_POINT('Ctrl Pts',(1.32014717838681,1.05709924001896,-2.36169595100801));
#31517=CARTESIAN_POINT('Ctrl Pts',(0.465222197363385,1.62999898968955,-2.32909774949883));
#31518=CARTESIAN_POINT('Ctrl Pts',(-0.392582646808871,1.60464250160246,
-2.30166701854538));
#31519=CARTESIAN_POINT('Ctrl Pts',(-0.977459806552233,1.29256118969725,
-2.2797668583326));
#31520=CARTESIAN_POINT('Ctrl Pts',(-1.32545625001454,0.933217602319048,
-2.26330236782603));
#31521=CARTESIAN_POINT('Ctrl Pts',(-1.54755282926423,0.48896150639208,-2.24685378788748));
#31522=CARTESIAN_POINT('Ctrl Pts',(-1.59831234300574,0.16375824267838,-2.23583746497264));
#31523=CARTESIAN_POINT('Ctrl Pts',(-1.59891715423784,-0.00421251370866319,
-2.23037046506263));
#31524=CARTESIAN_POINT('Ctrl Pts',(1.33274306951509,-0.00184287455380487,
-4.32188217182298));
#31525=CARTESIAN_POINT('Ctrl Pts',(1.33223133781691,0.140277436973989,-4.31725653492141));
#31526=CARTESIAN_POINT('Ctrl Pts',(1.2902720722241,0.409427197339747,-4.30814026546043));
#31527=CARTESIAN_POINT('Ctrl Pts',(1.10439696536374,0.78136050470156,-4.2943679341584));
#31528=CARTESIAN_POINT('Ctrl Pts',(0.813997842438886,1.08124532814599,-4.2806288618531));
#31529=CARTESIAN_POINT('Ctrl Pts',(0.325605208045794,1.34174117966905,-4.2623478198052));
#31530=CARTESIAN_POINT('Ctrl Pts',(-0.392266597046393,1.36343903424653,
-4.23936657717402));
#31531=CARTESIAN_POINT('Ctrl Pts',(-1.10832345882422,0.883510559025349,
-4.21212017602054));
#31532=CARTESIAN_POINT('Ctrl Pts',(-1.41486627333154,0.0794127438512151,
-4.18425457896408));
#31533=CARTESIAN_POINT('Ctrl Pts',(-1.19925904010042,-0.754482629518558,
-4.15773774905943));
#31534=CARTESIAN_POINT('Ctrl Pts',(-0.650749262275713,-1.21597342884471,
-4.13311264221038));
#31535=CARTESIAN_POINT('Ctrl Pts',(-0.112464476894189,-1.3451927619508,
-4.11791636030752));
#31536=CARTESIAN_POINT('Ctrl Pts',(0.408485467307824,-1.30883153454265,
-4.0934966575388));
#31537=CARTESIAN_POINT('Ctrl Pts',(0.97640470620415,-0.999499127010158,
-4.06306058338671));
#31538=CARTESIAN_POINT('Ctrl Pts',(1.35371346551323,-0.343351752449513,
-4.02856921698522));
#31539=CARTESIAN_POINT('Ctrl Pts',(1.33608077413191,0.349832021978961,-3.99661215349609));
#31540=CARTESIAN_POINT('Ctrl Pts',(1.03474305668921,0.892501702089117,-3.9676835930086));
#31541=CARTESIAN_POINT('Ctrl Pts',(0.591711345291201,1.23208009188755,-3.94161859350766));
#31542=CARTESIAN_POINT('Ctrl Pts',(0.0494704427508984,1.36622525558619,
-3.91554324711629));
#31543=CARTESIAN_POINT('Ctrl Pts',(-0.501185464467529,1.27217962308601,
-3.88947074773056));
#31544=CARTESIAN_POINT('Ctrl Pts',(-0.968441061163108,0.965813607757558,
-3.86338487895064));
#31545=CARTESIAN_POINT('Ctrl Pts',(-1.27435653987324,0.497981225383389,
-3.83729470829645));
#31546=CARTESIAN_POINT('Ctrl Pts',(-1.35202798814577,0.0385876101327993,
-3.81554266612973));
#31547=CARTESIAN_POINT('Ctrl Pts',(-1.3002933910548,-0.324722717286434,
-3.79813785235368));
#31548=CARTESIAN_POINT('Ctrl Pts',(-1.17582795675783,-0.670043044415297,
-3.78072900484704));
#31549=CARTESIAN_POINT('Ctrl Pts',(-0.89187979869532,-1.03986513675978,
-3.75895910935149));
#31550=CARTESIAN_POINT('Ctrl Pts',(-0.401602327156241,-1.31055280712498,
-3.73282284913628));
#31551=CARTESIAN_POINT('Ctrl Pts',(0.155958366856248,-1.36240893590434,
-3.70667247880376));
#31552=CARTESIAN_POINT('Ctrl Pts',(0.747921537864027,-1.16810540292178,
-3.67759847337626));
#31553=CARTESIAN_POINT('Ctrl Pts',(1.23417588205323,-0.66901461612135,-3.64559460713661));
#31554=CARTESIAN_POINT('Ctrl Pts',(1.37530120465285,-0.0508038734447465,
-3.61647247222503));
#31555=CARTESIAN_POINT('Ctrl Pts',(1.28250774044461,0.434054084292527,-3.59315698123624));
#31556=CARTESIAN_POINT('Ctrl Pts',(1.06322527327332,0.876535608048439,-3.56983009646951));
#31557=CARTESIAN_POINT('Ctrl Pts',(0.576461744420599,1.28506020436211,-3.54064402683342));
#31558=CARTESIAN_POINT('Ctrl Pts',(-0.17856418654777,1.39900778239141,-3.50558326489951));
#31559=CARTESIAN_POINT('Ctrl Pts',(-0.883333366011173,1.10227489402814,
-3.47047628213641));
#31560=CARTESIAN_POINT('Ctrl Pts',(-1.33009571946298,0.480304216542129,
-3.43532259018841));
#31561=CARTESIAN_POINT('Ctrl Pts',(-1.3871497940757,-0.284071969407902,
-3.400120449005));
#31562=CARTESIAN_POINT('Ctrl Pts',(-1.03698097164857,-0.967464807651622,
-3.36486363385704));
#31563=CARTESIAN_POINT('Ctrl Pts',(-0.381019254282027,-1.36835922625891,
-3.3295520402089));
#31564=CARTESIAN_POINT('Ctrl Pts',(0.389481902092793,-1.36921541021497,
-3.29418330968172));
#31565=CARTESIAN_POINT('Ctrl Pts',(0.99252740309322,-0.999836303890874,
-3.26170597024635));
#31566=CARTESIAN_POINT('Ctrl Pts',(1.31925718593453,-0.457044062570797,
-3.23213556718674));
#31567=CARTESIAN_POINT('Ctrl Pts',(1.39408265408951,0.108809587769026,-3.20548497542942));
#31568=CARTESIAN_POINT('Ctrl Pts',(1.23592254623773,0.658265411917513,-3.17879700908046));
#31569=CARTESIAN_POINT('Ctrl Pts',(0.870829270178407,1.09922483787908,-3.1520701953278));
#31570=CARTESIAN_POINT('Ctrl Pts',(0.3590595432658,1.35782293568119,-3.1253036554442));
#31571=CARTESIAN_POINT('Ctrl Pts',(-0.214278054221324,1.39023954473062,
-3.09849630861867));
#31572=CARTESIAN_POINT('Ctrl Pts',(-0.753588776103895,1.19041365958991,
-3.07164723768404));
#31573=CARTESIAN_POINT('Ctrl Pts',(-1.16869614334255,0.79091857588073,-3.04475523338839));
#31574=CARTESIAN_POINT('Ctrl Pts',(-1.38973889931854,0.258015243465068,
-3.0178197887389));
#31575=CARTESIAN_POINT('Ctrl Pts',(-1.37939392416049,-0.320037143804488,
-2.99083883865735));
#31576=CARTESIAN_POINT('Ctrl Pts',(-1.13807569240459,-0.846049140219926,
-2.96381384874762));
#31577=CARTESIAN_POINT('Ctrl Pts',(-0.658226832417825,-1.27644576592453,
-2.93373256101117));
#31578=CARTESIAN_POINT('Ctrl Pts',(0.0412819538892306,-1.45498650097557,
-2.90057659370659));
#31579=CARTESIAN_POINT('Ctrl Pts',(0.670130684154375,-1.26174671522835,
-2.87036221549118));
#31580=CARTESIAN_POINT('Ctrl Pts',(1.05852260489413,-0.926906152284757,
-2.84614667670633));
#31581=CARTESIAN_POINT('Ctrl Pts',(1.27183260914496,-0.606478431066315,
-2.82796258395378));
#31582=CARTESIAN_POINT('Ctrl Pts',(1.38999725539795,-0.239618169544361,
-2.80975639288988));
#31583=CARTESIAN_POINT('Ctrl Pts',(1.41039635928432,0.274677801973151,-2.78544881465415));
#31584=CARTESIAN_POINT('Ctrl Pts',(1.16873795631116,0.891852165624323,-2.75501303859493));
#31585=CARTESIAN_POINT('Ctrl Pts',(0.586622638095276,1.33397028424145,-2.72143197804221));
#31586=CARTESIAN_POINT('Ctrl Pts',(-0.0596281256868166,1.44364111061832,
-2.69086336929062));
#31587=CARTESIAN_POINT('Ctrl Pts',(-0.633235989998081,1.3022324586094,-2.66322875649725));
#31588=CARTESIAN_POINT('Ctrl Pts',(-1.10328636165357,0.942095047700372,
-2.63568453117449));
#31589=CARTESIAN_POINT('Ctrl Pts',(-1.39079426918394,0.423121775306233,
-2.60780030435273));
#31590=CARTESIAN_POINT('Ctrl Pts',(-1.4470391517022,-0.168622442050105,
-2.5803875186506));
#31591=CARTESIAN_POINT('Ctrl Pts',(-1.26122050903116,-0.734959886532534,
-2.55195681738039));
#31592=CARTESIAN_POINT('Ctrl Pts',(-0.864561437950006,-1.18011215245744,
-2.5250324432996));
#31593=CARTESIAN_POINT('Ctrl Pts',(-0.43303465558965,-1.37863126059473,
-2.50196116010659));
#31594=CARTESIAN_POINT('Ctrl Pts',(-0.0948241190351269,-1.42885069567028,
-2.48524012798101));
#31595=CARTESIAN_POINT('Ctrl Pts',(0.197430191428771,-1.42716228900735,
-2.47362609443607));
#31596=CARTESIAN_POINT('Ctrl Pts',(0.703761336166771,-1.30567723138343,
-2.45866246090041));
#31597=CARTESIAN_POINT('Ctrl Pts',(1.29440166462931,-0.809154737860619,
-2.43264970036145));
#31598=CARTESIAN_POINT('Ctrl Pts',(1.52702131467381,0.0899263703634786,
-2.40378749618235));
#31599=CARTESIAN_POINT('Ctrl Pts',(1.19621045642616,0.958876843822858,-2.37380181641756));
#31600=CARTESIAN_POINT('Ctrl Pts',(0.421100880351963,1.47853570405988,-2.34424608305228));
#31601=CARTESIAN_POINT('Ctrl Pts',(-0.357252438672992,1.45540691718553,
-2.31935534673135));
#31602=CARTESIAN_POINT('Ctrl Pts',(-0.887864026428122,1.17236987553731,
-2.29948793573597));
#31603=CARTESIAN_POINT('Ctrl Pts',(-1.2036269552239,0.846331645317162,-2.2845505972963));
#31604=CARTESIAN_POINT('Ctrl Pts',(-1.40562203409675,0.442258134242617,
-2.26958820164171));
#31605=CARTESIAN_POINT('Ctrl Pts',(-1.45149398156005,0.148118824010667,
-2.25962526863212));
#31606=CARTESIAN_POINT('Ctrl Pts',(-1.45204722659375,-0.00553074769862531,
-2.25462438506895));
#31607=CARTESIAN_POINT('Ctrl Pts',(1.42546076165175,-0.00530765277766144,
-4.20517133738338));
#31608=CARTESIAN_POINT('Ctrl Pts',(1.42491678471702,0.145767943482143,-4.20025422986036));
#31609=CARTESIAN_POINT('Ctrl Pts',(1.37993316537481,0.434308395373396,-4.19048113022102));
#31610=CARTESIAN_POINT('Ctrl Pts',(1.18155428429257,0.831168970214002,-4.17578689139102));
#31611=CARTESIAN_POINT('Ctrl Pts',(0.871544594210684,1.15127228944573,-4.16112003380017));
#31612=CARTESIAN_POINT('Ctrl Pts',(0.350551640194094,1.42916686330045,-4.14161998154656));
#31613=CARTESIAN_POINT('Ctrl Pts',(-0.413792109055743,1.45192144808262,
-4.11715319952602));
#31614=CARTESIAN_POINT('Ctrl Pts',(-1.17508330496538,0.941562236530219,
-4.08818474624585));
#31615=CARTESIAN_POINT('Ctrl Pts',(-1.49995829515209,0.0880210153638399,
-4.05861391303029));
#31616=CARTESIAN_POINT('Ctrl Pts',(-1.27166052210779,-0.795183444245264,
-4.03052951567407));
#31617=CARTESIAN_POINT('Ctrl Pts',(-0.690950520898828,-1.28317112464393,
-4.00448330152644));
#31618=CARTESIAN_POINT('Ctrl Pts',(-0.12294966963944,-1.41942987376945,
-3.98844212011088));
#31619=CARTESIAN_POINT('Ctrl Pts',(0.423496713647097,-1.38120666781861,
-3.96281661468422));
#31620=CARTESIAN_POINT('Ctrl Pts',(1.02300739912064,-1.0551451702216,-3.9307007006121));
#31621=CARTESIAN_POINT('Ctrl Pts',(1.41823975399121,-0.366076115830013,
-3.89451447899854));
#31622=CARTESIAN_POINT('Ctrl Pts',(1.39991931769537,0.360157039366418,-3.86102140976031));
#31623=CARTESIAN_POINT('Ctrl Pts',(1.08467609641392,0.927204409436556,-3.83079718639467));
#31624=CARTESIAN_POINT('Ctrl Pts',(0.622524980372356,1.28135687324873,-3.80360683546856));
#31625=CARTESIAN_POINT('Ctrl Pts',(0.0578874714694361,1.42090945106581,
-3.77645990760956));
#31626=CARTESIAN_POINT('Ctrl Pts',(-0.514223733569828,1.32307218876302,
-3.74937178821944));
#31627=CARTESIAN_POINT('Ctrl Pts',(-0.998714825490126,1.00527734669232,
-3.72232273145444));
#31628=CARTESIAN_POINT('Ctrl Pts',(-1.31519899241595,0.521043028789481,
-3.69532359157212));
#31629=CARTESIAN_POINT('Ctrl Pts',(-1.39531790201036,0.0465799073644213,
-3.67286064065657));
#31630=CARTESIAN_POINT('Ctrl Pts',(-1.34194411349281,-0.328091257034254,
-3.65491191111958));
#31631=CARTESIAN_POINT('Ctrl Pts',(-1.21369685084282,-0.683847300971654,
-3.63697744151664));
#31632=CARTESIAN_POINT('Ctrl Pts',(-0.921567460626822,-1.06416207336965,
-3.61458827224222));
#31633=CARTESIAN_POINT('Ctrl Pts',(-0.418267744270508,-1.34190400597337,
-3.58776279660469));
#31634=CARTESIAN_POINT('Ctrl Pts',(0.15284737168046,-1.3948923755348,-3.56097876688141));
#31635=CARTESIAN_POINT('Ctrl Pts',(0.75787751918564,-1.19616425763182,-3.53126429261728));
#31636=CARTESIAN_POINT('Ctrl Pts',(1.25347090588685,-0.68706525974854,-3.49863334111184));
#31637=CARTESIAN_POINT('Ctrl Pts',(1.39673252181696,-0.0584515547948913,
-3.46902548289891));
#31638=CARTESIAN_POINT('Ctrl Pts',(1.30253079349664,0.433452665070667,-3.44537162448077));
#31639=CARTESIAN_POINT('Ctrl Pts',(1.0803141186864,0.881753903034802,-3.42173818773312));
#31640=CARTESIAN_POINT('Ctrl Pts',(0.588097359665638,1.29451734211856,-3.39223897795944));
#31641=CARTESIAN_POINT('Ctrl Pts',(-0.173086256812962,1.40909830299405,
-3.35689534844021));
#31642=CARTESIAN_POINT('Ctrl Pts',(-0.881357490838906,1.11054942131824,
-3.32161122380991));
#31643=CARTESIAN_POINT('Ctrl Pts',(-1.32886706643363,0.487006580167841,
-3.28638134377501));
#31644=CARTESIAN_POINT('Ctrl Pts',(-1.38557808334009,-0.276926493197428,
-3.25120173340727));
#31645=CARTESIAN_POINT('Ctrl Pts',(-1.0363882630001,-0.957761324549181,
-3.21607364568651));
#31646=CARTESIAN_POINT('Ctrl Pts',(-0.384470557285378,-1.35581423463875,
-3.1809910035834));
#31647=CARTESIAN_POINT('Ctrl Pts',(0.378931861892865,-1.35637916104331,
-3.14595073219316));
#31648=CARTESIAN_POINT('Ctrl Pts',(0.974522766535925,-0.991220571877725,
-3.11386844951284));
#31649=CARTESIAN_POINT('Ctrl Pts',(1.29639097284273,-0.456264431544534,
-3.08472938251996));
#31650=CARTESIAN_POINT('Ctrl Pts',(1.36984281760244,0.100180562872646,-3.05852510329464));
#31651=CARTESIAN_POINT('Ctrl Pts',(1.21453148877589,0.639300308820662,-3.03233905402033));
#31652=CARTESIAN_POINT('Ctrl Pts',(0.856945441307693,1.07099928129219,-3.00617072299088));
#31653=CARTESIAN_POINT('Ctrl Pts',(0.356833095406517,1.32357019965779,-2.98001846012586));
#31654=CARTESIAN_POINT('Ctrl Pts',(-0.202218051140845,1.35505852042893,
-2.95388132800849));
#31655=CARTESIAN_POINT('Ctrl Pts',(-0.726946582754659,1.16050631432679,
-2.9277577739672));
#31656=CARTESIAN_POINT('Ctrl Pts',(-1.1299465441325,0.772502868173686,-2.90164700667616));
#31657=CARTESIAN_POINT('Ctrl Pts',(-1.34403191669268,0.256050785853187,
-2.87554684471141));
#31658=CARTESIAN_POINT('Ctrl Pts',(-1.33391812362185,-0.302943109300097,
-2.84945805333028));
#31659=CARTESIAN_POINT('Ctrl Pts',(-1.10089417653263,-0.810576208385297,
-2.8233749691623));
#31660=CARTESIAN_POINT('Ctrl Pts',(-0.638648401405453,-1.22503333555387,
-2.79440524878434));
#31661=CARTESIAN_POINT('Ctrl Pts',(0.0336164314160058,-1.39634316396761,
-2.76254512756927));
#31662=CARTESIAN_POINT('Ctrl Pts',(0.636267885288322,-1.21093971964553,
-2.73358845246346));
#31663=CARTESIAN_POINT('Ctrl Pts',(1.007759880785,-0.890596006587549,-2.71042533758501));
#31664=CARTESIAN_POINT('Ctrl Pts',(1.21153412552955,-0.584442304946323,
-2.69305317374889));
#31665=CARTESIAN_POINT('Ctrl Pts',(1.32424962304316,-0.234381274375833,
-2.67568185871626));
#31666=CARTESIAN_POINT('Ctrl Pts',(1.3436530953898,0.255742201160696,-2.65251890713377));
#31667=CARTESIAN_POINT('Ctrl Pts',(1.11357546301131,0.842698179974569,-2.62357045989763));
#31668=CARTESIAN_POINT('Ctrl Pts',(0.561090606358497,1.26205310456025,-2.59170793150652));
#31669=CARTESIAN_POINT('Ctrl Pts',(-0.0508352331085539,1.36575328346632,
-2.56276540366945));
#31670=CARTESIAN_POINT('Ctrl Pts',(-0.592973398636511,1.23202049926953,
-2.53664894408376));
#31671=CARTESIAN_POINT('Ctrl Pts',(-1.03644162056573,0.892081332980426,
-2.5106568633187));
#31672=CARTESIAN_POINT('Ctrl Pts',(-1.30718685521202,0.403259290541068,
-2.48439821792449));
#31673=CARTESIAN_POINT('Ctrl Pts',(-1.35991594860344,-0.153299990646814,
-2.45861400522989));
#31674=CARTESIAN_POINT('Ctrl Pts',(-1.18555928726333,-0.684735063431868,
-2.43194136639518));
#31675=CARTESIAN_POINT('Ctrl Pts',(-0.8132546917511,-1.10225590690569,-2.40667609365053));
#31676=CARTESIAN_POINT('Ctrl Pts',(-0.410343556007538,-1.28747626481981,
-2.38514102040768));
#31677=CARTESIAN_POINT('Ctrl Pts',(-0.0933128311840905,-1.33466761419352,
-2.36946411351112));
#31678=CARTESIAN_POINT('Ctrl Pts',(0.181125888445284,-1.33299774678052,
-2.35856079586863));
#31679=CARTESIAN_POINT('Ctrl Pts',(0.653791490249138,-1.21955477220406,
-2.34459674189696));
#31680=CARTESIAN_POINT('Ctrl Pts',(1.20414849306589,-0.756529297812768,
-2.32034780120738));
#31681=CARTESIAN_POINT('Ctrl Pts',(1.42067553810763,0.0806085523657789,
-2.29347807537358));
#31682=CARTESIAN_POINT('Ctrl Pts',(1.11285759072241,0.888214135289975,-2.26560569941744));
#31683=CARTESIAN_POINT('Ctrl Pts',(0.393419132618423,1.370470136021,-2.23817723786205));
#31684=CARTESIAN_POINT('Ctrl Pts',(-0.328107222499164,1.34873389309867,
-2.21510443211576));
#31685=CARTESIAN_POINT('Ctrl Pts',(-0.819225865019777,1.08678750638048,
-2.19671571124849));
#31686=CARTESIAN_POINT('Ctrl Pts',(-1.11128135031818,0.785195716061891,
-2.18290075218618));
#31687=CARTESIAN_POINT('Ctrl Pts',(-1.29824655204404,0.41107491982986,-2.16904707212731));
#31688=CARTESIAN_POINT('Ctrl Pts',(-1.3404415250879,0.140232419653471,-2.1598744395522));
#31689=CARTESIAN_POINT('Ctrl Pts',(-1.34095616469068,-0.00269548703267205,
-2.15522251757602));
#31690=CARTESIAN_POINT('Ctrl Pts',(1.57441728237085,-0.00475882175917087,
-4.20555490878314));
#31691=CARTESIAN_POINT('Ctrl Pts',(1.57382104694255,0.160830226396227,-4.20016542712911));
#31692=CARTESIAN_POINT('Ctrl Pts',(1.52389433620377,0.480836487680276,-4.18932537087206));
#31693=CARTESIAN_POINT('Ctrl Pts',(1.30515998157577,0.918375631205172,-4.17312689334584));
#31694=CARTESIAN_POINT('Ctrl Pts',(0.962591725337778,1.27211015243739,-4.15691751004377));
#31695=CARTESIAN_POINT('Ctrl Pts',(0.386859917276029,1.57929111008162,-4.13536808842013));
#31696=CARTESIAN_POINT('Ctrl Pts',(-0.457385721719227,1.60423173067857,
-4.10834473833266));
#31697=CARTESIAN_POINT('Ctrl Pts',(-1.29867867696178,1.04045295771887,-4.07633236307808));
#31698=CARTESIAN_POINT('Ctrl Pts',(-1.65759157297858,0.0972318401616007,
-4.04365867882984));
#31699=CARTESIAN_POINT('Ctrl Pts',(-1.40535915011805,-0.878658956485217,
-4.01262510582776));
#31700=CARTESIAN_POINT('Ctrl Pts',(-0.76365245051989,-1.4178801751674,-3.98384488263533));
#31701=CARTESIAN_POINT('Ctrl Pts',(-0.13609330725123,-1.56840947170582,
-3.96612093503963));
#31702=CARTESIAN_POINT('Ctrl Pts',(0.467361043861925,-1.52619301427989,
-3.93782048116129));
#31703=CARTESIAN_POINT('Ctrl Pts',(1.12965724939298,-1.16599408387728,-3.9023405236412));
#31704=CARTESIAN_POINT('Ctrl Pts',(1.56602152108927,-0.405070446115325,
-3.86238346280934));
#31705=CARTESIAN_POINT('Ctrl Pts',(1.54577900864213,0.396653620287876,-3.82540733153194));
#31706=CARTESIAN_POINT('Ctrl Pts',(1.19784827952487,1.0224148314103,-3.79205256002208));
#31707=CARTESIAN_POINT('Ctrl Pts',(0.687987022616282,1.41310185049113,-3.76205514281994));
#31708=CARTESIAN_POINT('Ctrl Pts',(0.0652988913500439,1.56696985038245,
-3.7321173863171));
#31709=CARTESIAN_POINT('Ctrl Pts',(-0.565374176136498,1.4590868805882,-3.70225538850416));
#31710=CARTESIAN_POINT('Ctrl Pts',(-1.09920151379461,1.10888693229534,-3.67245008645755));
#31711=CARTESIAN_POINT('Ctrl Pts',(-1.44772778366656,0.5755650513305,-3.6427143272373));
#31712=CARTESIAN_POINT('Ctrl Pts',(-1.53588854207107,0.0532839053016955,
-3.61798686327434));
#31713=CARTESIAN_POINT('Ctrl Pts',(-1.47715703636958,-0.358947593017698,
-3.59823839277339));
#31714=CARTESIAN_POINT('Ctrl Pts',(-1.33608585602734,-0.750253882144961,
-3.57851135695625));
#31715=CARTESIAN_POINT('Ctrl Pts',(-1.01486531301105,-1.16838041624213,
-3.55389397218704));
#31716=CARTESIAN_POINT('Ctrl Pts',(-0.461841975369745,-1.47350276179219,
-3.5244185529707));
#31717=CARTESIAN_POINT('Ctrl Pts',(0.165241246410054,-1.53164105217326,
-3.49500902468416));
#31718=CARTESIAN_POINT('Ctrl Pts',(0.829065654552701,-1.31352985004596,
-3.46240462216341));
#31719=CARTESIAN_POINT('Ctrl Pts',(1.37225900810044,-0.75538743290293,-3.4266337605291));
#31720=CARTESIAN_POINT('Ctrl Pts',(1.52901259893303,-0.0670223596449696,
-3.39421187953474));
#31721=CARTESIAN_POINT('Ctrl Pts',(1.42593328942179,0.471128805235677,-3.36833269058636));
#31722=CARTESIAN_POINT('Ctrl Pts',(1.18294681660127,0.96127347508502,-3.34249244595469));
#31723=CARTESIAN_POINT('Ctrl Pts',(0.645152558547863,1.41209702090449,-3.31026398403709));
#31724=CARTESIAN_POINT('Ctrl Pts',(-0.185257230536811,1.53693202566853,
-3.27170662449143));
#31725=CARTESIAN_POINT('Ctrl Pts',(-0.956824533914112,1.21152432946623,
-3.23326407354796));
#31726=CARTESIAN_POINT('Ctrl Pts',(-1.44351220487384,0.533089995718998,
-3.19493637614729));
#31727=CARTESIAN_POINT('Ctrl Pts',(-1.50493990529097,-0.296700747515234,
-3.15672350641668));
#31728=CARTESIAN_POINT('Ctrl Pts',(-1.12605725802962,-1.03499330356064,
-3.11862311978851));
#31729=CARTESIAN_POINT('Ctrl Pts',(-0.420109128147001,-1.46582906237508,
-3.08063579956));
#31730=CARTESIAN_POINT('Ctrl Pts',(0.405019871121438,-1.46621440348742,
-3.04276070099534));
#31731=CARTESIAN_POINT('Ctrl Pts',(1.04753237367876,-1.07208721947632,-3.00814341308827));
#31732=CARTESIAN_POINT('Ctrl Pts',(1.39414809541201,-0.495776795432331,
-2.9767535852974));
#31733=CARTESIAN_POINT('Ctrl Pts',(1.47307655905306,0.102798097369403,-2.94856378184586));
#31734=CARTESIAN_POINT('Ctrl Pts',(1.30615908686342,0.681855117890808,-2.92043510027654));
#31735=CARTESIAN_POINT('Ctrl Pts',(0.922564785236653,1.1448063648757,-2.89236677996251));
#31736=CARTESIAN_POINT('Ctrl Pts',(0.386946304111455,1.41519990400736,-2.86435840991392));
#31737=CARTESIAN_POINT('Ctrl Pts',(-0.210822359191289,1.44876915553345,
-2.83640937479909));
#31738=CARTESIAN_POINT('Ctrl Pts',(-0.770966689462007,1.24097992849669,
-2.80851922712657));
#31739=CARTESIAN_POINT('Ctrl Pts',(-1.20042387811736,0.827353496504227,
-2.78068709373845));
#31740=CARTESIAN_POINT('Ctrl Pts',(-1.42813960270921,0.277769872489742,
-2.75291296719939));
#31741=CARTESIAN_POINT('Ctrl Pts',(-1.41727339448313,-0.316071267297309,
-2.72519479229085));
#31742=CARTESIAN_POINT('Ctrl Pts',(-1.17009004112573,-0.85433932467822,
-2.69753499960645));
#31743=CARTESIAN_POINT('Ctrl Pts',(-0.680601408236679,-1.2930213408344,
-2.66686129038018));
#31744=CARTESIAN_POINT('Ctrl Pts',(0.0296769378175122,-1.4737959396875,
-2.63320025147592));
#31745=CARTESIAN_POINT('Ctrl Pts',(0.664787577307854,-1.2781518322714,-2.60267843039133));
#31746=CARTESIAN_POINT('Ctrl Pts',(1.05557427000303,-0.941121519830643,
-2.57830843402094));
#31747=CARTESIAN_POINT('Ctrl Pts',(1.26965186401621,-0.619418917470924,
-2.56005427954324));
#31748=CARTESIAN_POINT('Ctrl Pts',(1.38790872959175,-0.252058453272585,
-2.54182372891326));
#31749=CARTESIAN_POINT('Ctrl Pts',(1.40818671885242,0.261657220706895,-2.51754455036367));
#31750=CARTESIAN_POINT('Ctrl Pts',(1.16730350603785,0.875619151982967,-2.48725804038439));
#31751=CARTESIAN_POINT('Ctrl Pts',(0.59065049556,1.31296285283833,-2.45401003554107));
#31752=CARTESIAN_POINT('Ctrl Pts',(-0.0464288866481118,1.42080548531835,
-2.42387439318964));
#31753=CARTESIAN_POINT('Ctrl Pts',(-0.609707723834696,1.28173853674385,
-2.39673722570843));
#31754=CARTESIAN_POINT('Ctrl Pts',(-1.06945689724283,0.929144114286014,
-2.36978219725697));
#31755=CARTESIAN_POINT('Ctrl Pts',(-1.34955685669284,0.42327905257989,-2.3426113838214));
#31756=CARTESIAN_POINT('Ctrl Pts',(-1.40380914218791,-0.151670211794406,
-2.31596897050105));
#31757=CARTESIAN_POINT('Ctrl Pts',(-1.22422606355349,-0.699096895131267,
-2.28849786355966));
#31758=CARTESIAN_POINT('Ctrl Pts',(-0.840591520559868,-1.12894210887443,
-2.26246759589968));
#31759=CARTESIAN_POINT('Ctrl Pts',(-0.428235892457692,-1.31834260254916,
-2.24043266848866));
#31760=CARTESIAN_POINT('Ctrl Pts',(-0.102146798812591,-1.36704794478444,
-2.22430320026236));
#31761=CARTESIAN_POINT('Ctrl Pts',(0.180846350600063,-1.36521149131664,
-2.21306317611664));
#31762=CARTESIAN_POINT('Ctrl Pts',(0.664454998342927,-1.2490959498437,-2.19877907084499));
#31763=CARTESIAN_POINT('Ctrl Pts',(1.22624897429462,-0.775934691994764,
-2.17400695093128));
#31764=CARTESIAN_POINT('Ctrl Pts',(1.44687003037503,0.0775045360740113,
-2.14661308652914));
#31765=CARTESIAN_POINT('Ctrl Pts',(1.13340694971711,0.898760021455017,-2.11826252462912));
#31766=CARTESIAN_POINT('Ctrl Pts',(0.403206857004132,1.38786931881886,-2.09042681193968));
#31767=CARTESIAN_POINT('Ctrl Pts',(-0.32737568430479,1.36560820478861,-2.06706160097662));
#31768=CARTESIAN_POINT('Ctrl Pts',(-0.82372998777544,1.10080520427326,-2.04847494658758));
#31769=CARTESIAN_POINT('Ctrl Pts',(-1.11861986291797,0.79623547986047,-2.03452387002307));
#31770=CARTESIAN_POINT('Ctrl Pts',(-1.30704892942855,0.419117638021289,
-2.02055942174402));
#31771=CARTESIAN_POINT('Ctrl Pts',(-1.34962126675225,0.146088642239538,
-2.0113116407006));
#31772=CARTESIAN_POINT('Ctrl Pts',(-1.35013945947752,0.00217394721176147,
-2.00662760139703));
#31773=CARTESIAN_POINT('Ctrl Pts',(1.66767056912729,-0.000642017226719769,
-4.32172504735902));
#31774=CARTESIAN_POINT('Ctrl Pts',(1.66704137074608,0.174101642915884,-4.31603760751327));
#31775=CARTESIAN_POINT('Ctrl Pts',(1.61396148033041,0.513998779793965,-4.30452227032905));
#31776=CARTESIAN_POINT('Ctrl Pts',(1.3823231309458,0.977381813422264,-4.28736816567594));
#31777=CARTESIAN_POINT('Ctrl Pts',(1.0187270628173,1.35287697793601,-4.27016111559797));
#31778=CARTESIAN_POINT('Ctrl Pts',(0.407282097129691,1.67921088591362,-4.2472729970449));
#31779=CARTESIAN_POINT('Ctrl Pts',(-0.490224177097036,1.70583634833358,
-4.21854378626941));
#31780=CARTESIAN_POINT('Ctrl Pts',(-1.38612305014723,1.10583080364825,-4.18445474003016));
#31781=CARTESIAN_POINT('Ctrl Pts',(-1.76918891341576,0.10015298243074,-4.14961437587636));
#31782=CARTESIAN_POINT('Ctrl Pts',(-1.49979119562877,-0.942078102670249,
-4.1164687536911));
#31783=CARTESIAN_POINT('Ctrl Pts',(-0.814195262826672,-1.51872809084673,
-4.08569913393494));
#31784=CARTESIAN_POINT('Ctrl Pts',(-0.142049463935964,-1.68002727973188,
-4.06672107646415));
#31785=CARTESIAN_POINT('Ctrl Pts',(0.507025639203875,-1.63469298371086,
-4.0362894700067));
#31786=CARTESIAN_POINT('Ctrl Pts',(1.21604512412555,-1.24866425143607,-3.99829501018615));
#31787=CARTESIAN_POINT('Ctrl Pts',(1.68579278403846,-0.431030856387725,
-3.955329441603));
#31788=CARTESIAN_POINT('Ctrl Pts',(1.66385557197735,0.431794240343084,-3.91554634111577));
#31789=CARTESIAN_POINT('Ctrl Pts',(1.28907716480298,1.10639395357867,-3.87958490606665));
#31790=CARTESIAN_POINT('Ctrl Pts',(0.738851377208214,1.52806612434031,-3.84721380241475));
#31791=CARTESIAN_POINT('Ctrl Pts',(0.0661622682049421,1.69438919204168,
-3.81486774991119));
#31792=CARTESIAN_POINT('Ctrl Pts',(-0.616052772511665,1.5777818830296,-3.78256539435748));
#31793=CARTESIAN_POINT('Ctrl Pts',(-1.19415530829946,1.19862620912885,-3.7502887861161));
#31794=CARTESIAN_POINT('Ctrl Pts',(-1.57205496953799,0.620518762079344,
-3.71805226111082));
#31795=CARTESIAN_POINT('Ctrl Pts',(-1.66779537720002,0.0537257236388898,
-3.69121580691083));
#31796=CARTESIAN_POINT('Ctrl Pts',(-1.60402429743041,-0.393980244119804,
-3.66976771840974));
#31797=CARTESIAN_POINT('Ctrl Pts',(-1.4507479604018,-0.819179962498136,
-3.64833182858519));
#31798=CARTESIAN_POINT('Ctrl Pts',(-1.10147601660805,-1.27392279763523,
-3.62155991068323));
#31799=CARTESIAN_POINT('Ctrl Pts',(-0.499520414491787,-1.60612504451686,
-3.58947384999649));
#31800=CARTESIAN_POINT('Ctrl Pts',(0.183740564834017,-1.66954417804101,
-3.55742862876955));
#31801=CARTESIAN_POINT('Ctrl Pts',(0.907739575347634,-1.4317423227012,-3.52186870049055));
#31802=CARTESIAN_POINT('Ctrl Pts',(1.50088512449773,-0.822485081018016,
-3.48281468467816));
#31803=CARTESIAN_POINT('Ctrl Pts',(1.67233660105827,-0.0701090324061639,
-3.44737620589621));
#31804=CARTESIAN_POINT('Ctrl Pts',(1.55960131068257,0.518603001360326,-3.41906570333355));
#31805=CARTESIAN_POINT('Ctrl Pts',(1.29367344519901,1.05507798675663,-3.39078305610274));
#31806=CARTESIAN_POINT('Ctrl Pts',(0.70464689250189,1.54900028873722,-3.35547910665054));
#31807=CARTESIAN_POINT('Ctrl Pts',(-0.205850321961123,1.6860000359595,-3.31320221883856));
#31808=CARTESIAN_POINT('Ctrl Pts',(-1.05269691843797,1.32897874669926,-3.27101092652693));
#31809=CARTESIAN_POINT('Ctrl Pts',(-1.58740406658215,0.583802887696571,
-3.2289089373416));
#31810=CARTESIAN_POINT('Ctrl Pts',(-1.65503960428557,-0.328442529779849,
-3.18689851586196));
#31811=CARTESIAN_POINT('Ctrl Pts',(-1.23827554083022,-1.14076816918272,
-3.14498017094276));
#31812=CARTESIAN_POINT('Ctrl Pts',(-0.461083528427763,-1.61518777248162,
-3.10315676474998));
#31813=CARTESIAN_POINT('Ctrl Pts',(0.447958090773294,-1.61569817471631,
-3.06143035596376));
#31814=CARTESIAN_POINT('Ctrl Pts',(1.15625697096653,-1.18129145663195,-3.02327078103035));
#31815=CARTESIAN_POINT('Ctrl Pts',(1.5385483947366,-0.545732429710449,-2.98865340270468));
#31816=CARTESIAN_POINT('Ctrl Pts',(1.62564928333117,0.114622962233726,-2.95755433957182));
#31817=CARTESIAN_POINT('Ctrl Pts',(1.44146873106163,0.75365983619543,-2.92651289356067));
#31818=CARTESIAN_POINT('Ctrl Pts',(1.01804401786004,1.26471542389246,-2.89552948842941));
#31819=CARTESIAN_POINT('Ctrl Pts',(0.426652198015164,1.56328680486315,-2.86460483166852));
#31820=CARTESIAN_POINT('Ctrl Pts',(-0.233506697337365,1.60037716016785,
-2.8337394357706));
#31821=CARTESIAN_POINT('Ctrl Pts',(-0.852223154769246,1.37087508639121,
-2.80293386593878));
#31822=CARTESIAN_POINT('Ctrl Pts',(-1.32665537063582,0.913951584283742,
-2.77218870761467));
#31823=CARTESIAN_POINT('Ctrl Pts',(-1.57824191563113,0.306770803570071,
-2.74150432467094));
#31824=CARTESIAN_POINT('Ctrl Pts',(-1.56625075181747,-0.349333715748526,
-2.71088155852775));
#31825=CARTESIAN_POINT('Ctrl Pts',(-1.29312932697022,-0.944069321172231,
-2.68032007848504));
#31826=CARTESIAN_POINT('Ctrl Pts',(-0.752337350493662,-1.42875332810076,
-2.64643273964627));
#31827=CARTESIAN_POINT('Ctrl Pts',(0.0323708011696732,-1.62844696738958,
-2.60924549419053));
#31828=CARTESIAN_POINT('Ctrl Pts',(0.733911033259907,-1.41233998754078,
-2.57553270735194));
#31829=CARTESIAN_POINT('Ctrl Pts',(1.16549836573762,-1.04010955882194,-2.54861902978767));
#31830=CARTESIAN_POINT('Ctrl Pts',(1.40190416964634,-0.684856361734514,
-2.52846178585523));
#31831=CARTESIAN_POINT('Ctrl Pts',(1.53246914275855,-0.279241252768065,
-2.5083335304625));
#31832=CARTESIAN_POINT('Ctrl Pts',(1.55485929835845,0.287871240875836,-2.48153218805104));
#31833=CARTESIAN_POINT('Ctrl Pts',(1.2889653761743,0.965432901351441,-2.4481085910331));
#31834=CARTESIAN_POINT('Ctrl Pts',(0.65280735996725,1.44787419907493,-2.41143248159939));
#31835=CARTESIAN_POINT('Ctrl Pts',(-0.0496709907156844,1.56673997752695,
-2.37820546358285));
#31836=CARTESIAN_POINT('Ctrl Pts',(-0.670496836366765,1.4134565877183,-2.3482982885944));
#31837=CARTESIAN_POINT('Ctrl Pts',(-1.17699485748593,1.02494445873048,-2.31860068450517));
#31838=CARTESIAN_POINT('Ctrl Pts',(-1.48540922041371,0.467939880309279,
-2.28868623368794));
#31839=CARTESIAN_POINT('Ctrl Pts',(-1.54504707669121,-0.164866028014098,
-2.25936310649287));
#31840=CARTESIAN_POINT('Ctrl Pts',(-1.34758547808486,-0.766865278693161,
-2.22915760524));
#31841=CARTESIAN_POINT('Ctrl Pts',(-0.925619034963152,-1.23950709454415,
-2.20053050227581));
#31842=CARTESIAN_POINT('Ctrl Pts',(-0.47312689178265,-1.44727688910323,
-2.17635467666706));
#31843=CARTESIAN_POINT('Ctrl Pts',(-0.114624145491398,-1.50088266906923,
-2.15862063519408));
#31844=CARTESIAN_POINT('Ctrl Pts',(0.196793771251874,-1.49882011045581,
-2.14625337353289));
#31845=CARTESIAN_POINT('Ctrl Pts',(0.727540895785712,-1.37137349650026,
-2.13057991784179));
#31846=CARTESIAN_POINT('Ctrl Pts',(1.34350840501744,-0.852377020041632,
-2.10341642675301));
#31847=CARTESIAN_POINT('Ctrl Pts',(1.58522614346538,0.0829234946853341,
-2.07339634995277));
#31848=CARTESIAN_POINT('Ctrl Pts',(1.24189990551023,0.982145057415046,-2.04235987875837));
#31849=CARTESIAN_POINT('Ctrl Pts',(0.442964648689932,1.51696223459205,-2.01190849767654));
#31850=CARTESIAN_POINT('Ctrl Pts',(-0.355194757524547,1.49271901522222,
-1.98638599026986));
#31851=CARTESIAN_POINT('Ctrl Pts',(-0.89738743125439,1.20335711287795,-1.96608245344542));
#31852=CARTESIAN_POINT('Ctrl Pts',(-1.21934525660176,0.870788494252831,
-1.95084901288334));
#31853=CARTESIAN_POINT('Ctrl Pts',(-1.42451679199023,0.460127356714556,
-1.93564500481867));
#31854=CARTESIAN_POINT('Ctrl Pts',(-1.47111624563833,0.161276097580042,
-1.92552253081718));
#31855=CARTESIAN_POINT('Ctrl Pts',(-1.47167744855541,0.00541642853791316,
-1.92044971448322));
#31856=CARTESIAN_POINT('Ctrl Pts',(1.63403212256144,0.00396518640864409,
-4.46700040934992));
#31857=CARTESIAN_POINT('Ctrl Pts',(1.633414152876,0.175590365230348,-4.46141446774971));
#31858=CARTESIAN_POINT('Ctrl Pts',(1.58144489680089,0.508631329729613,-4.45013247933363));
#31859=CARTESIAN_POINT('Ctrl Pts',(1.35418050198765,0.963402541592023,-4.43329826263773));
#31860=CARTESIAN_POINT('Ctrl Pts',(0.997092638581031,1.33223572067097,-4.41639895348265));
#31861=CARTESIAN_POINT('Ctrl Pts',(0.396055854287184,1.6530578269441,-4.39389982100857));
#31862=CARTESIAN_POINT('Ctrl Pts',(-0.487453571014309,1.67953391279076,
-4.36562210287137));
#31863=CARTESIAN_POINT('Ctrl Pts',(-1.37107502680974,1.08800919403189,-4.33200538919037));
#31864=CARTESIAN_POINT('Ctrl Pts',(-1.75003909866722,0.0945250095421055,
-4.29758683406486));
#31865=CARTESIAN_POINT('Ctrl Pts',(-1.48325802053995,-0.937337267150294,
-4.26477411104859));
#31866=CARTESIAN_POINT('Ctrl Pts',(-0.804242501024566,-1.50915141701246,
-4.23427743771177));
#31867=CARTESIAN_POINT('Ctrl Pts',(-0.136252735175991,-1.66956614079881,
-4.21542680409255));
#31868=CARTESIAN_POINT('Ctrl Pts',(0.512509777066478,-1.62433935829672,
-4.18502241042396));
#31869=CARTESIAN_POINT('Ctrl Pts',(1.21666653808731,-1.24045434008153,-4.14728096812073));
#31870=CARTESIAN_POINT('Ctrl Pts',(1.68673889866034,-0.42419747492223,-4.1043501154818));
#31871=CARTESIAN_POINT('Ctrl Pts',(1.66463397769277,0.439031814106804,-4.06456655210986));
#31872=CARTESIAN_POINT('Ctrl Pts',(1.28918472074749,1.11554897429905,-4.02850284801316));
#31873=CARTESIAN_POINT('Ctrl Pts',(0.736527490917053,1.53916271070452,-3.99599306584002));
#31874=CARTESIAN_POINT('Ctrl Pts',(0.0597192645547418,1.70665889578166,
-3.96344496434848));
#31875=CARTESIAN_POINT('Ctrl Pts',(-0.62794703823877,1.58923892015398,-3.93088864416245));
#31876=CARTESIAN_POINT('Ctrl Pts',(-1.21173532891019,1.20650455789826,-3.89829917046084));
#31877=CARTESIAN_POINT('Ctrl Pts',(-1.59408295564238,0.621810298139683,
-3.86569345935932));
#31878=CARTESIAN_POINT('Ctrl Pts',(-1.69118658894133,0.0475258757840812,
-3.8385030380821));
#31879=CARTESIAN_POINT('Ctrl Pts',(-1.62649994211147,-0.406741823043796,
-3.81674141081092));
#31880=CARTESIAN_POINT('Ctrl Pts',(-1.47086327230883,-0.838547308822683,
-3.79497317393629));
#31881=CARTESIAN_POINT('Ctrl Pts',(-1.11580800536417,-1.30098277606591,
-3.76775322323976));
#31882=CARTESIAN_POINT('Ctrl Pts',(-0.502727993620926,-1.63947182863287,
-3.73507219388247));
#31883=CARTESIAN_POINT('Ctrl Pts',(0.194426113269872,-1.70429130667039,
-3.70237618329341));
#31884=CARTESIAN_POINT('Ctrl Pts',(0.934459323762974,-1.46137678148219,
-3.66603209917644));
#31885=CARTESIAN_POINT('Ctrl Pts',(1.54212626499169,-0.837565889576726,
-3.62603519928751));
#31886=CARTESIAN_POINT('Ctrl Pts',(1.71836542527733,-0.0653092002937604,
-3.58965833760839));
#31887=CARTESIAN_POINT('Ctrl Pts',(1.60248161771228,0.540059604623297,-3.56054876145131));
#31888=CARTESIAN_POINT('Ctrl Pts',(1.32877336422805,1.09233810609625,-3.53143388939476));
#31889=CARTESIAN_POINT('Ctrl Pts',(0.721562068605517,1.6018082509204,-3.49503283735083));
#31890=CARTESIAN_POINT('Ctrl Pts',(-0.219375445069418,1.74368689460065,
-3.451340537232));
#31891=CARTESIAN_POINT('Ctrl Pts',(-1.09661835982629,1.37415803608944,-3.40764136240512));
#31892=CARTESIAN_POINT('Ctrl Pts',(-1.65190763164543,0.600786199887819,
-3.36393787201356));
#31893=CARTESIAN_POINT('Ctrl Pts',(-1.7225493629562,-0.34824178044434,-3.3202332058754));
#31894=CARTESIAN_POINT('Ctrl Pts',(-1.28828245587157,-1.19528358601106,
-3.27653044626564));
#31895=CARTESIAN_POINT('Ctrl Pts',(-0.476392710097375,-1.69119687112247,
-3.23283283925704));
#31896=CARTESIAN_POINT('Ctrl Pts',(0.475412289608363,-1.69200841214036,
-3.18914326166888));
#31897=CARTESIAN_POINT('Ctrl Pts',(1.21873050036291,-1.23640649976984,-3.14910456666266));
#31898=CARTESIAN_POINT('Ctrl Pts',(1.62068706394748,-0.568391997078336,
-3.11271615020977));
#31899=CARTESIAN_POINT('Ctrl Pts',(1.71248714292806,0.126800675114135,-3.07997564707981));
#31900=CARTESIAN_POINT('Ctrl Pts',(1.51839160569328,0.800623065833593,-3.04724573761884));
#31901=CARTESIAN_POINT('Ctrl Pts',(1.07134132748941,1.34035514363526,-3.01452752981176));
#31902=CARTESIAN_POINT('Ctrl Pts',(0.445952950723967,1.65620521177943,-2.98182242827649));
#31903=CARTESIAN_POINT('Ctrl Pts',(-0.253235621616767,1.69558949724506,
-2.94913153234246));
#31904=CARTESIAN_POINT('Ctrl Pts',(-0.909531081339571,1.45225519765726,
-2.91645625461488));
#31905=CARTESIAN_POINT('Ctrl Pts',(-1.41354765304908,0.966974009737121,
-2.88379759749975));
#31906=CARTESIAN_POINT('Ctrl Pts',(-1.68125974445041,0.321135267881592,
-2.85115727605726));
#31907=CARTESIAN_POINT('Ctrl Pts',(-1.66857814222946,-0.377775811263314,
-2.81853548530576));
#31908=CARTESIAN_POINT('Ctrl Pts',(-1.37733100303391,-1.01221991954475,
-2.78593568804616));
#31909=CARTESIAN_POINT('Ctrl Pts',(-0.799731307240381,-1.53001994492261,
-2.74973597271145));
#31910=CARTESIAN_POINT('Ctrl Pts',(0.0397423073554164,-1.74387296836219,
-2.70995033892348));
#31911=CARTESIAN_POINT('Ctrl Pts',(0.791672052026611,-1.5124223123408,-2.67381718939549));
#31912=CARTESIAN_POINT('Ctrl Pts',(1.2548568142905,-1.11299176670312,-2.6449342586345));
#31913=CARTESIAN_POINT('Ctrl Pts',(1.50878301167248,-0.731448324033336,
-2.62328385326395));
#31914=CARTESIAN_POINT('Ctrl Pts',(1.6491603524909,-0.295437446030695,-2.60164646956971));
#31915=CARTESIAN_POINT('Ctrl Pts',(1.67327475040855,0.314684516226746,-2.57281079466485));
#31916=CARTESIAN_POINT('Ctrl Pts',(1.38702581105008,1.04462363319461,-2.53680591798736));
#31917=CARTESIAN_POINT('Ctrl Pts',(0.700764571894838,1.56526316414046,-2.4972337408036));
#31918=CARTESIAN_POINT('Ctrl Pts',(-0.0581917213931231,1.69379640831307,
-2.4613332982401));
#31919=CARTESIAN_POINT('Ctrl Pts',(-0.729733295442202,1.52804906535047,
-2.42898092007903));
#31920=CARTESIAN_POINT('Ctrl Pts',(-1.2782317500249,1.10745044146276,-2.39682477743175));
#31921=CARTESIAN_POINT('Ctrl Pts',(-1.61261796673324,0.503612684553527,
-2.3643904933464));
#31922=CARTESIAN_POINT('Ctrl Pts',(-1.67745533422548,-0.183031344035318,
-2.33257312444416));
#31923=CARTESIAN_POINT('Ctrl Pts',(-1.46287455872121,-0.837191718445536,
-2.29974535705945));
#31924=CARTESIAN_POINT('Ctrl Pts',(-1.00440147091468,-1.35094671104102,
-2.26863667244565));
#31925=CARTESIAN_POINT('Ctrl Pts',(-0.511166577563946,-1.57752630595462,
-2.24227873605543));
#31926=CARTESIAN_POINT('Ctrl Pts',(-0.121341981681085,-1.63572882933236,
-2.22299746469467));
#31927=CARTESIAN_POINT('Ctrl Pts',(0.216937568381371,-1.63355035713921,
-2.20956133114149));
#31928=CARTESIAN_POINT('Ctrl Pts',(0.795549791365443,-1.49463453149145,
-2.19247015083976));
#31929=CARTESIAN_POINT('Ctrl Pts',(1.46784754973028,-0.928439854007026,
-2.16282908058836));
#31930=CARTESIAN_POINT('Ctrl Pts',(1.73181203384054,0.0928136904787116,
-2.13004544067402));
#31931=CARTESIAN_POINT('Ctrl Pts',(1.35679704380804,1.07578258179391,-2.09612076196744));
#31932=CARTESIAN_POINT('Ctrl Pts',(0.4827459951358,1.6608517766393,-2.06280214834103));
#31933=CARTESIAN_POINT('Ctrl Pts',(-0.39100871803772,1.63458704965102,-2.03486072202743));
#31934=CARTESIAN_POINT('Ctrl Pts',(-0.985173173937378,1.31743448978772,
-2.01261038575294));
#31935=CARTESIAN_POINT('Ctrl Pts',(-1.33815367873876,0.952841687632227,
-1.99590730338613));
#31936=CARTESIAN_POINT('Ctrl Pts',(-1.56280887343282,0.503299446074766,
-1.97926439075081));
#31937=CARTESIAN_POINT('Ctrl Pts',(-1.61417743768913,0.174293206827452,
-1.96811869179015));
#31938=CARTESIAN_POINT('Ctrl Pts',(-1.61478859484591,0.00456003315652596,
-1.96259432990035));
#31939=CARTESIAN_POINT('Ctrl Pts',(1.54486203470619,0.00504105038853388,
-4.50992061443582));
#31940=CARTESIAN_POINT('Ctrl Pts',(1.54427529571177,0.167992708395013,-4.50461697279343));
#31941=CARTESIAN_POINT('Ctrl Pts',(1.4952334965929,0.482267292923238,-4.4939707520506));
#31942=CARTESIAN_POINT('Ctrl Pts',(1.280098125952,0.912812524518765,-4.47803220176687));
#31943=CARTESIAN_POINT('Ctrl Pts',(0.942266254010241,1.26176908060242,-4.46204447315161));
#31944=CARTESIAN_POINT('Ctrl Pts',(0.373481056552319,1.5653533290073,-4.44075200478145));
#31945=CARTESIAN_POINT('Ctrl Pts',(-0.463404247785094,1.59064712143174,
-4.41396463342408));
#31946=CARTESIAN_POINT('Ctrl Pts',(-1.30080065397219,1.03007856052102,-4.38210653434173));
#31947=CARTESIAN_POINT('Ctrl Pts',(-1.66044589527054,0.0879499473794728,
-4.34946171776996));
#31948=CARTESIAN_POINT('Ctrl Pts',(-1.40718897843239,-0.891504108835798,
-4.31831555008915));
#31949=CARTESIAN_POINT('Ctrl Pts',(-0.76257285222428,-1.43463924387864,
-4.28935167453691));
#31950=CARTESIAN_POINT('Ctrl Pts',(-0.127537178656397,-1.58719053169968,
-4.27143387847271));
#31951=CARTESIAN_POINT('Ctrl Pts',(0.490783544164864,-1.54412691424913,
-4.24246133751784));
#31952=CARTESIAN_POINT('Ctrl Pts',(1.16011254877525,-1.17901721909146,-4.20658115748246));
#31953=CARTESIAN_POINT('Ctrl Pts',(1.60839956049189,-0.401427769437864,
-4.16566702807252));
#31954=CARTESIAN_POINT('Ctrl Pts',(1.58726175515024,0.421750876894179,-4.12773560075408));
#31955=CARTESIAN_POINT('Ctrl Pts',(1.22901070732513,1.06761482142423,-4.09330500428777));
#31956=CARTESIAN_POINT('Ctrl Pts',(0.701012634421948,1.4723766837057,-4.06224619965589));
#31957=CARTESIAN_POINT('Ctrl Pts',(0.0538808968029187,1.63260191483167,
-4.03112301381928));
#31958=CARTESIAN_POINT('Ctrl Pts',(-0.604265655641256,1.52029339992018,
-3.99996509335409));
#31959=CARTESIAN_POINT('Ctrl Pts',(-1.16350103648761,1.15373453196215,-3.9687480484786));
#31960=CARTESIAN_POINT('Ctrl Pts',(-1.53013509440704,0.593198427290282,
-3.93748740632736));
#31961=CARTESIAN_POINT('Ctrl Pts',(-1.62337449866167,0.0421151334826504,
-3.91139521879784));
#31962=CARTESIAN_POINT('Ctrl Pts',(-1.56126900627456,-0.39411781117998,
-3.89049778782509));
#31963=CARTESIAN_POINT('Ctrl Pts',(-1.41175571186897,-0.808972539380072,
-3.86958433719094));
#31964=CARTESIAN_POINT('Ctrl Pts',(-1.07045540903568,-1.25359216931913,
-3.8434155366407));
#31965=CARTESIAN_POINT('Ctrl Pts',(-0.480515947183528,-1.57939238134504,
-3.8119666727399));
#31966=CARTESIAN_POINT('Ctrl Pts',(0.19100290161953,-1.64189675622309,-3.78047309491055));
#31967=CARTESIAN_POINT('Ctrl Pts',(0.904540049513209,-1.40777713332295,
-3.74543248330941));
#31968=CARTESIAN_POINT('Ctrl Pts',(1.49121694695292,-0.80572520337984,-3.70682471160733));
#31969=CARTESIAN_POINT('Ctrl Pts',(1.66171129304163,-0.0593325028595491,
-3.67166537676614));
#31970=CARTESIAN_POINT('Ctrl Pts',(1.5496167463837,0.526399295408366,-3.64350147770703));
#31971=CARTESIAN_POINT('Ctrl Pts',(1.28464063960639,1.0611311664764,-3.61531255256961));
#31972=CARTESIAN_POINT('Ctrl Pts',(0.696268858902054,1.55499203424871,-3.58003721182078));
#31973=CARTESIAN_POINT('Ctrl Pts',(-0.216920980436962,1.69287678092493,
-3.53763265470216));
#31974=CARTESIAN_POINT('Ctrl Pts',(-1.06955241283063,1.33391780047904,-3.49516506321254));
#31975=CARTESIAN_POINT('Ctrl Pts',(-1.61014220606482,0.581347239549756,
-3.45263319816296));
#31976=CARTESIAN_POINT('Ctrl Pts',(-1.67917373826321,-0.343620921298622,
-3.41003699377274));
#31977=CARTESIAN_POINT('Ctrl Pts',(-1.25550348658284,-1.17044583037604,
-3.36738575146504));
#31978=CARTESIAN_POINT('Ctrl Pts',(-0.462020640660321,-1.65532153402782,
-3.32467620708539));
#31979=CARTESIAN_POINT('Ctrl Pts',(0.469705448319077,-1.65634021328833,
-3.28191047946903));
#31980=CARTESIAN_POINT('Ctrl Pts',(1.19850015527152,-1.20982487444789,-3.24266160207414));
#31981=CARTESIAN_POINT('Ctrl Pts',(1.59317109062565,-0.554137583148034,
-3.20694338104645));
#31982=CARTESIAN_POINT('Ctrl Pts',(1.68346032775077,0.129027353549663,-3.17477150591299));
#31983=CARTESIAN_POINT('Ctrl Pts',(1.49259046599288,0.791977263040797,-3.14257297314195));
#31984=CARTESIAN_POINT('Ctrl Pts',(1.05233497259996,1.32363786938231,-3.11034993601051));
#31985=CARTESIAN_POINT('Ctrl Pts',(0.435701331628633,1.63516387116315,-3.07810298725901));
#31986=CARTESIAN_POINT('Ctrl Pts',(-0.254528938786086,1.67413199198048,
-3.04583353661053));
#31987=CARTESIAN_POINT('Ctrl Pts',(-0.903190199732295,1.43371965206946,
-3.01354225730577));
#31988=CARTESIAN_POINT('Ctrl Pts',(-1.40196135164732,0.953622409618861,
-2.98123117044023));
#31989=CARTESIAN_POINT('Ctrl Pts',(-1.6672295939013,0.3138788195484,-2.94889948881354));
#31990=CARTESIAN_POINT('Ctrl Pts',(-1.65476459871361,-0.379237401091453,
-2.91655275411879));
#31991=CARTESIAN_POINT('Ctrl Pts',(-1.36561533935134,-1.00925640253928,
-2.88418251158926));
#31992=CARTESIAN_POINT('Ctrl Pts',(-0.791580155685632,-1.52405179134768,
-2.84820516769771));
#31993=CARTESIAN_POINT('Ctrl Pts',(0.0440188697820079,-1.73707316808419,
-2.80860411869647));
#31994=CARTESIAN_POINT('Ctrl Pts',(0.793703939881436,-1.5065313997291,-2.7725852475833));
#31995=CARTESIAN_POINT('Ctrl Pts',(1.25604301727935,-1.10785808168577,-2.74375918621644));
#31996=CARTESIAN_POINT('Ctrl Pts',(1.50972654347214,-0.72674230304296,-2.72213354167433));
#31997=CARTESIAN_POINT('Ctrl Pts',(1.65008105202239,-0.290858305672986,
-2.70050394464286));
#31998=CARTESIAN_POINT('Ctrl Pts',(1.67426371947403,0.31954215732238,-2.67165783625169));
#31999=CARTESIAN_POINT('Ctrl Pts',(1.38767058671888,1.05071135347934,-2.63559821398635));
#32000=CARTESIAN_POINT('Ctrl Pts',(0.699340526719848,1.57321635116522,-2.5959018076405));
#32001=CARTESIAN_POINT('Ctrl Pts',(-0.0630631132721198,1.70239827801748,
-2.5598438057277));
#32002=CARTESIAN_POINT('Ctrl Pts',(-0.738459672332989,1.53580212731004,
-2.52731017136676));
#32003=CARTESIAN_POINT('Ctrl Pts',(-1.29085657604536,1.11232101894069,-2.49493239584644));
#32004=CARTESIAN_POINT('Ctrl Pts',(-1.62801909720545,0.50360740192754,-2.46223591640657));
#32005=CARTESIAN_POINT('Ctrl Pts',(-1.69359681981401,-0.189305516347992,
-2.43013459810603));
#32006=CARTESIAN_POINT('Ctrl Pts',(-1.47670396873442,-0.850502437605762,
-2.39695331495922));
#32007=CARTESIAN_POINT('Ctrl Pts',(-1.01336092382365,-1.36995827385155,
-2.36551397783944));
#32008=CARTESIAN_POINT('Ctrl Pts',(-0.513033351478244,-1.59989730603717,
-2.33877562827901));
#32009=CARTESIAN_POINT('Ctrl Pts',(-0.118638858821434,-1.65866879273177,
-2.3192717897149));
#32010=CARTESIAN_POINT('Ctrl Pts',(0.2231378134643,-1.65654474281072,-2.30569511174964));
#32011=CARTESIAN_POINT('Ctrl Pts',(0.810235746795052,-1.51562520417683,
-2.28835279734094));
#32012=CARTESIAN_POINT('Ctrl Pts',(1.49319309129472,-0.940792787098675,
-2.25825858954862));
#32013=CARTESIAN_POINT('Ctrl Pts',(1.76161999248799,0.0974220507406099,
-2.22493345911928));
#32014=CARTESIAN_POINT('Ctrl Pts',(1.38017223194885,1.09810710677196,-2.19040761292332));
#32015=CARTESIAN_POINT('Ctrl Pts',(0.489443651430728,1.6945190877625,-2.15645393542203));
#32016=CARTESIAN_POINT('Ctrl Pts',(-0.401928537350069,1.66796741397563,
-2.12795487297203));
#32017=CARTESIAN_POINT('Ctrl Pts',(-1.00884755318753,1.34402342569283,-2.10522879430255));
#32018=CARTESIAN_POINT('Ctrl Pts',(-1.36955730416376,0.971469379765492,
-2.08816145749317));
#32019=CARTESIAN_POINT('Ctrl Pts',(-1.59923321977339,0.511901403140453,
-2.07114854304999));
#32020=CARTESIAN_POINT('Ctrl Pts',(-1.65176416971881,0.175099526035226,
-2.05974032540467));
#32021=CARTESIAN_POINT('Ctrl Pts',(-1.65238846619436,0.00171724468601428,
-2.05409719479715));
#32022=CARTESIAN_POINT('Ctrl Pts',(1.49998243058588,0.00487945268456504,
-4.50992061443582));
#32023=CARTESIAN_POINT('Ctrl Pts',(1.49941141170999,0.163465252269264,-4.50475906983506));
#32024=CARTESIAN_POINT('Ctrl Pts',(1.45186405026655,0.468260659554012,-4.49443439156157));
#32025=CARTESIAN_POINT('Ctrl Pts',(1.24285849641208,0.886559230778761,-4.47894878298098));
#32026=CARTESIAN_POINT('Ctrl Pts',(0.914832037666938,1.22538627239788,-4.46342570918691));
#32027=CARTESIAN_POINT('Ctrl Pts',(0.362526476214984,1.52015190223001,-4.44275032349895));
#32028=CARTESIAN_POINT('Ctrl Pts',(-0.450285458827622,1.54477765231458,
-4.41673352060185));
#32029=CARTESIAN_POINT('Ctrl Pts',(-1.26358566414186,1.00029259499041,-4.38579230410963));
#32030=CARTESIAN_POINT('Ctrl Pts',(-1.61297063863451,0.0851696210599042,
-4.35408217822798));
#32031=CARTESIAN_POINT('Ctrl Pts',(-1.36691769149066,-0.86636719535778,
-4.32382427572184));
#32032=CARTESIAN_POINT('Ctrl Pts',(-0.740664712301201,-1.39406711347056,
-4.29568368658589));
#32033=CARTESIAN_POINT('Ctrl Pts',(-0.123568561445898,-1.54231629531191,
-4.27827259231965));
#32034=CARTESIAN_POINT('Ctrl Pts',(0.477570602247783,-1.50045464230821,
-4.25010620760684));
#32035=CARTESIAN_POINT('Ctrl Pts',(1.12799462557692,-1.14561364539286,-4.21523812123688));
#32036=CARTESIAN_POINT('Ctrl Pts',(1.56388513724472,-0.389673012803625,
-4.17546007003578));
#32037=CARTESIAN_POINT('Ctrl Pts',(1.5433188232119,0.410763669941787,-4.13857735821636));
#32038=CARTESIAN_POINT('Ctrl Pts',(1.19490853879333,1.03893941579882,-4.10508910882579));
#32039=CARTESIAN_POINT('Ctrl Pts',(0.681279880783051,1.43269210784687,-4.07487536403218));
#32040=CARTESIAN_POINT('Ctrl Pts',(0.051646821861207,1.58859643745763,-4.04459309324451));
#32041=CARTESIAN_POINT('Ctrl Pts',(-0.588862535961304,1.47930900476985,
-4.01426969238989));
#32042=CARTESIAN_POINT('Ctrl Pts',(-1.13322870809872,1.1225062752352,-3.98388228335323));
#32043=CARTESIAN_POINT('Ctrl Pts',(-1.4902067993283,0.576759659588736,-3.95344539501966));
#32044=CARTESIAN_POINT('Ctrl Pts',(-1.58102020223693,0.0400740757948976,
-3.92803411508518));
#32045=CARTESIAN_POINT('Ctrl Pts',(-1.52052962309553,-0.384828263720139,
-3.90767925424071));
#32046=CARTESIAN_POINT('Ctrl Pts',(-1.3748830928401,-0.788957250234775,
-3.88730621071591));
#32047=CARTESIAN_POINT('Ctrl Pts',(-1.0423371162911,-1.22218867468557,-3.86180720794638));
#32048=CARTESIAN_POINT('Ctrl Pts',(-0.467378790598492,-1.53972799805516,
-3.83115568482052));
#32049=CARTESIAN_POINT('Ctrl Pts',(0.187274531141039,-1.60068158914455,
-3.80045226057647));
#32050=CARTESIAN_POINT('Ctrl Pts',(0.883096272461548,-1.37238382842803,
-3.76628010013367));
#32051=CARTESIAN_POINT('Ctrl Pts',(1.45542862121288,-0.785128737057825,
-3.72861800828645));
#32052=CARTESIAN_POINT('Ctrl Pts',(1.62183852895481,-0.0567398924127903,
-3.69430530328978));
#32053=CARTESIAN_POINT('Ctrl Pts',(1.51242393883133,0.515046269014153,-3.66681113832745));
#32054=CARTESIAN_POINT('Ctrl Pts',(1.25371395215128,1.0371419048164,-3.63928782397711));
#32055=CARTESIAN_POINT('Ctrl Pts',(0.679041108905056,1.51956040430477,-3.60482953394523));
#32056=CARTESIAN_POINT('Ctrl Pts',(-0.213247562120534,1.65433450298338,
-3.56339447382386));
#32057=CARTESIAN_POINT('Ctrl Pts',(-1.04680323812526,1.30346814108,-3.52187569315801));
#32058=CARTESIAN_POINT('Ctrl Pts',(-1.57557751626781,0.567442201034068,
-3.48027478133792));
#32059=CARTESIAN_POINT('Ctrl Pts',(-1.64318830952972,-0.337637019006298,
-3.43859332018342));
#32060=CARTESIAN_POINT('Ctrl Pts',(-1.22844519515377,-1.14714492715669,
-3.39683307764518));
#32061=CARTESIAN_POINT('Ctrl Pts',(-0.451245980735406,-1.62215680765017,
-3.35499576544402));
#32062=CARTESIAN_POINT('Ctrl Pts',(0.461841974941765,-1.62319460304399,
-3.31308315566976));
#32063=CARTESIAN_POINT('Ctrl Pts',(1.17649440309474,-1.18543555842648,-3.27459582000513));
#32064=CARTESIAN_POINT('Ctrl Pts',(1.5636738872075,-0.54221871976191,-3.23955517618414));
#32065=CARTESIAN_POINT('Ctrl Pts',(1.65231581225766,0.128238780519003,-3.20797910267182));
#32066=CARTESIAN_POINT('Ctrl Pts',(1.46493973472583,0.779138006438161,-3.17636441807156));
#32067=CARTESIAN_POINT('Ctrl Pts',(1.03253139188493,1.30136595938992,-3.14471191495533));
#32068=CARTESIAN_POINT('Ctrl Pts',(0.426609970086491,1.60751024918497,-3.11302251069183));
#32069=CARTESIAN_POINT('Ctrl Pts',(-0.251933879032834,1.64584505089144,
-3.08129700553233));
#32070=CARTESIAN_POINT('Ctrl Pts',(-0.889905805470703,1.40942555957253,
-3.04953632759992));
#32071=CARTESIAN_POINT('Ctrl Pts',(-1.38068331350981,0.937053401938582,
-3.01774135131172));
#32072=CARTESIAN_POINT('Ctrl Pts',(-1.64184179716058,0.307317409087506,
-2.98591300518706));
#32073=CARTESIAN_POINT('Ctrl Pts',(-1.62957916709941,-0.37530803509689,
-2.95405221275351));
#32074=CARTESIAN_POINT('Ctrl Pts',(-1.34474730528677,-0.996034495385219,
-2.92215989404433));
#32075=CARTESIAN_POINT('Ctrl Pts',(-0.778879409529726,-1.50350912987896,
-2.88668999089474));
#32076=CARTESIAN_POINT('Ctrl Pts',(0.0452156959044932,-1.71370006437942,
-2.84763094470004));
#32077=CARTESIAN_POINT('Ctrl Pts',(0.785100365893931,-1.486208751186,-2.81208062847635));
#32078=CARTESIAN_POINT('Ctrl Pts',(1.24161679713701,-1.09259013745182,-2.7836165314676));
#32079=CARTESIAN_POINT('Ctrl Pts',(1.49217131201598,-0.716178712962469,
-2.76225639002869));
#32080=CARTESIAN_POINT('Ctrl Pts',(1.63085414425123,-0.285537734548898,
-2.7408855262812));
#32081=CARTESIAN_POINT('Ctrl Pts',(1.65475200752033,0.317728375257333,-2.7123738937245));
#32082=CARTESIAN_POINT('Ctrl Pts',(1.37145521865962,1.04076278423927,-2.67671479060714));
#32083=CARTESIAN_POINT('Ctrl Pts',(0.69041646931577,1.55777895441666,-2.63743464573646));
#32084=CARTESIAN_POINT('Ctrl Pts',(-0.0643948515707663,1.68574777587918,
-2.6017316079884));
#32085=CARTESIAN_POINT('Ctrl Pts',(-0.733422672005601,1.52073388540773,
-2.56950115646222));
#32086=CARTESIAN_POINT('Ctrl Pts',(-1.28085476582717,1.10113604465525,-2.53741554342871));
#32087=CARTESIAN_POINT('Ctrl Pts',(-1.61517951924605,0.4975562304161,-2.50499073603886));
#32088=CARTESIAN_POINT('Ctrl Pts',(-1.68029840248005,-0.189791143389858,
-2.47314557601871));
#32089=CARTESIAN_POINT('Ctrl Pts',(-1.46497737904047,-0.846156793246451,
-2.44020210847229));
#32090=CARTESIAN_POINT('Ctrl Pts',(-1.00508021286665,-1.36188270355857,
-2.40899190246463));
#32091=CARTESIAN_POINT('Ctrl Pts',(-0.507582321376923,-1.59058364540096,
-2.38240038156976));
#32092=CARTESIAN_POINT('Ctrl Pts',(-0.115985349294589,-1.64889286597431,
-2.36303576958252));
#32093=CARTESIAN_POINT('Ctrl Pts',(0.223158570335046,-1.64681924620263,
-2.349562123073));
#32094=CARTESIAN_POINT('Ctrl Pts',(0.806901355148856,-1.50671742388011,
-2.33231544041505));
#32095=CARTESIAN_POINT('Ctrl Pts',(1.48644477626825,-0.934917871941825,
-2.30237235343056));
#32096=CARTESIAN_POINT('Ctrl Pts',(1.75362331696032,0.0983401101520701,
-2.26920259215576));
#32097=CARTESIAN_POINT('Ctrl Pts',(1.37388207698597,1.09486845045221,-2.23481640537456));
#32098=CARTESIAN_POINT('Ctrl Pts',(0.486437491100621,1.68918937268853,-2.20098350021554));
#32099=CARTESIAN_POINT('Ctrl Pts',(-0.402275175720241,1.66276347810902,
-2.172565595614));
#32100=CARTESIAN_POINT('Ctrl Pts',(-1.0075498708897,1.33971834323449,-2.14990060001603));
#32101=CARTESIAN_POINT('Ctrl Pts',(-1.36740441992316,0.968073875003734,
-2.13287342310861));
#32102=CARTESIAN_POINT('Ctrl Pts',(-1.59664060478066,0.509453342147398,
-2.11589441486025));
#32103=CARTESIAN_POINT('Ctrl Pts',(-1.64911395659225,0.173292258411803,
-2.10450673116507));
#32104=CARTESIAN_POINT('Ctrl Pts',(-1.64973702763284,0.000250310089940127,
-2.09887467748946));
#32105=CARTESIAN_POINT('Ctrl Pts',(0.551250187536832,1.40171416652003,-4.45000670703013));
#32106=CARTESIAN_POINT('Ctrl Pts',(0.531806260700359,1.40940188459679,-4.44930721296889));
#32107=CARTESIAN_POINT('Ctrl Pts',(0.221926689463,1.52441165170123,-4.43824995043405));
#32108=CARTESIAN_POINT('Ctrl Pts',(-0.450285458827622,1.54477765231458,
-4.41673352060185));
#32109=CARTESIAN_POINT('Ctrl Pts',(-1.26358566414186,1.00029259499041,-4.38579230410963));
#32110=CARTESIAN_POINT('Ctrl Pts',(-1.61297063863451,0.0851696210599042,
-4.35408217822798));
#32111=CARTESIAN_POINT('Ctrl Pts',(-1.36691769149066,-0.86636719535778,
-4.32382427572184));
#32112=CARTESIAN_POINT('Ctrl Pts',(-0.740664712301201,-1.39406711347056,
-4.29568368658589));
#32113=CARTESIAN_POINT('Ctrl Pts',(-0.123568561445898,-1.54231629531191,
-4.27827259231965));
#32114=CARTESIAN_POINT('Ctrl Pts',(0.477570602247783,-1.50045464230821,
-4.25010620760684));
#32115=CARTESIAN_POINT('Ctrl Pts',(1.12799462557692,-1.14561364539286,-4.21523812123688));
#32116=CARTESIAN_POINT('Ctrl Pts',(1.56388513724472,-0.389673012803625,
-4.17546007003578));
#32117=CARTESIAN_POINT('Ctrl Pts',(1.5433188232119,0.410763669941787,-4.13857735821636));
#32118=CARTESIAN_POINT('Ctrl Pts',(1.19490853879333,1.03893941579882,-4.10508910882579));
#32119=CARTESIAN_POINT('Ctrl Pts',(0.681279880783051,1.43269210784687,-4.07487536403218));
#32120=CARTESIAN_POINT('Ctrl Pts',(0.051646821861207,1.58859643745763,-4.04459309324451));
#32121=CARTESIAN_POINT('Ctrl Pts',(-0.588862535961304,1.47930900476985,
-4.01426969238989));
#32122=CARTESIAN_POINT('Ctrl Pts',(-1.13322870809872,1.1225062752352,-3.98388228335323));
#32123=CARTESIAN_POINT('Ctrl Pts',(-1.4902067993283,0.576759659588736,-3.95344539501966));
#32124=CARTESIAN_POINT('Ctrl Pts',(-1.58102020223693,0.0400740757948976,
-3.92803411508518));
#32125=CARTESIAN_POINT('Ctrl Pts',(-1.52052962309553,-0.384828263720139,
-3.90767925424071));
#32126=CARTESIAN_POINT('Ctrl Pts',(-1.3748830928401,-0.788957250234775,
-3.88730621071591));
#32127=CARTESIAN_POINT('Ctrl Pts',(-1.0423371162911,-1.22218867468557,-3.86180720794638));
#32128=CARTESIAN_POINT('Ctrl Pts',(-0.467378790598492,-1.53972799805516,
-3.83115568482052));
#32129=CARTESIAN_POINT('Ctrl Pts',(0.187274531141039,-1.60068158914455,
-3.80045226057647));
#32130=CARTESIAN_POINT('Ctrl Pts',(0.883096272461548,-1.37238382842803,
-3.76628010013367));
#32131=CARTESIAN_POINT('Ctrl Pts',(1.45542862121288,-0.785128737057825,
-3.72861800828645));
#32132=CARTESIAN_POINT('Ctrl Pts',(1.62183852895481,-0.0567398924127903,
-3.69430530328978));
#32133=CARTESIAN_POINT('Ctrl Pts',(1.51242393883133,0.515046269014153,-3.66681113832745));
#32134=CARTESIAN_POINT('Ctrl Pts',(1.25371395215128,1.0371419048164,-3.63928782397711));
#32135=CARTESIAN_POINT('Ctrl Pts',(0.679041108905056,1.51956040430477,-3.60482953394523));
#32136=CARTESIAN_POINT('Ctrl Pts',(-0.213247562120534,1.65433450298338,
-3.56339447382386));
#32137=CARTESIAN_POINT('Ctrl Pts',(-1.04680323812526,1.30346814108,-3.52187569315801));
#32138=CARTESIAN_POINT('Ctrl Pts',(-1.57557751626781,0.567442201034068,
-3.48027478133792));
#32139=CARTESIAN_POINT('Ctrl Pts',(-1.64318830952972,-0.337637019006298,
-3.43859332018342));
#32140=CARTESIAN_POINT('Ctrl Pts',(-1.22844519515377,-1.14714492715669,
-3.39683307764518));
#32141=CARTESIAN_POINT('Ctrl Pts',(-0.451245980735406,-1.62215680765017,
-3.35499576544402));
#32142=CARTESIAN_POINT('Ctrl Pts',(0.461841974941765,-1.62319460304399,
-3.31308315566976));
#32143=CARTESIAN_POINT('Ctrl Pts',(1.17649440309474,-1.18543555842648,-3.27459582000513));
#32144=CARTESIAN_POINT('Ctrl Pts',(1.5636738872075,-0.54221871976191,-3.23955517618414));
#32145=CARTESIAN_POINT('Ctrl Pts',(1.65231581225766,0.128238780519003,-3.20797910267182));
#32146=CARTESIAN_POINT('Ctrl Pts',(1.46493973472583,0.779138006438161,-3.17636441807156));
#32147=CARTESIAN_POINT('Ctrl Pts',(1.03253139188493,1.30136595938992,-3.14471191495533));
#32148=CARTESIAN_POINT('Ctrl Pts',(0.426609970086491,1.60751024918497,-3.11302251069183));
#32149=CARTESIAN_POINT('Ctrl Pts',(-0.251933879032834,1.64584505089144,
-3.08129700553233));
#32150=CARTESIAN_POINT('Ctrl Pts',(-0.889905805470703,1.40942555957253,
-3.04953632759992));
#32151=CARTESIAN_POINT('Ctrl Pts',(-1.38068331350981,0.937053401938582,
-3.01774135131172));
#32152=CARTESIAN_POINT('Ctrl Pts',(-1.64184179716058,0.307317409087506,
-2.98591300518706));
#32153=CARTESIAN_POINT('Ctrl Pts',(-1.62957916709941,-0.37530803509689,
-2.95405221275351));
#32154=CARTESIAN_POINT('Ctrl Pts',(-1.34474730528677,-0.996034495385219,
-2.92215989404433));
#32155=CARTESIAN_POINT('Ctrl Pts',(-0.778879409529726,-1.50350912987896,
-2.88668999089474));
#32156=CARTESIAN_POINT('Ctrl Pts',(0.0452156959044932,-1.71370006437942,
-2.84763094470004));
#32157=CARTESIAN_POINT('Ctrl Pts',(0.785100365893931,-1.486208751186,-2.81208062847635));
#32158=CARTESIAN_POINT('Ctrl Pts',(1.24161679713701,-1.09259013745182,-2.7836165314676));
#32159=CARTESIAN_POINT('Ctrl Pts',(1.49217131201598,-0.716178712962469,
-2.76225639002869));
#32160=CARTESIAN_POINT('Ctrl Pts',(1.63085414425123,-0.285537734548898,
-2.7408855262812));
#32161=CARTESIAN_POINT('Ctrl Pts',(1.65475200752033,0.317728375257333,-2.7123738937245));
#32162=CARTESIAN_POINT('Ctrl Pts',(1.37145521865962,1.04076278423927,-2.67671479060714));
#32163=CARTESIAN_POINT('Ctrl Pts',(0.69041646931577,1.55777895441666,-2.63743464573646));
#32164=CARTESIAN_POINT('Ctrl Pts',(-0.0643948515707663,1.68574777587918,
-2.6017316079884));
#32165=CARTESIAN_POINT('Ctrl Pts',(-0.733422672005601,1.52073388540773,
-2.56950115646222));
#32166=CARTESIAN_POINT('Ctrl Pts',(-1.28085476582717,1.10113604465525,-2.53741554342871));
#32167=CARTESIAN_POINT('Ctrl Pts',(-1.61517951924605,0.4975562304161,-2.50499073603886));
#32168=CARTESIAN_POINT('Ctrl Pts',(-1.68029840248005,-0.189791143389858,
-2.47314557601871));
#32169=CARTESIAN_POINT('Ctrl Pts',(-1.46497737904047,-0.846156793246451,
-2.44020210847229));
#32170=CARTESIAN_POINT('Ctrl Pts',(-1.00508021286665,-1.36188270355857,
-2.40899190246463));
#32171=CARTESIAN_POINT('Ctrl Pts',(-0.507582321376923,-1.59058364540096,
-2.38240038156976));
#32172=CARTESIAN_POINT('Ctrl Pts',(-0.115985349294589,-1.64889286597431,
-2.36303576958252));
#32173=CARTESIAN_POINT('Ctrl Pts',(0.223158570335046,-1.64681924620263,
-2.349562123073));
#32174=CARTESIAN_POINT('Ctrl Pts',(0.806901355148856,-1.50671742388011,
-2.33231544041505));
#32175=CARTESIAN_POINT('Ctrl Pts',(1.48644477626825,-0.934917871941825,
-2.30237235343056));
#32176=CARTESIAN_POINT('Ctrl Pts',(1.75362331696032,0.0983401101520701,
-2.26920259215576));
#32177=CARTESIAN_POINT('Ctrl Pts',(1.37388207698597,1.09486845045221,-2.23481640537456));
#32178=CARTESIAN_POINT('Ctrl Pts',(0.486437491100621,1.68918937268853,-2.20098350021554));
#32179=CARTESIAN_POINT('Ctrl Pts',(-0.402275175720241,1.66276347810902,
-2.172565595614));
#32180=CARTESIAN_POINT('Ctrl Pts',(-1.0075498708897,1.33971834323449,-2.14990060001603));
#32181=CARTESIAN_POINT('Ctrl Pts',(-1.36740441992316,0.968073875003734,
-2.13287342310861));
#32182=CARTESIAN_POINT('Ctrl Pts',(-1.59664060478066,0.509453342147398,
-2.11589441486025));
#32183=CARTESIAN_POINT('Ctrl Pts',(-1.64911395659225,0.173292258411803,
-2.10450673116507));
#32184=CARTESIAN_POINT('Ctrl Pts',(-1.64973702763284,0.000250310089940127,
-2.09887467748946));
#32185=CARTESIAN_POINT('',(0.,0.,0.));
#32186=CARTESIAN_POINT('Origin',(1.535,0.385,-1.2));
#32187=CARTESIAN_POINT('',(1.52,0.4,-0.6));
#32188=CARTESIAN_POINT('',(1.55,0.37,-0.6));
#32189=CARTESIAN_POINT('',(1.52,0.4,-0.6));
#32190=CARTESIAN_POINT('',(1.55,0.37,-1.4));
#32191=CARTESIAN_POINT('',(1.55,0.37,-1.2));
#32192=CARTESIAN_POINT('',(1.52,0.4,-1.4));
#32193=CARTESIAN_POINT('',(1.55,0.37,-1.4));
#32194=CARTESIAN_POINT('',(1.52,0.4,-1.2));
#32195=CARTESIAN_POINT('Origin',(1.535,2.77555756156289E-17,-0.6));
#32196=CARTESIAN_POINT('',(1.52,-0.4,-0.6));
#32197=CARTESIAN_POINT('',(1.55,-0.37,-0.6));
#32198=CARTESIAN_POINT('',(1.52,-0.4,-0.6));
#32199=CARTESIAN_POINT('Origin',(1.55,2.77555756156289E-17,-0.6));
#32200=CARTESIAN_POINT('Origin',(1.52,2.77555756156289E-17,-0.6));
#32201=CARTESIAN_POINT('Origin',(1.535,-0.385,-0.8));
#32202=CARTESIAN_POINT('',(1.52,-0.4,-1.4));
#32203=CARTESIAN_POINT('',(1.55,-0.37,-1.4));
#32204=CARTESIAN_POINT('',(1.52,-0.4,-1.4));
#32205=CARTESIAN_POINT('',(1.55,-0.37,-0.8));
#32206=CARTESIAN_POINT('',(1.52,-0.4,-0.8));
#32207=CARTESIAN_POINT('Origin',(1.535,2.77555756156289E-17,-1.4));
#32208=CARTESIAN_POINT('Origin',(1.55,2.77555756156289E-17,-1.4));
#32209=CARTESIAN_POINT('Origin',(1.52,2.77555756156289E-17,-1.4));
#32210=CARTESIAN_POINT('Origin',(0.85,2.77555756156289E-17,-0.6));
#32211=CARTESIAN_POINT('',(0.85,0.4,-0.6));
#32212=CARTESIAN_POINT('',(0.85,0.4,-0.6));
#32213=CARTESIAN_POINT('',(0.85,-0.4,-0.6));
#32214=CARTESIAN_POINT('Origin',(0.85,2.77555756156289E-17,-0.6));
#32215=CARTESIAN_POINT('',(0.85,-0.4,-0.6));
#32216=CARTESIAN_POINT('Origin',(0.85,0.4,-1.4));
#32217=CARTESIAN_POINT('',(0.85,0.4,-1.4));
#32218=CARTESIAN_POINT('',(0.85,0.4,-1.4));
#32219=CARTESIAN_POINT('',(0.85,0.4,-0.6));
#32220=CARTESIAN_POINT('Origin',(1.55,0.,-1.));
#32221=CARTESIAN_POINT('Origin',(0.85,2.77555756156289E-17,-1.4));
#32222=CARTESIAN_POINT('',(0.85,-0.4,-1.4));
#32223=CARTESIAN_POINT('',(0.85,-0.4,-1.4));
#32224=CARTESIAN_POINT('Origin',(0.85,2.77555756156289E-17,-1.4));
#32225=CARTESIAN_POINT('Origin',(0.85,-0.4,-0.6));
#32226=CARTESIAN_POINT('',(0.85,-0.4,-1.4));
#32227=CARTESIAN_POINT('Origin',(0.85,0.,-1.));
#32228=CARTESIAN_POINT('',(0.,0.,0.));
#32229=CARTESIAN_POINT('Origin',(0.,0.,0.68));
#32230=CARTESIAN_POINT('',(-1.9,-2.32682891837997E-16,0.66));
#32231=CARTESIAN_POINT('Origin',(0.,0.,0.66));
#32232=CARTESIAN_POINT('',(-1.9,-2.32682891837997E-16,0.7));
#32233=CARTESIAN_POINT('',(-1.9,-2.32682891837997E-16,0.68));
#32234=CARTESIAN_POINT('Origin',(0.,0.,0.7));
#32235=CARTESIAN_POINT('Origin',(0.,0.,0.68));
#32236=CARTESIAN_POINT('',(-1.7,-2.0818995585505E-16,0.66));
#32237=CARTESIAN_POINT('Origin',(0.,0.,0.66));
#32238=CARTESIAN_POINT('',(-1.7,-2.0818995585505E-16,0.7));
#32239=CARTESIAN_POINT('',(-1.7,-2.0818995585505E-16,0.68));
#32240=CARTESIAN_POINT('Origin',(0.,0.,0.7));
#32241=CARTESIAN_POINT('Origin',(1.9,0.,0.66));
#32242=CARTESIAN_POINT('Origin',(1.4,0.,0.7));
#32243=CARTESIAN_POINT('',(-1.4,-1.71450551880629E-16,0.7));
#32244=CARTESIAN_POINT('Origin',(0.,0.,0.7));
#32245=CARTESIAN_POINT('Origin',(0.,0.,0.68));
#32246=CARTESIAN_POINT('',(1.96,-2.40030772632881E-16,0.7));
#32247=CARTESIAN_POINT('Origin',(0.,0.,0.7));
#32248=CARTESIAN_POINT('',(2.,2.44929359829471E-16,0.66));
#32249=CARTESIAN_POINT('',(1.98,2.42480066231176E-16,0.68));
#32250=CARTESIAN_POINT('',(-2.,-2.44929359829471E-16,0.66));
#32251=CARTESIAN_POINT('Origin',(0.,0.,0.66));
#32252=CARTESIAN_POINT('Origin',(0.,0.,0.66));
#32253=CARTESIAN_POINT('Origin',(0.,0.,0.35));
#32254=CARTESIAN_POINT('',(-2.,-2.44929359829471E-16,0.04));
#32255=CARTESIAN_POINT('',(-2.,-2.44929359829471E-16,0.35));
#32256=CARTESIAN_POINT('',(2.,-2.44929359829471E-16,0.04));
#32257=CARTESIAN_POINT('Origin',(0.,0.,0.04));
#32258=CARTESIAN_POINT('Origin',(0.,0.,0.04));
#32259=CARTESIAN_POINT('Origin',(1.4,0.,0.7));
#32260=CARTESIAN_POINT('Origin',(0.,0.,0.02));
#32261=CARTESIAN_POINT('',(1.96,2.40030772632881E-16,0.));
#32262=CARTESIAN_POINT('',(1.98,2.42480066231176E-16,0.02));
#32263=CARTESIAN_POINT('Origin',(0.,0.,0.));
#32264=CARTESIAN_POINT('Origin',(2.,0.,0.));
#32265=CARTESIAN_POINT('',(-1.65,-2.02066721859313E-16,6.93889390390723E-18));
#32266=CARTESIAN_POINT('Origin',(0.,0.,0.));
#32267=CARTESIAN_POINT('Origin',(0.,0.,0.06));
#32268=CARTESIAN_POINT('',(-1.65,-2.02066721859313E-16,0.12));
#32269=CARTESIAN_POINT('Origin',(0.,0.,0.12));
#32270=CARTESIAN_POINT('',(-1.65,-2.02066721859313E-16,0.06));
#32271=CARTESIAN_POINT('Origin',(0.,0.,0.665));
#32272=CARTESIAN_POINT('',(-1.4,-1.71450551880629E-16,0.63));
#32273=CARTESIAN_POINT('',(-1.4,-1.71450551880629E-16,0.665));
#32274=CARTESIAN_POINT('Origin',(0.,0.,0.63));
#32275=CARTESIAN_POINT('Origin',(0.,0.,0.595));
#32276=CARTESIAN_POINT('',(-1.55,-1.8982025386784E-16,0.56));
#32277=CARTESIAN_POINT('',(-1.475,-1.80635402874235E-16,0.595));
#32278=CARTESIAN_POINT('Origin',(0.,0.,0.56));
#32279=CARTESIAN_POINT('Origin',(0.,0.,0.49));
#32280=CARTESIAN_POINT('',(-1.55,-1.8982025386784E-16,0.42));
#32281=CARTESIAN_POINT('',(-1.55,-1.8982025386784E-16,0.49));
#32282=CARTESIAN_POINT('Origin',(0.,0.,0.42));
#32283=CARTESIAN_POINT('Origin',(0.,0.,0.37));
#32284=CARTESIAN_POINT('',(-1.25,-1.53080849893419E-16,0.32));
#32285=CARTESIAN_POINT('',(-1.4,-1.71450551880629E-16,0.37));
#32286=CARTESIAN_POINT('Origin',(0.,0.,0.32));
#32287=CARTESIAN_POINT('Origin',(0.,0.,0.29));
#32288=CARTESIAN_POINT('',(-1.25,-1.53080849893419E-16,0.26));
#32289=CARTESIAN_POINT('',(-1.25,-1.53080849893419E-16,0.29));
#32290=CARTESIAN_POINT('Origin',(0.,0.,0.26));
#32291=CARTESIAN_POINT('Origin',(0.,0.,0.19));
#32292=CARTESIAN_POINT('',(-1.55,-1.8982025386784E-16,0.12));
#32293=CARTESIAN_POINT('',(-1.4,-1.71450551880629E-16,0.19));
#32294=CARTESIAN_POINT('Origin',(0.,0.,0.12));
#32295=CARTESIAN_POINT('Origin',(1.65,0.,0.12));
#32296=CARTESIAN_POINT('',(0.,0.,0.));
#32297=CARTESIAN_POINT('Origin',(0.,0.,-1.33003901172249));
#32298=CARTESIAN_POINT('',(-0.747455179358203,1.21560254491701E-5,-0.193723222248808));
#32299=CARTESIAN_POINT('',(-0.747444078220075,-6.40459137760119E-6,-0.187197830382768));
#32300=CARTESIAN_POINT('',(-0.7475,-1.95907305151415E-14,-1.33003901172249));
#32301=CARTESIAN_POINT('',(0.708694801171174,0.237542783106662,-0.12));
#32302=CARTESIAN_POINT('Ctrl Pts',(-0.747455179358203,1.21560254491664E-5,
-0.193723222248808));
#32303=CARTESIAN_POINT('Ctrl Pts',(-0.747409043365027,-0.0764700511820524,
-0.191546603424787));
#32304=CARTESIAN_POINT('Ctrl Pts',(-0.717056524628233,-0.275197846725069,
-0.185891997066606));
#32305=CARTESIAN_POINT('Ctrl Pts',(-0.543630981761309,-0.556730447339977,
-0.176759403174265));
#32306=CARTESIAN_POINT('Ctrl Pts',(-0.217353554555294,-0.747156946739445,
-0.166325440571784));
#32307=CARTESIAN_POINT('Ctrl Pts',(0.160155550638919,-0.761465819139253,
-0.155891477969304));
#32308=CARTESIAN_POINT('Ctrl Pts',(0.499915663487151,-0.59630128045638,
-0.145457515366823));
#32309=CARTESIAN_POINT('Ctrl Pts',(0.721838643854921,-0.290560778341041,
-0.135023552764343));
#32310=CARTESIAN_POINT('Ctrl Pts',(0.763953513632068,0.0137597889773607,
-0.126537714308735));
#32311=CARTESIAN_POINT('Ctrl Pts',(0.725795582116324,0.186572354342476,
-0.121529863387287));
#32312=CARTESIAN_POINT('Ctrl Pts',(0.708694801171174,0.237542783106662,
-0.12));
#32313=CARTESIAN_POINT('',(0.747395528060274,0.0124969850565471,-0.12));
#32314=CARTESIAN_POINT('Origin',(0.,0.,-0.12));
#32315=CARTESIAN_POINT('Ctrl Pts',(-0.747444078220075,-6.40459137765323E-6,
-0.187197830382768));
#32316=CARTESIAN_POINT('Ctrl Pts',(-0.747460394071194,-0.0538175344429383,
-0.185666478793473));
#32317=CARTESIAN_POINT('Ctrl Pts',(-0.728699568742349,-0.229832596850158,
-0.180657139670018));
#32318=CARTESIAN_POINT('Ctrl Pts',(-0.591963456523644,-0.505033918677001,
-0.172169813012403));
#32319=CARTESIAN_POINT('Ctrl Pts',(-0.284343786563683,-0.724320025643106,
-0.161735850409922));
#32320=CARTESIAN_POINT('Ctrl Pts',(0.09031673140191,-0.772864465068915,
-0.151301887807442));
#32321=CARTESIAN_POINT('Ctrl Pts',(0.44365235923649,-0.639262442637623,
-0.140867925204961));
#32322=CARTESIAN_POINT('Ctrl Pts',(0.692489824641788,-0.354929918130683,
-0.13043396260248));
#32323=CARTESIAN_POINT('Ctrl Pts',(0.749438361810141,-0.109676867461678,
-0.12347798753416));
#32324=CARTESIAN_POINT('Ctrl Pts',(0.747395528060274,0.012496985056547,
-0.12));
#32325=CARTESIAN_POINT('Origin',(0.,0.,-1.33003901172249));
#32326=CARTESIAN_POINT('',(-0.747444051384665,-6.42748184059897E-6,-0.327407432775125));
#32327=CARTESIAN_POINT('',(-0.747492032740272,-1.77696257388504E-5,-0.320882040909084));
#32328=CARTESIAN_POINT('',(-0.7475,-1.95907305151415E-14,-1.33003901172249));
#32329=CARTESIAN_POINT('Ctrl Pts',(-0.747444051384665,-6.42748184055686E-6,
-0.327407432775125));
#32330=CARTESIAN_POINT('Ctrl Pts',(-0.747460735268479,-0.0535655898421367,
-0.325883248386414));
#32331=CARTESIAN_POINT('Ctrl Pts',(-0.728815731862446,-0.229328242581168,
-0.320881076463544));
#32332=CARTESIAN_POINT('Ctrl Pts',(-0.592475727944849,-0.504436944883207,
-0.312400917006513));
#32333=CARTESIAN_POINT('Ctrl Pts',(-0.285071300054314,-0.724029331642755,
-0.301966954404032));
#32334=CARTESIAN_POINT('Ctrl Pts',(0.0895271131383019,-0.772961199617318,
-0.291532991801552));
#32335=CARTESIAN_POINT('Ctrl Pts',(0.443023143994601,-0.639698844990308,
-0.281099029199071));
#32336=CARTESIAN_POINT('Ctrl Pts',(0.692094455558156,-0.355653462496774,
-0.27066506659659));
#32337=CARTESIAN_POINT('Ctrl Pts',(0.778032597283115,0.0122227909580681,
-0.26023110399411));
#32338=CARTESIAN_POINT('Ctrl Pts',(0.680581143349384,0.377218004776158,
-0.249797141391629));
#32339=CARTESIAN_POINT('Ctrl Pts',(0.422710313521399,0.653299414263413,
-0.239363178789149));
#32340=CARTESIAN_POINT('Ctrl Pts',(0.0652026943778876,0.775391960536891,
-0.228929216186668));
#32341=CARTESIAN_POINT('Ctrl Pts',(-0.307673823063876,0.714717431064052,
-0.218495253584187));
#32342=CARTESIAN_POINT('Ctrl Pts',(-0.608028707877235,0.485577090895019,
-0.208061290981707));
#32343=CARTESIAN_POINT('Ctrl Pts',(-0.732306246915869,0.213659075752679,
-0.199803947203247));
#32344=CARTESIAN_POINT('Ctrl Pts',(-0.747482763396927,0.0457397543737755,
-0.195024590958948));
#32345=CARTESIAN_POINT('Ctrl Pts',(-0.747455179358203,1.21560254491664E-5,
-0.193723222248808));
#32346=CARTESIAN_POINT('Ctrl Pts',(-0.747492032740272,-1.77696257388088E-5,
-0.320882040909084));
#32347=CARTESIAN_POINT('Ctrl Pts',(-0.747521461794713,-0.0308968347335437,
-0.3200031237551));
#32348=CARTESIAN_POINT('Ctrl Pts',(-0.738208053524619,-0.183950674319053,
-0.315646219066956));
#32349=CARTESIAN_POINT('Ctrl Pts',(-0.635857117988058,-0.448519615362849,
-0.307811326844651));
#32350=CARTESIAN_POINT('Ctrl Pts',(-0.349675784487423,-0.695133774103561,
-0.29737736424217));
#32351=CARTESIAN_POINT('Ctrl Pts',(0.0189274157531888,-0.777898369643474,
-0.28694340163969));
#32352=CARTESIAN_POINT('Ctrl Pts',(0.383069251609914,-0.67730500314506,
-0.276509439037209));
#32353=CARTESIAN_POINT('Ctrl Pts',(0.656918053157321,-0.417064487823481,
-0.266075476434728));
#32354=CARTESIAN_POINT('Ctrl Pts',(0.775925115315038,-0.0585179376441977,
-0.255641513832248));
#32355=CARTESIAN_POINT('Ctrl Pts',(0.712039292365909,0.313821812003488,
-0.245207551229767));
#32356=CARTESIAN_POINT('Ctrl Pts',(0.480319196218496,0.612190866640263,
-0.234773588627287));
#32357=CARTESIAN_POINT('Ctrl Pts',(0.135383189993241,0.766260668703223,
-0.224339626024806));
#32358=CARTESIAN_POINT('Ctrl Pts',(-0.241463591288354,0.739715845333339,
-0.213905663422325));
#32359=CARTESIAN_POINT('Ctrl Pts',(-0.561395755032469,0.5388126158932,-0.203471700819845));
#32360=CARTESIAN_POINT('Ctrl Pts',(-0.721466439761005,0.25903244063098,
-0.194569089806659));
#32361=CARTESIAN_POINT('Ctrl Pts',(-0.747423337703997,0.0683976642946542,
-0.189144466327633));
#32362=CARTESIAN_POINT('Ctrl Pts',(-0.747444078220075,-6.40459137765323E-6,
-0.187197830382768));
#32363=CARTESIAN_POINT('Origin',(0.,0.,-1.33003901172249));
#32364=CARTESIAN_POINT('',(-0.747492771866375,-1.77854026472873E-5,-0.46109164330144));
#32365=CARTESIAN_POINT('',(-0.747552914013562,-7.59237280062441E-6,-0.4545662514354));
#32366=CARTESIAN_POINT('',(-0.7475,-1.95907305151415E-14,-1.33003901172249));
#32367=CARTESIAN_POINT('Ctrl Pts',(-0.747492771866375,-1.77854026472586E-5,
-0.46109164330144));
#32368=CARTESIAN_POINT('Ctrl Pts',(-0.747522042549813,-0.0306449575355944,
-0.460219893348041));
#32369=CARTESIAN_POINT('Ctrl Pts',(-0.738300189612618,-0.18344667931334,
-0.455870155860481));
#32370=CARTESIAN_POINT('Ctrl Pts',(-0.636310057828871,-0.44787680201301,
-0.448042430838761));
#32371=CARTESIAN_POINT('Ctrl Pts',(-0.350378094607072,-0.694780044542982,
-0.43760846823628));
#32372=CARTESIAN_POINT('Ctrl Pts',(0.0181412792138254,-0.777917099351843,
-0.4271745056338));
#32373=CARTESIAN_POINT('Ctrl Pts',(0.382384582988461,-0.677691781098534,
-0.416740543031318));
#32374=CARTESIAN_POINT('Ctrl Pts',(0.656496245978095,-0.417728139454399,
-0.406306580428839));
#32375=CARTESIAN_POINT('Ctrl Pts',(0.775865572452267,-0.0593020485231105,
-0.395872617826357));
#32376=CARTESIAN_POINT('Ctrl Pts',(0.71235609003925,0.313102092711011,-0.385438655223877));
#32377=CARTESIAN_POINT('Ctrl Pts',(0.480937580760022,0.611705127399056,
-0.375004692621396));
#32378=CARTESIAN_POINT('Ctrl Pts',(0.136157562681014,0.766123513283346,
-0.364570730018916));
#32379=CARTESIAN_POINT('Ctrl Pts',(-0.240716072858233,0.739959385191357,
-0.354136767416435));
#32380=CARTESIAN_POINT('Ctrl Pts',(-0.560850667196364,0.539379874112098,
-0.343702804813955));
#32381=CARTESIAN_POINT('Ctrl Pts',(-0.721333836132674,0.259535992032654,
-0.334793026600185));
#32382=CARTESIAN_POINT('Ctrl Pts',(-0.747422664848419,0.0686493471490407,
-0.329361235920574));
#32383=CARTESIAN_POINT('Ctrl Pts',(-0.747444051384665,-6.42748184055686E-6,
-0.327407432775125));
#32384=CARTESIAN_POINT('Ctrl Pts',(-0.747552914013562,-7.5923728006114E-6,
-0.4545662514354));
#32385=CARTESIAN_POINT('Ctrl Pts',(-0.747557174200553,-0.00796275413960644,
-0.454339768716726));
#32386=CARTESIAN_POINT('Ctrl Pts',(-0.745521898301695,-0.138079373049215,
-0.450635298463892));
#32387=CARTESIAN_POINT('Ctrl Pts',(-0.674371225051026,-0.388210728933218,
-0.443452840676899));
#32388=CARTESIAN_POINT('Ctrl Pts',(-0.412054943730941,-0.660071846530996,
-0.433018878074418));
#32389=CARTESIAN_POINT('Ctrl Pts',(-0.0526134386847218,-0.776347824950465,
-0.422584915471937));
#32390=CARTESIAN_POINT('Ctrl Pts',(0.319229548446936,-0.709631323036316,
-0.412150952869456));
#32391=CARTESIAN_POINT('Ctrl Pts',(0.615827130120359,-0.475648047450979,
-0.401716990266976));
#32392=CARTESIAN_POINT('Ctrl Pts',(0.767268468189365,-0.129550055793601,
-0.391283027664495));
#32393=CARTESIAN_POINT('Ctrl Pts',(0.737857415668762,0.24708410184319,-0.380849065062015));
#32394=CARTESIAN_POINT('Ctrl Pts',(0.534526434095284,0.565478213973463,
-0.370415102459534));
#32395=CARTESIAN_POINT('Ctrl Pts',(0.205202547258304,0.750583795355781,
-0.359981139857054));
#32396=CARTESIAN_POINT('Ctrl Pts',(-0.172489509004567,0.758769720339229,
-0.349547177254573));
#32397=CARTESIAN_POINT('Ctrl Pts',(-0.509524166428113,0.588106489551379,
-0.339113214652093));
#32398=CARTESIAN_POINT('Ctrl Pts',(-0.708185410677574,0.304874056256314,
-0.329558169203596));
#32399=CARTESIAN_POINT('Ctrl Pts',(-0.747405007264242,0.0912955733047001,
-0.32348111128926));
#32400=CARTESIAN_POINT('Ctrl Pts',(-0.747492032740272,-1.77696257388088E-5,
-0.320882040909084));
#32401=CARTESIAN_POINT('Origin',(0.,0.,-1.33003901172249));
#32402=CARTESIAN_POINT('',(-0.747553321122146,-7.36938304350496E-6,-0.594775853827756));
#32403=CARTESIAN_POINT('',(-0.747538056636856,1.3017034258378E-5,-0.588250461961716));
#32404=CARTESIAN_POINT('',(-0.7475,-1.95907305151415E-14,-1.33003901172249));
#32405=CARTESIAN_POINT('Ctrl Pts',(-0.747553321122146,-7.36938304344778E-6,
-0.594775853827756));
#32406=CARTESIAN_POINT('Ctrl Pts',(-0.747557343204729,-0.00771077241775835,
-0.594556538309667));
#32407=CARTESIAN_POINT('Ctrl Pts',(-0.745590310689939,-0.137575565048739,
-0.590859235257418));
#32408=CARTESIAN_POINT('Ctrl Pts',(-0.674763198638613,-0.387529025027261,
-0.583683944671008));
#32409=CARTESIAN_POINT('Ctrl Pts',(-0.412721788492088,-0.659655095318368,
-0.573249982068528));
#32410=CARTESIAN_POINT('Ctrl Pts',(-0.0533979730410232,-0.776294258609905,
-0.562816019466047));
#32411=CARTESIAN_POINT('Ctrl Pts',(0.318512246619028,-0.709953567657274,
-0.552382056863567));
#32412=CARTESIAN_POINT('Ctrl Pts',(0.615346135603009,-0.476270146948173,
-0.541948094261086));
#32413=CARTESIAN_POINT('Ctrl Pts',(0.767137155915032,-0.130325375465362,
-0.531514131658606));
#32414=CARTESIAN_POINT('Ctrl Pts',(0.738106737168653,0.246338312127524,
-0.521080169056125));
#32415=CARTESIAN_POINT('Ctrl Pts',(0.535097621960438,0.56493774386907,-0.510646206453644));
#32416=CARTESIAN_POINT('Ctrl Pts',(0.20596096711532,0.750376038730258,-0.500212243851164));
#32417=CARTESIAN_POINT('Ctrl Pts',(-0.171722623797873,0.758943647414989,
-0.489778281248683));
#32418=CARTESIAN_POINT('Ctrl Pts',(-0.50892957801762,0.588621104017174,
-0.479344318646202));
#32419=CARTESIAN_POINT('Ctrl Pts',(-0.708026179252433,0.305377277568616,
-0.469782105997122));
#32420=CARTESIAN_POINT('Ctrl Pts',(-0.747405262420699,0.0915471027789014,
-0.463697880882201));
#32421=CARTESIAN_POINT('Ctrl Pts',(-0.747492771866375,-1.77854026472586E-5,
-0.46109164330144));
#32422=CARTESIAN_POINT('Ctrl Pts',(-0.747538056636856,1.30170342583693E-5,
-0.588250461961716));
#32423=CARTESIAN_POINT('Ctrl Pts',(-0.747449782311829,-0.107195335869156,
-0.585198426144193));
#32424=CARTESIAN_POINT('Ctrl Pts',(-0.697538394050389,-0.33665395487388,
-0.578668402792509));
#32425=CARTESIAN_POINT('Ctrl Pts',(-0.470949408769067,-0.619427779176751,
-0.568660391906665));
#32426=CARTESIAN_POINT('Ctrl Pts',(-0.123709349589919,-0.768231811408391,
-0.558226429304186));
#32427=CARTESIAN_POINT('Ctrl Pts',(0.252690166207058,-0.735956383991622,
-0.547792466701704));
#32428=CARTESIAN_POINT('Ctrl Pts',(0.569528234436075,-0.530209118571064,
-0.537358504099224));
#32429=CARTESIAN_POINT('Ctrl Pts',(0.752123144005562,-0.199486579716444,
-0.526924541496743));
#32430=CARTESIAN_POINT('Ctrl Pts',(0.757435558261682,0.178256821234392,
-0.516490578894262));
#32431=CARTESIAN_POINT('Ctrl Pts',(0.58421329122536,0.513983413731816,-0.506056616291782));
#32432=CARTESIAN_POINT('Ctrl Pts',(0.273286459598611,0.728559283954182,
-0.495622653689301));
#32433=CARTESIAN_POINT('Ctrl Pts',(-0.102056559562226,0.77140688218741,
-0.485188691086821));
#32434=CARTESIAN_POINT('Ctrl Pts',(-0.453343888260034,0.63242662674262,
-0.47475472848434));
#32435=CARTESIAN_POINT('Ctrl Pts',(-0.692468131949325,0.350629951601099,
-0.464547248600534));
#32436=CARTESIAN_POINT('Ctrl Pts',(-0.74749175253247,0.114200886509031,
-0.457817756250887));
#32437=CARTESIAN_POINT('Ctrl Pts',(-0.747552914013562,-7.5923728006114E-6,
-0.4545662514354));
#32438=CARTESIAN_POINT('Origin',(0.,0.,-1.33003901172249));
#32439=CARTESIAN_POINT('',(-0.747537418840408,1.31793815494462E-5,-0.728460064354072));
#32440=CARTESIAN_POINT('',(-0.747472643624562,1.62103417218756E-5,-0.721934672488032));
#32441=CARTESIAN_POINT('',(-0.7475,-1.95907305151415E-14,-1.33003901172249));
#32442=CARTESIAN_POINT('Ctrl Pts',(-0.747537418840408,1.31793815494417E-5,
-0.728460064354072));
#32443=CARTESIAN_POINT('Ctrl Pts',(-0.747448558105652,-0.106943676944281,
-0.725415195737133));
#32444=CARTESIAN_POINT('Ctrl Pts',(-0.697716187447847,-0.336151536347626,
-0.718892339586034));
#32445=CARTESIAN_POINT('Ctrl Pts',(-0.471575149406303,-0.618951531170265,
-0.708891495900776));
#32446=CARTESIAN_POINT('Ctrl Pts',(-0.124485645778937,-0.768106401138927,
-0.698457533298295));
#32447=CARTESIAN_POINT('Ctrl Pts',(0.251946294775516,-0.736211371838605,
-0.688023570695814));
#32448=CARTESIAN_POINT('Ctrl Pts',(0.568992125251126,-0.530784401501965,
-0.677589608093334));
#32449=CARTESIAN_POINT('Ctrl Pts',(0.751921163041749,-0.200246558136555,
-0.667155645490853));
#32450=CARTESIAN_POINT('Ctrl Pts',(0.757615314330881,0.177491281382809,
-0.656721682888373));
#32451=CARTESIAN_POINT('Ctrl Pts',(0.584732414132281,0.513392757388168,
-0.646287720285892));
#32452=CARTESIAN_POINT('Ctrl Pts',(0.274022587194125,0.728282734371089,
-0.635853757683411));
#32453=CARTESIAN_POINT('Ctrl Pts',(-0.101276939472296,0.771509624701284,
-0.625419795080931));
#32454=CARTESIAN_POINT('Ctrl Pts',(-0.452704539459628,0.632884443977129,
-0.61498583247845));
#32455=CARTESIAN_POINT('Ctrl Pts',(-0.692281540434249,0.351131872468854,
-0.604771185394059));
#32456=CARTESIAN_POINT('Ctrl Pts',(-0.747493559514422,0.114452674833002,
-0.598034525843827));
#32457=CARTESIAN_POINT('Ctrl Pts',(-0.747553321122146,-7.36938304344778E-6,
-0.594775853827756));
#32458=CARTESIAN_POINT('Ctrl Pts',(-0.747472643624562,1.6210341721886E-5,
-0.721934672488032));
#32459=CARTESIAN_POINT('Ctrl Pts',(-0.747402612221546,-0.0842954619945286,
-0.719535071105819));
#32460=CARTESIAN_POINT('Ctrl Pts',(-0.712499566770547,-0.290865199736191,
-0.713657482189446));
#32461=CARTESIAN_POINT('Ctrl Pts',(-0.525861117638763,-0.573545293931951,
-0.704301905738913));
#32462=CARTESIAN_POINT('Ctrl Pts',(-0.193759067069451,-0.753618964174968,
-0.693867943136433));
#32463=CARTESIAN_POINT('Ctrl Pts',(0.184013817024176,-0.756057560229359,
-0.683433980533952));
#32464=CARTESIAN_POINT('Ctrl Pts',(0.518412914638575,-0.580286282081279,
-0.673000017931472));
#32465=CARTESIAN_POINT('Ctrl Pts',(0.73061721497504,-0.267736072313561,
-0.66256605532899));
#32466=CARTESIAN_POINT('Ctrl Pts',(0.770608169635336,0.107922046529211,
-0.652132092726511));
#32467=CARTESIAN_POINT('Ctrl Pts',(0.62895953467438,0.458141924492798,-0.64169813012403));
#32468=CARTESIAN_POINT('Ctrl Pts',(0.339059224908714,0.700373444128258,
-0.63126416752155));
#32469=CARTESIAN_POINT('Ctrl Pts',(-0.0307605314660666,0.777520359180197,
-0.620830204919068));
#32470=CARTESIAN_POINT('Ctrl Pts',(-0.393329741412471,0.671398416557692,
-0.610396242316588));
#32471=CARTESIAN_POINT('Ctrl Pts',(-0.663187433844332,0.407021555727391,
-0.599962279714107));
#32472=CARTESIAN_POINT('Ctrl Pts',(-0.74351458894893,0.152101734785081,
-0.59258035292915));
#32473=CARTESIAN_POINT('Ctrl Pts',(-0.747550376479259,0.0149753519108121,
-0.588676413678353));
#32474=CARTESIAN_POINT('Ctrl Pts',(-0.747538056636856,1.30170342583693E-5,
-0.588250461961716));
#32475=CARTESIAN_POINT('Origin',(0.,0.,-1.33003901172249));
#32476=CARTESIAN_POINT('',(-0.747472002174668,1.61159471936433E-5,-0.862144274880388));
#32477=CARTESIAN_POINT('',(-0.747440403350747,2.49991181699993E-7,-0.855618883014348));
#32478=CARTESIAN_POINT('',(-0.7475,-1.95907305151415E-14,-1.33003901172249));
#32479=CARTESIAN_POINT('Ctrl Pts',(-0.747472002174668,1.61159471936609E-5,
-0.862144274880388));
#32480=CARTESIAN_POINT('Ctrl Pts',(-0.747402682287736,-0.0840439390973367,
-0.85975184069876));
#32481=CARTESIAN_POINT('Ctrl Pts',(-0.712650382827925,-0.290361716183338,
-0.853881418982972));
#32482=CARTESIAN_POINT('Ctrl Pts',(-0.526440462347927,-0.573013576696855,
-0.844533009733022));
#32483=CARTESIAN_POINT('Ctrl Pts',(-0.194520560057907,-0.753422770554806,
-0.834099047130545));
#32484=CARTESIAN_POINT('Ctrl Pts',(0.183249666810382,-0.75624313490388,
-0.823665084528061));
#32485=CARTESIAN_POINT('Ctrl Pts',(0.517826224589069,-0.580809883355642,
-0.813231121925582));
#32486=CARTESIAN_POINT('Ctrl Pts',(0.730346273449163,-0.268474282445113,
-0.802797159323101));
#32487=CARTESIAN_POINT('Ctrl Pts',(0.770716840097934,0.107143230607854,
-0.79236319672062));
#32488=CARTESIAN_POINT('Ctrl Pts',(0.629422202475751,0.457506077015547,
-0.781929234118141));
#32489=CARTESIAN_POINT('Ctrl Pts',(0.339766834898865,0.700030440322704,
-0.771495271515659));
#32490=CARTESIAN_POINT('Ctrl Pts',(-0.0299747696136733,0.777551048267703,
-0.76106130891318));
#32491=CARTESIAN_POINT('Ctrl Pts',(-0.392651039152918,0.671795564831834,
-0.750627346310697));
#32492=CARTESIAN_POINT('Ctrl Pts',(-0.662775767680288,0.407691551606601,
-0.740193383708218));
#32493=CARTESIAN_POINT('Ctrl Pts',(-0.743438739207481,0.152605612016257,
-0.732804289722675));
#32494=CARTESIAN_POINT('Ctrl Pts',(-0.747550058881758,0.0152273129384333,
-0.728893183271293));
#32495=CARTESIAN_POINT('Ctrl Pts',(-0.747537418840408,1.31793815494417E-5,
-0.728460064354072));
#32496=CARTESIAN_POINT('Ctrl Pts',(-0.747440403350747,2.49991181703463E-7,
-0.855618883014348));
#32497=CARTESIAN_POINT('Ctrl Pts',(-0.747439664227336,-0.0613952789202318,
-0.853871716067446));
#32498=CARTESIAN_POINT('Ctrl Pts',(-0.725057127938405,-0.245007983420982,
-0.848646561586384));
#32499=CARTESIAN_POINT('Ctrl Pts',(-0.576325689361536,-0.522812412838008,
-0.83994341957116));
#32500=CARTESIAN_POINT('Ctrl Pts',(-0.262170190030731,-0.732632862145289,
-0.82950945696868));
#32501=CARTESIAN_POINT('Ctrl Pts',(0.113781287599418,-0.769764858789943,
-0.819075494366201));
#32502=CARTESIAN_POINT('Ctrl Pts',(0.462913446150841,-0.625456042107332,
-0.808641531763718));
#32503=CARTESIAN_POINT('Ctrl Pts',(0.702932553865032,-0.333721356752229,
-0.79820756916124));
#32504=CARTESIAN_POINT('Ctrl Pts',(0.77726385077405,0.0366745895092527,
-0.787773606558758));
#32505=CARTESIAN_POINT('Ctrl Pts',(0.668386751451239,0.398425990267,-0.777339643956278));
#32506=CARTESIAN_POINT('Ctrl Pts',(0.401964611697131,0.666264639748313,
-0.766905681353798));
#32507=CARTESIAN_POINT('Ctrl Pts',(0.040795634331005,0.777058450475451,
-0.756471718751315));
#32508=CARTESIAN_POINT('Ctrl Pts',(-0.329989257542916,0.704692279751986,
-0.746037756148836));
#32509=CARTESIAN_POINT('Ctrl Pts',(-0.622992579377319,0.46622351428963,
-0.735603793546354));
#32510=CARTESIAN_POINT('Ctrl Pts',(-0.735537269423189,0.19797773894019,
-0.727569432326087));
#32511=CARTESIAN_POINT('Ctrl Pts',(-0.747504115891486,0.0379060617849294,
-0.72301305863998));
#32512=CARTESIAN_POINT('Ctrl Pts',(-0.747472643624562,1.6210341721886E-5,
-0.721934672488032));
#32513=CARTESIAN_POINT('Origin',(0.,0.,-1.33003901172249));
#32514=CARTESIAN_POINT('',(-0.747440394010334,2.88097106332193E-8,-0.995828485406703));
#32515=CARTESIAN_POINT('',(-0.747471187093045,-1.59917937688214E-5,-0.989303093540664));
#32516=CARTESIAN_POINT('',(-0.7475,-1.95907305151415E-14,-1.33003901172249));
#32517=CARTESIAN_POINT('Ctrl Pts',(-0.747440394010334,2.88097106414253E-8,
-0.995828485406703));
#32518=CARTESIAN_POINT('Ctrl Pts',(-0.747440305752117,-0.0611436444929983,
-0.994088485660386));
#32519=CARTESIAN_POINT('Ctrl Pts',(-0.72518211407954,-0.244504027566076,
-0.988870498379908));
#32520=CARTESIAN_POINT('Ctrl Pts',(-0.576853733233578,-0.522229725565815,
-0.980174523565273));
#32521=CARTESIAN_POINT('Ctrl Pts',(-0.262910442753167,-0.732367543071951,
-0.969740560962789));
#32522=CARTESIAN_POINT('Ctrl Pts',(0.113003322331734,-0.769879451565163,
-0.959306598360312));
#32523=CARTESIAN_POINT('Ctrl Pts',(0.462281136078415,-0.62592353336717,
-0.948872635757828));
#32524=CARTESIAN_POINT('Ctrl Pts',(0.702594943458043,-0.334431555819591,
-0.938438673155349));
#32525=CARTESIAN_POINT('Ctrl Pts',(0.777300516433143,0.0358890839459625,
-0.928004710552868));
#32526=CARTESIAN_POINT('Ctrl Pts',(0.668789051521523,0.397750328889649,
-0.917570747950388));
#32527=CARTESIAN_POINT('Ctrl Pts',(0.402637719871008,0.665858082479754,
-0.907136785347906));
#32528=CARTESIAN_POINT('Ctrl Pts',(0.0415808928872853,0.777016826591823,
-0.896702822745427));
#32529=CARTESIAN_POINT('Ctrl Pts',(-0.329276941530812,0.705025400441648,
-0.886268860142945));
#32530=CARTESIAN_POINT('Ctrl Pts',(-0.622521105437113,0.466852859850312,
-0.875834897540466));
#32531=CARTESIAN_POINT('Ctrl Pts',(-0.735437461077155,0.198481764760452,
-0.867793369119612));
#32532=CARTESIAN_POINT('Ctrl Pts',(-0.747503455677645,0.038157886060821,
-0.86322982823292));
#32533=CARTESIAN_POINT('Ctrl Pts',(-0.747472002174668,1.61159471936609E-5,
-0.862144274880388));
#32534=CARTESIAN_POINT('Ctrl Pts',(-0.747471187093045,-1.59917937688492E-5,
-0.989303093540664));
#32535=CARTESIAN_POINT('Ctrl Pts',(-0.747502606642687,-0.0384803988601526,
-0.988208361029073));
#32536=CARTESIAN_POINT('Ctrl Pts',(-0.735309243690986,-0.199127278369176,
-0.983635640983321));
#32537=CARTESIAN_POINT('Ctrl Pts',(-0.621916351700688,-0.467658178639457,
-0.975584933403408));
#32538=CARTESIAN_POINT('Ctrl Pts',(-0.328364174807739,-0.705450981188055,
-0.965150970800928));
#32539=CARTESIAN_POINT('Ctrl Pts',(0.0425865250681795,-0.776962359283856,
-0.954717008198448));
#32540=CARTESIAN_POINT('Ctrl Pts',(0.403499180542327,-0.665336403825431,
-0.944283045595967));
#32541=CARTESIAN_POINT('Ctrl Pts',(0.669303286159028,-0.39688440440999,
-0.933849082993487));
#32542=CARTESIAN_POINT('Ctrl Pts',(0.777346315469044,-0.0348830195569227,
-0.923415120391006));
#32543=CARTESIAN_POINT('Ctrl Pts',(0.702161510858137,0.335340620697416,
-0.912981157788526));
#32544=CARTESIAN_POINT('Ctrl Pts',(0.461470637519422,0.626521324425118,
-0.902547195186045));
#32545=CARTESIAN_POINT('Ctrl Pts',(0.112006796904714,0.770025062366403,
-0.892113232583564));
#32546=CARTESIAN_POINT('Ctrl Pts',(-0.263858098652974,0.732026654580471,
-0.881679269981083));
#32547=CARTESIAN_POINT('Ctrl Pts',(-0.577529159980994,0.521482682939162,
-0.871245307378604));
#32548=CARTESIAN_POINT('Ctrl Pts',(-0.72534176137517,0.24385860707159,-0.862558511723024));
#32549=CARTESIAN_POINT('Ctrl Pts',(-0.747441135558977,0.0608213670538152,
-0.857349703601606));
#32550=CARTESIAN_POINT('Ctrl Pts',(-0.747440403350747,2.49991181703463E-7,
-0.855618883014348));
#32551=CARTESIAN_POINT('Origin',(0.,0.,-1.33003901172249));
#32552=CARTESIAN_POINT('',(-0.7475,-1.95907305151415E-14,-1.12625));
#32553=CARTESIAN_POINT('',(-0.747536615034749,-1.54000427280421E-5,-1.12298730406698));
#32554=CARTESIAN_POINT('',(-0.7475,-1.95907305151415E-14,-1.33003901172249));
#32555=CARTESIAN_POINT('',(-0.738728321778977,-0.114178441930235,-1.12625));
#32556=CARTESIAN_POINT('Origin',(0.,0.,-1.12625));
#32557=CARTESIAN_POINT('Ctrl Pts',(-0.738728321778978,-0.114178441930233,
-1.12625));
#32558=CARTESIAN_POINT('Ctrl Pts',(-0.720064014057805,-0.23493549980332,
-1.12277201246584));
#32559=CARTESIAN_POINT('Ctrl Pts',(-0.622428467720143,-0.467011987146764,
-1.11581603739752));
#32560=CARTESIAN_POINT('Ctrl Pts',(-0.329058176975965,-0.705127368582219,
-1.10538207479504));
#32561=CARTESIAN_POINT('Ctrl Pts',(0.0417919283474094,-0.777000661774149,
-1.09494811219256));
#32562=CARTESIAN_POINT('Ctrl Pts',(0.402831360764579,-0.665746034504356,
-1.08451414959008));
#32563=CARTESIAN_POINT('Ctrl Pts',(0.668899442574653,-0.397559467050135,
-1.0740801869876));
#32564=CARTESIAN_POINT('Ctrl Pts',(0.777311895666571,-0.0356691406410416,
-1.06364622438512));
#32565=CARTESIAN_POINT('Ctrl Pts',(0.702499416237836,0.334631148448012,
-1.05321226178264));
#32566=CARTESIAN_POINT('Ctrl Pts',(0.46210386898375,0.626054505003765,-1.04277829918015));
#32567=CARTESIAN_POINT('Ctrl Pts',(0.112784749994036,0.769911552166375,
-1.03234433657768));
#32568=CARTESIAN_POINT('Ctrl Pts',(-0.26311811085717,0.732292892594134,
-1.02191037397519));
#32569=CARTESIAN_POINT('Ctrl Pts',(-0.577001907123836,0.522066075167687,
-1.01147641137271));
#32570=CARTESIAN_POINT('Ctrl Pts',(-0.72521712885417,0.24436255769002,-1.00278244851655));
#32571=CARTESIAN_POINT('Ctrl Pts',(-0.747440482166499,0.0610730017965627,
-0.997566473194546));
#32572=CARTESIAN_POINT('Ctrl Pts',(-0.747440394010334,2.88097106414253E-8,
-0.995828485406703));
#32573=CARTESIAN_POINT('Ctrl Pts',(-0.747536615034749,-1.54000427279987E-5,
-1.12298730406698));
#32574=CARTESIAN_POINT('Ctrl Pts',(-0.747549574643972,-0.0155531187576177,
-1.1225450059907));
#32575=CARTESIAN_POINT('Ctrl Pts',(-0.743340401009097,-0.153262521212319,
-1.11862472038026));
#32576=CARTESIAN_POINT('Ctrl Pts',(-0.662248238305507,-0.408538693637011,
-1.11122644723566));
#32577=CARTESIAN_POINT('Ctrl Pts',(-0.391780881856493,-0.672308433025167,
-1.10079248463318));
#32578=CARTESIAN_POINT('Ctrl Pts',(-0.0289685614302378,-0.777586532369439,
-1.0903585220307));
#32579=CARTESIAN_POINT('Ctrl Pts',(0.34067266544482,-0.699591456600571,
-1.07992455942821));
#32580=CARTESIAN_POINT('Ctrl Pts',(0.630013764781801,-0.456690366635246,
-1.06949059682574));
#32581=CARTESIAN_POINT('Ctrl Pts',(0.770854889346008,-0.10614597677494,
-1.05905663422325));
#32582=CARTESIAN_POINT('Ctrl Pts',(0.729998172573568,0.269419497799131,
-1.04862267162077));
#32583=CARTESIAN_POINT('Ctrl Pts',(0.517074073818031,0.581479511865621,
-1.03818870901829));
#32584=CARTESIAN_POINT('Ctrl Pts',(0.182270729955255,0.756479721113076,
-1.02775474641581));
#32585=CARTESIAN_POINT('Ctrl Pts',(-0.195495525574094,0.753170354596226,
-1.01732078381333));
#32586=CARTESIAN_POINT('Ctrl Pts',(-0.527181654493517,0.572331754114923,
-1.00688682121085));
#32587=CARTESIAN_POINT('Ctrl Pts',(-0.712843111741136,0.289716880061177,
-0.997547591119961));
#32588=CARTESIAN_POINT('Ctrl Pts',(-0.747402786092163,0.083721807495523,
-0.991686348563233));
#32589=CARTESIAN_POINT('Ctrl Pts',(-0.747471187093045,-1.59917937688492E-5,
-0.989303093540664));
#32590=CARTESIAN_POINT('Ctrl Pts',(0.82685,-3.02682447659827E-15,-1.12625));
#32591=CARTESIAN_POINT('Ctrl Pts',(0.82685,0.135161967341268,-1.12277201246584));
#32592=CARTESIAN_POINT('Ctrl Pts',(0.759329854291358,0.405358483866949,
-1.11581603739752));
#32593=CARTESIAN_POINT('Ctrl Pts',(0.478857035684594,0.715228292912727,
-1.10538207479504));
#32594=CARTESIAN_POINT('Ctrl Pts',(0.0855976892416237,0.85645773182655,
-1.09494811219256));
#32595=CARTESIAN_POINT('Ctrl Pts',(-0.327878991306296,0.795839011623234,
-1.08451414959008));
#32596=CARTESIAN_POINT('Ctrl Pts',(-0.664050737432062,0.547619885496961,
-1.0740801869876));
#32597=CARTESIAN_POINT('Ctrl Pts',(-0.84371003918773,0.170328555651515,
-1.06364622438512));
#32598=CARTESIAN_POINT('Ctrl Pts',(-0.824493582456408,-0.247114352893222,
-1.05321226178264));
#32599=CARTESIAN_POINT('Ctrl Pts',(-0.610938970960343,-0.606308285553784,
-1.04277829918015));
#32600=CARTESIAN_POINT('Ctrl Pts',(-0.253378910006021,-0.82259057174209,
-1.03234433657767));
#32601=CARTESIAN_POINT('Ctrl Pts',(0.163904234062435,-0.844980061330928,
-1.02191037397519));
#32602=CARTESIAN_POINT('Ctrl Pts',(0.542553969616097,-0.668200044521288,
-1.01147641137271));
#32603=CARTESIAN_POINT('Ctrl Pts',(0.793318450980058,-0.333918875136032,
-1.00104244877023));
#32604=CARTESIAN_POINT('Ctrl Pts',(0.857090409214355,0.0790700506594116,
-0.990608486167751));
#32605=CARTESIAN_POINT('Ctrl Pts',(0.718838053513711,0.47342145348791,-0.980174523565272));
#32606=CARTESIAN_POINT('Ctrl Pts',(0.411148835382881,0.756182953459404,
-0.96974056096279));
#32607=CARTESIAN_POINT('Ctrl Pts',(0.00654795948643633,0.860705030962387,
-0.959306598360311));
#32608=CARTESIAN_POINT('Ctrl Pts',(-0.399596325757394,0.762350837560662,
-0.948872635757829));
#32609=CARTESIAN_POINT('Ctrl Pts',(-0.711552003832336,0.484303387427028,
-0.938438673155349));
#32610=CARTESIAN_POINT('Ctrl Pts',(-0.855788184097908,0.0921010751558475,
-0.928004710552867));
#32611=CARTESIAN_POINT('Ctrl Pts',(-0.798307045430395,-0.321810325775008,
-0.917570747950388));
#32612=CARTESIAN_POINT('Ctrl Pts',(-0.552657431316075,-0.659868008045783,
-0.907136785347907));
#32613=CARTESIAN_POINT('Ctrl Pts',(-0.176741265643768,-0.842388597645021,
-0.896702822745426));
#32614=CARTESIAN_POINT('Ctrl Pts',(0.240834477891075,-0.826350276046737,
-0.886268860142946));
#32615=CARTESIAN_POINT('Ctrl Pts',(0.60164327098714,-0.615533426310556,
-0.875834897540465));
#32616=CARTESIAN_POINT('Ctrl Pts',(0.820639089442,-0.259629561740577,-0.865400934937984));
#32617=CARTESIAN_POINT('Ctrl Pts',(0.846202560151336,0.15747143116726,-0.854966972335505));
#32618=CARTESIAN_POINT('Ctrl Pts',(0.672308132783287,0.537454927447039,
-0.844533009733023));
#32619=CARTESIAN_POINT('Ctrl Pts',(0.339944358537648,0.790755245029512,
-0.834099047130544));
#32620=CARTESIAN_POINT('Ctrl Pts',(-0.0725474966321842,0.857667117928167,
-0.823665084528062));
#32621=CARTESIAN_POINT('Ctrl Pts',(-0.467939224870045,0.722418788703156,
-0.813231121925582));
#32622=CARTESIAN_POINT('Ctrl Pts',(-0.75303327898166,0.416889559942562,
-0.802797159323101));
#32623=CARTESIAN_POINT('Ctrl Pts',(-0.860630310410644,0.0130955429679302,
-0.79236319672062));
#32624=CARTESIAN_POINT('Ctrl Pts',(-0.765368687391838,-0.393785216587893,
-0.78192923411814));
#32625=CARTESIAN_POINT('Ctrl Pts',(-0.489702469969954,-0.70784709884863,
-0.771495271515659));
#32626=CARTESIAN_POINT('Ctrl Pts',(-0.0986087769686508,-0.855062765852803,
-0.761061308913178));
#32627=CARTESIAN_POINT('Ctrl Pts',(0.315727931727778,-0.800732100998825,
-0.750627346310699));
#32628=CARTESIAN_POINT('Ctrl Pts',(0.655644598941733,-0.557661352723703,
-0.740193383708217));
#32629=CARTESIAN_POINT('Ctrl Pts',(0.841019670852427,-0.183144581362294,
-0.729759421105737));
#32630=CARTESIAN_POINT('Ctrl Pts',(0.828158500407521,0.234541089461659,
-0.719325458503256));
#32631=CARTESIAN_POINT('Ctrl Pts',(0.620092586381243,0.596943220715435,
-0.708891495900776));
#32632=CARTESIAN_POINT('Ctrl Pts',(0.265865020615963,0.818640223331329,
-0.698457533298294));
#32633=CARTESIAN_POINT('Ctrl Pts',(-0.151029429750584,0.847376029748488,
-0.688023570695815));
#32634=CARTESIAN_POINT('Ctrl Pts',(-0.532324823785286,0.676377340265815,
-0.677589608093333));
#32635=CARTESIAN_POINT('Ctrl Pts',(-0.788146252778427,0.345950153453385,
-0.667155645490854));
#32636=CARTESIAN_POINT('Ctrl Pts',(-0.858194201088188,-0.0660207366037423,
-0.656721682888372));
#32637=CARTESIAN_POINT('Ctrl Pts',(-0.725957708818034,-0.462429918420906,
-0.646287720285892));
#32638=CARTESIAN_POINT('Ctrl Pts',(-0.422606160274219,-0.749840021432156,
-0.635853757683412));
#32639=CARTESIAN_POINT('Ctrl Pts',(-0.0196423670795997,-0.860505782582898,
-0.625419795080931));
#32640=CARTESIAN_POINT('Ctrl Pts',(0.387951316682125,-0.768342241665588,
-0.61498583247845));
#32641=CARTESIAN_POINT('Ctrl Pts',(0.704101228197687,-0.495073211650161,
-0.604551869875969));
#32642=CARTESIAN_POINT('Ctrl Pts',(0.854287861381835,-0.105110771754113,
-0.594117907273489));
#32643=CARTESIAN_POINT('Ctrl Pts',(0.803110814976077,0.309627265129475,
-0.583683944671009));
#32644=CARTESIAN_POINT('Ctrl Pts',(0.562632999903826,0.651383244996612,
-0.573249982068528));
#32645=CARTESIAN_POINT('Ctrl Pts',(0.189537297769379,0.839602070743859,
-0.562816019466046));
#32646=CARTESIAN_POINT('Ctrl Pts',(-0.228234127178964,0.829918795807127,
-0.552382056863568));
#32647=CARTESIAN_POINT('Ctrl Pts',(-0.592208622855233,0.624615859115826,
-0.541948094261085));
#32648=CARTESIAN_POINT('Ctrl Pts',(-0.816593979116471,0.272085092781331,
-0.531514131658606));
#32649=CARTESIAN_POINT('Ctrl Pts',(-0.848500458175959,-0.14457868763508,
-0.521080169056125));
#32650=CARTESIAN_POINT('Ctrl Pts',(-0.68040740298517,-0.527163912275938,
-0.510646206453644));
#32651=CARTESIAN_POINT('Ctrl Pts',(-0.351935926797396,-0.785491647232708,
-0.500212243851164));
#32652=CARTESIAN_POINT('Ctrl Pts',(0.0594901556810227,-0.858671616987626,
-0.489778281248683));
#32653=CARTESIAN_POINT('Ctrl Pts',(0.456893849233147,-0.729454614747217,
-0.479344318646202));
#32654=CARTESIAN_POINT('Ctrl Pts',(0.746603367528272,-0.428298302633273,
-0.468910356043722));
#32655=CARTESIAN_POINT('Ctrl Pts',(0.86033145371393,-0.026188054405967,
-0.458476393441242));
#32656=CARTESIAN_POINT('Ctrl Pts',(0.771271328784717,0.382094964423424,
-0.44804243083876));
#32657=CARTESIAN_POINT('Ctrl Pts',(0.500415301388769,0.700314608286257,
-0.43760846823628));
#32658=CARTESIAN_POINT('Ctrl Pts',(0.111606683342934,0.853463515726457,
-0.427174505633799));
#32659=CARTESIAN_POINT('Ctrl Pts',(-0.303508679116189,0.805443049597213,
-0.416740543031319));
#32660=CARTESIAN_POINT('Ctrl Pts',(-0.647084192799484,0.567572085176716,
-0.406306580428838));
#32661=CARTESIAN_POINT('Ctrl Pts',(-0.838135879378579,0.195919044866888,
-0.395872617826358));
#32662=CARTESIAN_POINT('Ctrl Pts',(-0.831631060361419,-0.221913956041062,
-0.385438655223877));
#32663=CARTESIAN_POINT('Ctrl Pts',(-0.629102982738006,-0.587439751421952,
-0.375004692621396));
#32664=CARTESIAN_POINT('Ctrl Pts',(-0.27828941825328,-0.814500475222728,
-0.364570730018916));
#32665=CARTESIAN_POINT('Ctrl Pts',(0.138119578151258,-0.849575780352193,
-0.354136767416435));
#32666=CARTESIAN_POINT('Ctrl Pts',(0.521972491602107,-0.68439808771962,
-0.343702804813955));
#32667=CARTESIAN_POINT('Ctrl Pts',(0.782791582026738,-0.357901332117923,
-0.333268842211474));
#32668=CARTESIAN_POINT('Ctrl Pts',(0.859099337993374,0.0529561317558155,
-0.322834879608993));
#32669=CARTESIAN_POINT('Ctrl Pts',(0.732909304116493,0.451331337820343,
-0.312400917006513));
#32670=CARTESIAN_POINT('Ctrl Pts',(0.433965657579446,0.743323504356007,
-0.301966954404032));
#32671=CARTESIAN_POINT('Ctrl Pts',(0.0327322261453305,0.860107334350009,
-0.291532991801552));
#32672=CARTESIAN_POINT('Ctrl Pts',(-0.376216498791157,0.774155778332486,
-0.281099029199071));
#32673=CARTESIAN_POINT('Ctrl Pts',(-0.696487458167497,0.505728431782095,
-0.27066506659659));
#32674=CARTESIAN_POINT('Ctrl Pts',(-0.85258977678019,0.11809613232106,-0.26023110399411));
#32675=CARTESIAN_POINT('Ctrl Pts',(-0.807728669522179,-0.297372520979856,
-0.249797141391629));
#32676=CARTESIAN_POINT('Ctrl Pts',(-0.572478323412184,-0.642747704547972,
-0.239363178789149));
#32677=CARTESIAN_POINT('Ctrl Pts',(-0.202289451911266,-0.836621155292497,
-0.228929216186668));
#32678=CARTESIAN_POINT('Ctrl Pts',(0.215580939060966,-0.833295246691129,
-0.218495253584187));
#32679=CARTESIAN_POINT('Ctrl Pts',(0.582636887836429,-0.633553595935411,
-0.208061290981707));
#32680=CARTESIAN_POINT('Ctrl Pts',(0.812359822146787,-0.284477837654288,
-0.197627328379226));
#32681=CARTESIAN_POINT('Ctrl Pts',(0.850601954996979,0.131652867513652,
-0.187193365776746));
#32682=CARTESIAN_POINT('Ctrl Pts',(0.688349122337921,0.51675009114102,-0.176759403174265));
#32683=CARTESIAN_POINT('Ctrl Pts',(0.363846105084835,0.780047728610939,
-0.166325440571784));
#32684=CARTESIAN_POINT('Ctrl Pts',(-0.0464192020363249,0.859474361780549,
-0.155891477969304));
#32685=CARTESIAN_POINT('Ctrl Pts',(-0.445742392858126,0.736327430271745,
-0.145457515366823));
#32686=CARTESIAN_POINT('Ctrl Pts',(-0.740001245121628,0.439596369442954,
-0.135023552764343));
#32687=CARTESIAN_POINT('Ctrl Pts',(-0.859832124525603,0.0392974457347639,
-0.124589590161862));
#32688=CARTESIAN_POINT('Ctrl Pts',(-0.776998977184784,-0.370364573784867,
-0.114155627559381));
#32689=CARTESIAN_POINT('Ctrl Pts',(-0.599661254481026,-0.585112006191809,
-0.107199652491061));
#32690=CARTESIAN_POINT('Ctrl Pts',(-0.490897892427245,-0.665357183556688,
-0.103721664956901));
#32691=CARTESIAN_POINT('Ctrl Pts',(0.82685,-3.02682447659827E-15,-1.12910983122651));
#32692=CARTESIAN_POINT('Ctrl Pts',(0.82685,0.135162380594788,-1.12563184369234));
#32693=CARTESIAN_POINT('Ctrl Pts',(0.759329891769105,0.405358236621017,
-1.11867586862402));
#32694=CARTESIAN_POINT('Ctrl Pts',(0.478857042724245,0.715228435638403,
-1.10824190602154));
#32695=CARTESIAN_POINT('Ctrl Pts',(0.0855976953161789,0.856457696102362,
-1.09780794341906));
#32696=CARTESIAN_POINT('Ctrl Pts',(-0.327879002777267,0.795839066043265,
-1.08737398081658));
#32697=CARTESIAN_POINT('Ctrl Pts',(-0.664050756097956,0.547619885902201,
-1.0769400182141));
#32698=CARTESIAN_POINT('Ctrl Pts',(-0.843710064534722,0.1703285686858,-1.06650605561162));
#32699=CARTESIAN_POINT('Ctrl Pts',(-0.824493606532926,-0.247114364257445,
-1.05607209300914));
#32700=CARTESIAN_POINT('Ctrl Pts',(-0.610938989097404,-0.606308301358732,
-1.04563813040666));
#32701=CARTESIAN_POINT('Ctrl Pts',(-0.253378917416559,-0.822590597055703,
-1.03520416780418));
#32702=CARTESIAN_POINT('Ctrl Pts',(0.163904238864601,-0.84498008571162,
-1.0247702052017));
#32703=CARTESIAN_POINT('Ctrl Pts',(0.542553985631648,-0.6682000644996,-1.01433624259922));
#32704=CARTESIAN_POINT('Ctrl Pts',(0.793318474366499,-0.333918884843967,
-1.00390227999674));
#32705=CARTESIAN_POINT('Ctrl Pts',(0.857090434493622,0.0790700529203285,
-0.993468317394256));
#32706=CARTESIAN_POINT('Ctrl Pts',(0.718838074709768,0.473421467484897,
-0.983034354791778));
#32707=CARTESIAN_POINT('Ctrl Pts',(0.411148847508511,0.756182975740501,
-0.972600392189296));
#32708=CARTESIAN_POINT('Ctrl Pts',(0.00654795967898853,0.860705056353458,
-0.962166429586816));
#32709=CARTESIAN_POINT('Ctrl Pts',(-0.399596337541002,0.762350860037237,
-0.951732466984335));
#32710=CARTESIAN_POINT('Ctrl Pts',(-0.711552024815771,0.484303401711296,
-0.941298504381855));
#32711=CARTESIAN_POINT('Ctrl Pts',(-0.855788209334578,0.09210107787063,
-0.930864541779373));
#32712=CARTESIAN_POINT('Ctrl Pts',(-0.798307068972085,-0.321810335264399,
-0.920430579176894));
#32713=CARTESIAN_POINT('Ctrl Pts',(-0.552657447613633,-0.659868027505261,
-0.909996616574413));
#32714=CARTESIAN_POINT('Ctrl Pts',(-0.176741270855785,-0.842388622486455,
-0.899562653971931));
#32715=CARTESIAN_POINT('Ctrl Pts',(0.240834484993162,-0.826350300415453,
-0.889128691369452));
#32716=CARTESIAN_POINT('Ctrl Pts',(0.60164328872928,-0.61553344446227,-0.878694728766969));
#32717=CARTESIAN_POINT('Ctrl Pts',(0.820639113642216,-0.259629569396937,
-0.868260766164492));
#32718=CARTESIAN_POINT('Ctrl Pts',(0.846202585105402,0.15747143581102,-0.857826803562008));
#32719=CARTESIAN_POINT('Ctrl Pts',(0.6723081526093,0.537454943296297,-0.847392840959531));
#32720=CARTESIAN_POINT('Ctrl Pts',(0.339944368562428,0.79075526834847,-0.836958878357048));
#32721=CARTESIAN_POINT('Ctrl Pts',(-0.0725474987715713,0.857667143220318,
-0.826524915754568));
#32722=CARTESIAN_POINT('Ctrl Pts',(-0.467939238669326,0.722418810006905,
-0.816090953152087));
#32723=CARTESIAN_POINT('Ctrl Pts',(-0.753033301188214,0.416889572236416,
-0.805656990549607));
#32724=CARTESIAN_POINT('Ctrl Pts',(-0.860630335790178,0.0130955433541108,
-0.795223027947126));
#32725=CARTESIAN_POINT('Ctrl Pts',(-0.765368709962158,-0.393785228200412,
-0.784789065344646));
#32726=CARTESIAN_POINT('Ctrl Pts',(-0.489702484411021,-0.707847119722667,
-0.774355102742164));
#32727=CARTESIAN_POINT('Ctrl Pts',(-0.0986087798765718,-0.855062791068153,
-0.763921140139686));
#32728=CARTESIAN_POINT('Ctrl Pts',(0.315727941038429,-0.800732124611992,
-0.753487177537203));
#32729=CARTESIAN_POINT('Ctrl Pts',(0.655644618276346,-0.557661369168842,
-0.743053214934723));
#32730=CARTESIAN_POINT('Ctrl Pts',(0.841019695653653,-0.183144586763131,
-0.732619252332243));
#32731=CARTESIAN_POINT('Ctrl Pts',(0.828158524829479,0.234541096378151,
-0.722185289729762));
#32732=CARTESIAN_POINT('Ctrl Pts',(0.620092604667446,0.596943238318976,
-0.711751327127282));
#32733=CARTESIAN_POINT('Ctrl Pts',(0.265865028456182,0.818640247472598,
-0.7013173645248));
#32734=CARTESIAN_POINT('Ctrl Pts',(-0.151029434204362,0.847376054737159,
-0.690883401922321));
#32735=CARTESIAN_POINT('Ctrl Pts',(-0.532324839483263,0.676377360211827,
-0.680449439319839));
#32736=CARTESIAN_POINT('Ctrl Pts',(-0.788146276020444,0.345950163655273,
-0.670015476717359));
#32737=CARTESIAN_POINT('Ctrl Pts',(-0.858194226395883,-0.0660207385506592,
-0.659581514114878));
#32738=CARTESIAN_POINT('Ctrl Pts',(-0.725957730226144,-0.46242993205772,
-0.649147551512398));
#32739=CARTESIAN_POINT('Ctrl Pts',(-0.422606172736652,-0.749840043544544,
-0.638713588909917));
#32740=CARTESIAN_POINT('Ctrl Pts',(-0.0196423676588426,-0.860505807958758,
-0.628279626307437));
#32741=CARTESIAN_POINT('Ctrl Pts',(0.387951328122605,-0.768342264323596,
-0.617845663704956));
#32742=CARTESIAN_POINT('Ctrl Pts',(0.70410124896126,-0.495073226249608,
-0.607411701102476));
#32743=CARTESIAN_POINT('Ctrl Pts',(0.854287886574333,-0.105110774853774,
-0.596977738499994));
#32744=CARTESIAN_POINT('Ctrl Pts',(0.803110838659391,0.309627274260219,
-0.586543775897515));
#32745=CARTESIAN_POINT('Ctrl Pts',(0.562633016495577,0.65138326420556,-0.576109813295033));
#32746=CARTESIAN_POINT('Ctrl Pts',(0.189537303358733,0.839602095503281,
-0.565675850692553));
#32747=CARTESIAN_POINT('Ctrl Pts',(-0.228234133909468,0.829918820280995,
-0.555241888090073));
#32748=CARTESIAN_POINT('Ctrl Pts',(-0.592208640319154,0.624615877535418,
-0.544807925487591));
#32749=CARTESIAN_POINT('Ctrl Pts',(-0.816594003197396,0.272085100804978,
-0.534373962885111));
#32750=CARTESIAN_POINT('Ctrl Pts',(-0.84850048319779,-0.14457869189863,
-0.523940000282631));
#32751=CARTESIAN_POINT('Ctrl Pts',(-0.680407423050025,-0.527163927821724,
-0.513506037680149));
#32752=CARTESIAN_POINT('Ctrl Pts',(-0.351935937175801,-0.785491670396441,
-0.503072075077669));
#32753=CARTESIAN_POINT('Ctrl Pts',(0.0594901574353558,-0.8586716423094,
-0.492638112475189));
#32754=CARTESIAN_POINT('Ctrl Pts',(0.456893862706706,-0.729454636258448,
-0.482204149872708));
#32755=CARTESIAN_POINT('Ctrl Pts',(0.746603389545211,-0.428298315263564,
-0.471770187270228));
#32756=CARTESIAN_POINT('Ctrl Pts',(0.860331479084652,-0.0261880551782389,
-0.461336224667747));
#32757=CARTESIAN_POINT('Ctrl Pts',(0.771271351529101,0.382094975691203,
-0.450902262065267));
#32758=CARTESIAN_POINT('Ctrl Pts',(0.500415316145753,0.700314628938165,
-0.440468299462785));
#32759=CARTESIAN_POINT('Ctrl Pts',(0.111606686634156,0.853463540894646,
-0.430034336860305));
#32760=CARTESIAN_POINT('Ctrl Pts',(-0.3035086880665,0.805443073349304,-0.419600374257825));
#32761=CARTESIAN_POINT('Ctrl Pts',(-0.647084211881655,0.567572101914117,
-0.409166411655343));
#32762=CARTESIAN_POINT('Ctrl Pts',(-0.838135904094766,0.195919050644438,
-0.398732449052864));
#32763=CARTESIAN_POINT('Ctrl Pts',(-0.831631084885775,-0.22191396258519,
-0.388298486450382));
#32764=CARTESIAN_POINT('Ctrl Pts',(-0.62910300128993,-0.587439768745234,
-0.377864523847903));
#32765=CARTESIAN_POINT('Ctrl Pts',(-0.278289426459872,-0.814500499241931,
-0.367430561245421));
#32766=CARTESIAN_POINT('Ctrl Pts',(0.138119582224299,-0.849575805405708,
-0.356996598642941));
#32767=CARTESIAN_POINT('Ctrl Pts',(0.521972506994863,-0.684398107902212,
-0.346562636040461));
#32768=CARTESIAN_POINT('Ctrl Pts',(0.782791605110725,-0.357901342672141,
-0.336128673437979));
#32769=CARTESIAN_POINT('Ctrl Pts',(0.859099363328006,0.05295613331726,-0.3256947108355));
#32770=CARTESIAN_POINT('Ctrl Pts',(0.73290932572912,0.451331351130267,-0.315260748233018));
#32771=CARTESIAN_POINT('Ctrl Pts',(0.433965670377812,0.743323526275438,
-0.304826785630539));
#32772=CARTESIAN_POINT('Ctrl Pts',(0.0327322271087253,0.860107359715668,
-0.294392823028057));
#32773=CARTESIAN_POINT('Ctrl Pts',(-0.376216509881926,0.774155801158889,
-0.283958860425577));
#32774=CARTESIAN_POINT('Ctrl Pts',(-0.696487478713732,0.505728446701738,
-0.273524897823096));
#32775=CARTESIAN_POINT('Ctrl Pts',(-0.85258980190849,0.118096135791905,
-0.263090935220616));
#32776=CARTESIAN_POINT('Ctrl Pts',(-0.807728693369426,-0.297372529726131,
-0.252656972618135));
#32777=CARTESIAN_POINT('Ctrl Pts',(-0.57247834023973,-0.642747723547624,
-0.242223010015654));
#32778=CARTESIAN_POINT('Ctrl Pts',(-0.202289457983844,-0.836621179874877,
-0.231789047413174));
#32779=CARTESIAN_POINT('Ctrl Pts',(0.21558094562892,-0.83329527143972,-0.221355084810693));
#32780=CARTESIAN_POINT('Ctrl Pts',(0.582636904604278,-0.633553614274392,
-0.210921122208213));
#32781=CARTESIAN_POINT('Ctrl Pts',(0.812359846915985,-0.284477846719709,
-0.200487159605732));
#32782=CARTESIAN_POINT('Ctrl Pts',(0.850601978482959,0.131652872725006,
-0.190053197003252));
#32783=CARTESIAN_POINT('Ctrl Pts',(0.68834914577673,0.516750103768234,-0.179619234400771));
#32784=CARTESIAN_POINT('Ctrl Pts',(0.363846109644706,0.780047756745796,
-0.16918527179829));
#32785=CARTESIAN_POINT('Ctrl Pts',(-0.0464191912805425,0.859474377041381,
-0.158751309195809));
#32786=CARTESIAN_POINT('Ctrl Pts',(-0.445742429839058,0.736327471811288,
-0.148317346593329));
#32787=CARTESIAN_POINT('Ctrl Pts',(-0.740001219981202,0.439596343345502,
-0.137883383990848));
#32788=CARTESIAN_POINT('Ctrl Pts',(-0.859832243554816,0.0392975248057583,
-0.127449421388368));
#32789=CARTESIAN_POINT('Ctrl Pts',(-0.776998800479081,-0.370364750731827,
-0.117015458785887));
#32790=CARTESIAN_POINT('Ctrl Pts',(-0.599661587021631,-0.58511176084467,
-0.110059483717567));
#32791=CARTESIAN_POINT('Ctrl Pts',(-0.490897892427245,-0.665357183556688,
-0.106581496183406));
#32792=CARTESIAN_POINT('Ctrl Pts',(0.825266255435535,-3.02102691136588E-15,
-1.13578682154469));
#32793=CARTESIAN_POINT('Ctrl Pts',(0.825266255435536,0.134902373133398,
-1.13230883401052));
#32794=CARTESIAN_POINT('Ctrl Pts',(0.75787537350136,0.40458248431603,-1.12535285894221));
#32795=CARTESIAN_POINT('Ctrl Pts',(0.477939823171875,0.713858104336506,
-1.11491889633972));
#32796=CARTESIAN_POINT('Ctrl Pts',(0.0854337254619215,0.854817337751033,
-1.10448493373724));
#32797=CARTESIAN_POINT('Ctrl Pts',(-0.327250953856659,0.794314572438199,
-1.09405097113476));
#32798=CARTESIAN_POINT('Ctrl Pts',(-0.662778785930793,0.546570976276213,
-1.08361700853228));
#32799=CARTESIAN_POINT('Ctrl Pts',(-0.842093957705064,0.170002286889038,
-1.0731830459298));
#32800=CARTESIAN_POINT('Ctrl Pts',(-0.822914310253025,-0.246641011830834,
-1.06274908332732));
#32801=CARTESIAN_POINT('Ctrl Pts',(-0.609768750387387,-0.605146938555681,
-1.05231512072484));
#32802=CARTESIAN_POINT('Ctrl Pts',(-0.252893576591472,-0.821014942444097,
-1.04188115812236));
#32803=CARTESIAN_POINT('Ctrl Pts',(0.163590284471113,-0.843361548903803,
-1.03144719551988));
#32804=CARTESIAN_POINT('Ctrl Pts',(0.541514736972467,-0.666920143216008,
-1.0210132329174));
#32805=CARTESIAN_POINT('Ctrl Pts',(0.791798892653785,-0.333279271931911,
-1.01057927031492));
#32806=CARTESIAN_POINT('Ctrl Pts',(0.855448699150101,0.0789185963993257,
-1.00014530771244));
#32807=CARTESIAN_POINT('Ctrl Pts',(0.717461158327155,0.47251464038409,-0.989711345109957));
#32808=CARTESIAN_POINT('Ctrl Pts',(0.41036130215142,0.754734526176119,-0.979277382507476));
#32809=CARTESIAN_POINT('Ctrl Pts',(0.00653541722714587,0.859056397277897,
-0.968843419904996));
#32810=CARTESIAN_POINT('Ctrl Pts',(-0.398830920732015,0.76089059600768,
-0.958409457302514));
#32811=CARTESIAN_POINT('Ctrl Pts',(-0.710189064673796,0.483375730628082,
-0.947975494700035));
#32812=CARTESIAN_POINT('Ctrl Pts',(-0.854148968382192,0.0919246605583472,
-0.937541532097554));
#32813=CARTESIAN_POINT('Ctrl Pts',(-0.796777931708911,-0.321193915602005,
-0.927107569495074));
#32814=CARTESIAN_POINT('Ctrl Pts',(-0.551598846068353,-0.658604066769503,
-0.916673606892593));
#32815=CARTESIAN_POINT('Ctrl Pts',(-0.176402727363294,-0.840775048108438,
-0.906239644290112));
#32816=CARTESIAN_POINT('Ctrl Pts',(0.240373172548915,-0.824767447042348,
-0.895805681687632));
#32817=CARTESIAN_POINT('Ctrl Pts',(0.600490856028098,-0.614354405514617,
-0.88537171908515));
#32818=CARTESIAN_POINT('Ctrl Pts',(0.819067199905029,-0.259132255437638,
-0.874937756482672));
#32819=CARTESIAN_POINT('Ctrl Pts',(0.844581705176757,0.157169803206536,
-0.864503793880189));
#32820=CARTESIAN_POINT('Ctrl Pts',(0.6710203631253,0.536425461768513,-0.85406983127771));
#32821=CARTESIAN_POINT('Ctrl Pts',(0.339293213610224,0.789240596370972,
-0.843635868675228));
#32822=CARTESIAN_POINT('Ctrl Pts',(-0.072408535848624,0.856024303216786,
-0.833201906072748));
#32823=CARTESIAN_POINT('Ctrl Pts',(-0.467042912738471,0.721035034809535,
-0.822767943470268));
#32824=CARTESIAN_POINT('Ctrl Pts',(-0.751590884697194,0.4160910306673,-0.812333980867786));
#32825=CARTESIAN_POINT('Ctrl Pts',(-0.858981819865243,0.0130704591677099,
-0.801900018265307));
#32826=CARTESIAN_POINT('Ctrl Pts',(-0.763902665303551,-0.393030942425559,
-0.791466055662826));
#32827=CARTESIAN_POINT('Ctrl Pts',(-0.488764471526209,-0.706491256234296,
-0.781032093060345));
#32828=CARTESIAN_POINT('Ctrl Pts',(-0.0984198972202151,-0.853424939636155,
-0.770598130457865));
#32829=CARTESIAN_POINT('Ctrl Pts',(0.315123172048649,-0.799198342215373,
-0.760164167855384));
#32830=CARTESIAN_POINT('Ctrl Pts',(0.654388747376404,-0.556593182736683,
-0.749730205252903));
#32831=CARTESIAN_POINT('Ctrl Pts',(0.839408743420373,-0.182793777878888,
-0.739296242650423));
#32832=CARTESIAN_POINT('Ctrl Pts',(0.826572207847869,0.234091838762714,
-0.728862280047942));
#32833=CARTESIAN_POINT('Ctrl Pts',(0.618904832762113,0.595799808447022,
-0.718428317445461));
#32834=CARTESIAN_POINT('Ctrl Pts',(0.265355770630763,0.817072162513667,
-0.707994354842981));
#32835=CARTESIAN_POINT('Ctrl Pts',(-0.150740141093178,0.845752927056724,
-0.697560392240501));
#32836=CARTESIAN_POINT('Ctrl Pts',(-0.531305184541261,0.675081776262243,
-0.687126429638019));
#32837=CARTESIAN_POINT('Ctrl Pts',(-0.786636601502631,0.345287504752486,
-0.676692467035539));
#32838=CARTESIAN_POINT('Ctrl Pts',(-0.856550376777682,-0.065894277473992,
-0.666258504433058));
#32839=CARTESIAN_POINT('Ctrl Pts',(-0.724567176315434,-0.461544159066155,
-0.655824541830578));
#32840=CARTESIAN_POINT('Ctrl Pts',(-0.421796681161976,-0.748403743658829,
-0.645390579228098));
#32841=CARTESIAN_POINT('Ctrl Pts',(-0.01960474319391,-0.858857530563777,
-0.634956616625617));
#32842=CARTESIAN_POINT('Ctrl Pts',(0.387208217037725,-0.766870523895836,
-0.624522654023136));
#32843=CARTESIAN_POINT('Ctrl Pts',(0.702752560594826,-0.49412492584287,
-0.614088691420655));
#32844=CARTESIAN_POINT('Ctrl Pts',(0.85265151945255,-0.104909437788343,
-0.603654728818175));
#32845=CARTESIAN_POINT('Ctrl Pts',(0.801572499895393,0.309034190945368,
-0.593220766215694));
#32846=CARTESIAN_POINT('Ctrl Pts',(0.561555306997066,0.650135555822967,
-0.582786803613213));
#32847=CARTESIAN_POINT('Ctrl Pts',(0.189174249385427,0.837993858647703,
-0.572352841010733));
#32848=CARTESIAN_POINT('Ctrl Pts',(-0.227796957123202,0.828329131497389,
-0.561918878408252));
#32849=CARTESIAN_POINT('Ctrl Pts',(-0.591074279451483,0.623419441413817,
-0.551484915805771));
#32850=CARTESIAN_POINT('Ctrl Pts',(-0.815029837768296,0.271563928586243,
-0.541050953203291));
#32851=CARTESIAN_POINT('Ctrl Pts',(-0.846875201702707,-0.144301755023308,
-0.53061699060081));
#32852=CARTESIAN_POINT('Ctrl Pts',(-0.679104119615673,-0.52615415847718,
-0.520183027998331));
#32853=CARTESIAN_POINT('Ctrl Pts',(-0.351261812673254,-0.783987080709439,
-0.509749065395849));
#32854=CARTESIAN_POINT('Ctrl Pts',(0.0593762055237968,-0.857026878212932,
-0.499315102793369));
#32855=CARTESIAN_POINT('Ctrl Pts',(0.456018693917791,-0.728057384111526,
-0.488881140190888));
#32856=CARTESIAN_POINT('Ctrl Pts',(0.745173289389437,-0.427477920531967,
-0.478447177588408));
#32857=CARTESIAN_POINT('Ctrl Pts',(0.858683535612277,-0.0261378926122579,
-0.468013214985927));
#32858=CARTESIAN_POINT('Ctrl Pts',(0.769794000507915,0.381363082303218,
-0.457579252383447));
#32859=CARTESIAN_POINT('Ctrl Pts',(0.499456783099169,0.698973193747863,
-0.447145289780966));
#32860=CARTESIAN_POINT('Ctrl Pts',(0.111392906811862,0.851828752786434,
-0.436711327178486));
#32861=CARTESIAN_POINT('Ctrl Pts',(-0.302927324750768,0.803900267247975,
-0.426277364576005));
#32862=CARTESIAN_POINT('Ctrl Pts',(-0.645844738226477,0.56648493172078,
-0.415843401973524));
#32863=CARTESIAN_POINT('Ctrl Pts',(-0.836530475692225,0.195543772593505,
-0.405409439371044));
#32864=CARTESIAN_POINT('Ctrl Pts',(-0.830038116302073,-0.221488891929322,
-0.394975476768563));
#32865=CARTESIAN_POINT('Ctrl Pts',(-0.627897970194763,-0.58631454253204,
-0.384541514166082));
#32866=CARTESIAN_POINT('Ctrl Pts',(-0.277756370010263,-0.812940343867362,
-0.374107551563602));
#32867=CARTESIAN_POINT('Ctrl Pts',(0.137855017612411,-0.847948464157851,
-0.363673588961121));
#32868=CARTESIAN_POINT('Ctrl Pts',(0.520972681687152,-0.6830871604105,-0.353239626358641));
#32869=CARTESIAN_POINT('Ctrl Pts',(0.781292187331713,-0.357215791584557,
-0.34280566375616));
#32870=CARTESIAN_POINT('Ctrl Pts',(0.857453779941941,0.0528546971663474,
-0.33237170115368));
#32871=CARTESIAN_POINT('Ctrl Pts',(0.731505456212057,0.450466837192338,
-0.321937738551198));
#32872=CARTESIAN_POINT('Ctrl Pts',(0.4331344199664,0.741899708618019,-0.311503775948718));
#32873=CARTESIAN_POINT('Ctrl Pts',(0.0326695293498048,0.858459845534159,
-0.301069813346237));
#32874=CARTESIAN_POINT('Ctrl Pts',(-0.375495876558354,0.772672925054673,
-0.290635850743757));
#32875=CARTESIAN_POINT('Ctrl Pts',(-0.695153374314705,0.504759736470026,
-0.280201888141276));
#32876=CARTESIAN_POINT('Ctrl Pts',(-0.850956687463707,0.117869925623525,
-0.269767925538796));
#32877=CARTESIAN_POINT('Ctrl Pts',(-0.806181509144913,-0.296802920130984,
-0.259333962936315));
#32878=CARTESIAN_POINT('Ctrl Pts',(-0.571381772416905,-0.641516556204871,
-0.248900000333835));
#32879=CARTESIAN_POINT('Ctrl Pts',(-0.201901977286727,-0.835018653129937,
-0.238466037731354));
#32880=CARTESIAN_POINT('Ctrl Pts',(0.215168005139201,-0.831699114674314,
-0.228032075128873));
#32881=CARTESIAN_POINT('Ctrl Pts',(0.581520879277012,-0.632340059072374,
-0.217598112526393));
#32882=CARTESIAN_POINT('Ctrl Pts',(0.810803789707567,-0.283932934675704,
-0.207164149923912));
#32883=CARTESIAN_POINT('Ctrl Pts',(0.848972675949112,0.131400691338025,
-0.196730187321432));
#32884=CARTESIAN_POINT('Ctrl Pts',(0.687030621675961,0.515760288909193,
-0.186296224718951));
#32885=CARTESIAN_POINT('Ctrl Pts',(0.363149188196709,0.778553580855519,
-0.17586226211647));
#32886=CARTESIAN_POINT('Ctrl Pts',(-0.0463303092822819,0.85782810261103,
-0.16542829951399));
#32887=CARTESIAN_POINT('Ctrl Pts',(-0.444888556851272,0.734917001280118,
-0.154994336911509));
#32888=CARTESIAN_POINT('Ctrl Pts',(-0.738583893176416,0.438754413204515,
-0.144560374309029));
#32889=CARTESIAN_POINT('Ctrl Pts',(-0.858185002917792,0.0392220405825488,
-0.134126411706548));
#32890=CARTESIAN_POINT('Ctrl Pts',(-0.775511018752148,-0.369654877107235,
-0.123692449104067));
#32891=CARTESIAN_POINT('Ctrl Pts',(-0.598512098358569,-0.583991704355496,
-0.116736474035747));
#32892=CARTESIAN_POINT('Ctrl Pts',(-0.489957628934667,-0.66408276156614,
-0.113258486501587));
#32893=CARTESIAN_POINT('Ctrl Pts',(0.82035433218061,-3.00304598431118E-15,
-1.14076763757253));
#32894=CARTESIAN_POINT('Ctrl Pts',(0.82035433218061,0.134101768298553,-1.13728965003837));
#32895=CARTESIAN_POINT('Ctrl Pts',(0.75336476651959,0.402173049067151,-1.13033367497005));
#32896=CARTESIAN_POINT('Ctrl Pts',(0.475095200548896,0.709610076749492,
-1.11989971236757));
#32897=CARTESIAN_POINT('Ctrl Pts',(0.0849252644561683,0.849729327752103,
-1.10946574976509));
#32898=CARTESIAN_POINT('Ctrl Pts',(-0.325303245075438,0.789587177339035,
-1.09903178716261));
#32899=CARTESIAN_POINT('Ctrl Pts',(-0.658834080958526,0.543317828833921,
-1.08859782456013));
#32900=CARTESIAN_POINT('Ctrl Pts',(-0.83708201976552,0.168990519247407,
-1.07816386195765));
#32901=CARTESIAN_POINT('Ctrl Pts',(-0.818016521001051,-0.24517308681731,
-1.06772989935517));
#32902=CARTESIAN_POINT('Ctrl Pts',(-0.60613955422243,-0.6015452379551,-1.05729593675269));
#32903=CARTESIAN_POINT('Ctrl Pts',(-0.251388414543861,-0.816128465044897,
-1.04686197415021));
#32904=CARTESIAN_POINT('Ctrl Pts',(0.162616634294624,-0.838342060921672,
-1.03642801154773));
#32905=CARTESIAN_POINT('Ctrl Pts',(0.538291771678319,-0.662950796574503,
-1.02599404894524));
#32906=CARTESIAN_POINT('Ctrl Pts',(0.787086296167865,-0.331295673135838,
-1.01556008634276));
#32907=CARTESIAN_POINT('Ctrl Pts',(0.850357274403784,0.0784488915092827,
-1.00512612374028));
#32908=CARTESIAN_POINT('Ctrl Pts',(0.713191002178239,0.469702347171163,
-0.994692161137803));
#32909=CARTESIAN_POINT('Ctrl Pts',(0.407918930452032,0.750242527821311,
-0.984258198535323));
#32910=CARTESIAN_POINT('Ctrl Pts',(0.00649651999368601,0.853943500409919,
-0.973824235932842));
#32911=CARTESIAN_POINT('Ctrl Pts',(-0.396457175080163,0.756361958283295,
-0.963390273330361));
#32912=CARTESIAN_POINT('Ctrl Pts',(-0.705962190288662,0.480498794630969,
-0.952956310727882));
#32913=CARTESIAN_POINT('Ctrl Pts',(-0.849065279296998,0.091377547096046,
-0.942522348125399));
#32914=CARTESIAN_POINT('Ctrl Pts',(-0.792035701226649,-0.319282246717188,
-0.93208838552292));
#32915=CARTESIAN_POINT('Ctrl Pts',(-0.548315862494257,-0.654684213877513,
-0.92165442292044));
#32916=CARTESIAN_POINT('Ctrl Pts',(-0.175352820786369,-0.835770957377394,
-0.911220460317958));
#32917=CARTESIAN_POINT('Ctrl Pts',(0.238942529278509,-0.819858629701545,
-0.900786497715479));
#32918=CARTESIAN_POINT('Ctrl Pts',(0.596916878978052,-0.610697915954459,
-0.890352535112996));
#32919=CARTESIAN_POINT('Ctrl Pts',(0.814192309062806,-0.257589962620873,
-0.879918572510518));
#32920=CARTESIAN_POINT('Ctrl Pts',(0.83955495813993,0.156234366365254,-0.869484609908036));
#32921=CARTESIAN_POINT('Ctrl Pts',(0.667026611423941,0.53323278652594,-0.859050647305556));
#32922=CARTESIAN_POINT('Ctrl Pts',(0.337273822063288,0.784543226294379,
-0.848616684703075));
#32923=CARTESIAN_POINT('Ctrl Pts',(-0.0719775776704071,0.850929452590405,
-0.838182722100595));
#32924=CARTESIAN_POINT('Ctrl Pts',(-0.464263185728891,0.716743607819753,
-0.827748759498114));
#32925=CARTESIAN_POINT('Ctrl Pts',(-0.747117596643004,0.413614556996799,
-0.817314796895633));
#32926=CARTESIAN_POINT('Ctrl Pts',(-0.853869366811587,0.0129926669405188,
-0.806880834293152));
#32927=CARTESIAN_POINT('Ctrl Pts',(-0.759356100494368,-0.390691716850215,
-0.796446871690672));
#32928=CARTESIAN_POINT('Ctrl Pts',(-0.485855463026629,-0.70228639031422,
-0.786012909088191));
#32929=CARTESIAN_POINT('Ctrl Pts',(-0.0978341256794825,-0.848345559796203,
-0.775578946485711));
#32930=CARTESIAN_POINT('Ctrl Pts',(0.313247634771888,-0.794441706032111,
-0.765144983883231));
#32931=CARTESIAN_POINT('Ctrl Pts',(0.650493983049113,-0.55328047407287,
-0.754711021280748));
#32932=CARTESIAN_POINT('Ctrl Pts',(0.834412784606905,-0.181705833307426,
-0.74427705867827));
#32933=CARTESIAN_POINT('Ctrl Pts',(0.821652649004654,0.232698580479195,
-0.733843096075788));
#32934=CARTESIAN_POINT('Ctrl Pts',(0.615221260154403,0.592253751383161,
-0.723409133473309));
#32935=CARTESIAN_POINT('Ctrl Pts',(0.263776436949313,0.812209145653827,
-0.712975170870827));
#32936=CARTESIAN_POINT('Ctrl Pts',(-0.149842972053255,0.84071920918916,
-0.702541208268347));
#32937=CARTESIAN_POINT('Ctrl Pts',(-0.528142983956435,0.671063852007383,
-0.692107245665866));
#32938=CARTESIAN_POINT('Ctrl Pts',(-0.781954729776755,0.343232436627368,
-0.681673283063385));
#32939=CARTESIAN_POINT('Ctrl Pts',(-0.851452395088087,-0.0655020905937811,
-0.671239320460905));
#32940=CARTESIAN_POINT('Ctrl Pts',(-0.720254726869516,-0.458797159315003,
-0.660805357858424));
#32941=CARTESIAN_POINT('Ctrl Pts',(-0.419286248832958,-0.743949424701023,
-0.650371395255944));
#32942=CARTESIAN_POINT('Ctrl Pts',(-0.0194880604808538,-0.85374581725013,
-0.639937432653463));
#32943=CARTESIAN_POINT('Ctrl Pts',(0.384903646922485,-0.762306295106611,
-0.629503470050983));
#32944=CARTESIAN_POINT('Ctrl Pts',(0.698569946491375,-0.491184013209342,
-0.619069507448501));
#32945=CARTESIAN_POINT('Ctrl Pts',(0.847576742823385,-0.10428504206404,
-0.608635544846022));
#32946=CARTESIAN_POINT('Ctrl Pts',(0.796801733297027,0.307194893818648,
-0.59820158224354));
#32947=CARTESIAN_POINT('Ctrl Pts',(0.558213064963931,0.646266105468152,
-0.58776761964106));
#32948=CARTESIAN_POINT('Ctrl Pts',(0.188048329783199,0.83300632088787,-0.577333657038579));
#32949=CARTESIAN_POINT('Ctrl Pts',(-0.226441164460161,0.823399115867465,
-0.566899694436099));
#32950=CARTESIAN_POINT('Ctrl Pts',(-0.587556347598871,0.61970899894198,
-0.556465731833618));
#32951=CARTESIAN_POINT('Ctrl Pts',(-0.810178976333798,0.269947645442809,
-0.546031769231138));
#32952=CARTESIAN_POINT('Ctrl Pts',(-0.841834804326556,-0.143442905707693,
-0.535597806628657));
#32953=CARTESIAN_POINT('Ctrl Pts',(-0.675062255341265,-0.523022615559749,
-0.525163844026176));
#32954=CARTESIAN_POINT('Ctrl Pts',(-0.349171186905277,-0.779320978293641,
-0.514729881423695));
#32955=CARTESIAN_POINT('Ctrl Pts',(0.0590228126390761,-0.851926060501479,
-0.504295918821215));
#32956=CARTESIAN_POINT('Ctrl Pts',(0.453304580405342,-0.723724161788821,
-0.493861956218735));
#32957=CARTESIAN_POINT('Ctrl Pts',(0.740738197317945,-0.424933674833568,
-0.483427993616254));
#32958=CARTESIAN_POINT('Ctrl Pts',(0.853572857874703,-0.0259823261662502,
-0.472994031013773));
#32959=CARTESIAN_POINT('Ctrl Pts',(0.765212371889514,0.379093301023122,
-0.462560068411293));
#32960=CARTESIAN_POINT('Ctrl Pts',(0.496484136534512,0.694813073526274,
-0.452126105808812));
#32961=CARTESIAN_POINT('Ctrl Pts',(0.110729923040362,0.846758873066443,
-0.441692143206332));
#32962=CARTESIAN_POINT('Ctrl Pts',(-0.301124374221852,0.799115646338571,
-0.431258180603851));
#32963=CARTESIAN_POINT('Ctrl Pts',(-0.642000825785283,0.563113349747737,
-0.42082421800137));
#32964=CARTESIAN_POINT('Ctrl Pts',(-0.831551647635552,0.194379943122157,
-0.410390255398891));
#32965=CARTESIAN_POINT('Ctrl Pts',(-0.825097929205883,-0.220170643352121,
-0.399956292796408));
#32966=CARTESIAN_POINT('Ctrl Pts',(-0.624160872597553,-0.582824939487969,
-0.389522330193929));
#32967=CARTESIAN_POINT('Ctrl Pts',(-0.276103230945767,-0.808101918597743,
-0.379088367591447));
#32968=CARTESIAN_POINT('Ctrl Pts',(0.137034537726095,-0.842901678981727,
-0.368654404988968));
#32969=CARTESIAN_POINT('Ctrl Pts',(0.517871977672865,-0.679021590036208,
-0.358220442386487));
#32970=CARTESIAN_POINT('Ctrl Pts',(0.776642124271996,-0.355089729166509,
-0.347786479784006));
#32971=CARTESIAN_POINT('Ctrl Pts',(0.852350421415523,0.0525401187286379,
-0.337352517181526));
#32972=CARTESIAN_POINT('Ctrl Pts',(0.727151711791375,0.447785766997164,
-0.326918554579045));
#32973=CARTESIAN_POINT('Ctrl Pts',(0.430556508150092,0.737484100106964,
-0.316484591976565));
#32974=CARTESIAN_POINT('Ctrl Pts',(0.0324750881634892,0.853350499154803,
-0.306050629374083));
#32975=CARTESIAN_POINT('Ctrl Pts',(-0.373261015454173,0.768074161753151,
-0.295616666771603));
#32976=CARTESIAN_POINT('Ctrl Pts',(-0.691015988779456,0.501755528036834,
-0.285182704169122));
#32977=CARTESIAN_POINT('Ctrl Pts',(-0.8458919979872,0.117168392128866,-0.274748741566642));
#32978=CARTESIAN_POINT('Ctrl Pts',(-0.801383310988866,-0.295036420454529,
-0.264314778964161));
#32979=CARTESIAN_POINT('Ctrl Pts',(-0.567981045319896,-0.637698404316481,
-0.253880816361681));
#32980=CARTESIAN_POINT('Ctrl Pts',(-0.200700305914004,-0.830048822575997,
-0.2434468537592));
#32981=CARTESIAN_POINT('Ctrl Pts',(0.213887378143144,-0.826749042700629,
-0.23301289115672));
#32982=CARTESIAN_POINT('Ctrl Pts',(0.578059804635798,-0.628576521295641,
-0.222578928554239));
#32983=CARTESIAN_POINT('Ctrl Pts',(0.805978085266885,-0.282243037988439,
-0.212144965951758));
#32984=CARTESIAN_POINT('Ctrl Pts',(0.843919785925288,0.130618633522326,
-0.201711003349278));
#32985=CARTESIAN_POINT('Ctrl Pts',(0.682941598426257,0.512690593115557,
-0.191277040746797));
#32986=CARTESIAN_POINT('Ctrl Pts',(0.360987776933422,0.773919846182338,
-0.180843078144316));
#32987=CARTESIAN_POINT('Ctrl Pts',(-0.0460544942459823,0.852722459491376,
-0.170409115541836));
#32988=CARTESIAN_POINT('Ctrl Pts',(-0.442240821284995,0.73054306366155,
-0.159975152939355));
#32989=CARTESIAN_POINT('Ctrl Pts',(-0.734187755498598,0.436142832866621,
-0.149541190336875));
#32990=CARTESIAN_POINT('Ctrl Pts',(-0.853077819122258,0.038989038595815,
-0.139107227734394));
#32991=CARTESIAN_POINT('Ctrl Pts',(-0.770894241208365,-0.367455713931438,
-0.128673265131913));
#32992=CARTESIAN_POINT('Ctrl Pts',(-0.594951669076762,-0.580514449476557,
-0.121717290063593));
#32993=CARTESIAN_POINT('Ctrl Pts',(-0.48704143763805,-0.660130190455607,
-0.118239302529433));
#32994=CARTESIAN_POINT('Ctrl Pts',(0.816972063808647,-2.99066461804804E-15,
-1.1425283350431));
#32995=CARTESIAN_POINT('Ctrl Pts',(0.816972063808648,0.133547259366551,
-1.13905034750894));
#32996=CARTESIAN_POINT('Ctrl Pts',(0.750258545288663,0.400515882139597,
-1.13209437244062));
#32997=CARTESIAN_POINT('Ctrl Pts',(0.473136385937636,0.70668384175515,-1.12166040983814));
#32998=CARTESIAN_POINT('Ctrl Pts',(0.0845750992767496,0.846226087845691,
-1.11122644723566));
#32999=CARTESIAN_POINT('Ctrl Pts',(-0.323961995775536,0.786331547179378,
-1.10079248463318));
#33000=CARTESIAN_POINT('Ctrl Pts',(-0.656117677249231,0.541077762637851,
-1.0903585220307));
#33001=CARTESIAN_POINT('Ctrl Pts',(-0.833630685095572,0.168293731192072,
-1.07992455942822));
#33002=CARTESIAN_POINT('Ctrl Pts',(-0.814643797129343,-0.244162209445383,
-1.06949059682573));
#33003=CARTESIAN_POINT('Ctrl Pts',(-0.603640408739919,-0.59906504366349,
-1.05905663422325));
#33004=CARTESIAN_POINT('Ctrl Pts',(-0.250351927233723,-0.812763520669616,
-1.04862267162077));
#33005=CARTESIAN_POINT('Ctrl Pts',(0.161946157548482,-0.83488553496122,
-1.03818870901829));
#33006=CARTESIAN_POINT('Ctrl Pts',(0.536072366553592,-0.660217414778481,
-1.02775474641581));
#33007=CARTESIAN_POINT('Ctrl Pts',(0.783841098330601,-0.329929724332764,
-1.01732078381333));
#33008=CARTESIAN_POINT('Ctrl Pts',(0.846851206973997,0.0781254429130721,
-1.00688682121085));
#33009=CARTESIAN_POINT('Ctrl Pts',(0.710250478470445,0.467765739743977,
-0.99645285860837));
#33010=CARTESIAN_POINT('Ctrl Pts',(0.406237059412559,0.747149238803469,
-0.98601889600589));
#33011=CARTESIAN_POINT('Ctrl Pts',(0.00646973450489124,0.850422646762807,
-0.975584933403409));
#33012=CARTESIAN_POINT('Ctrl Pts',(-0.394822561461415,0.753243438481206,
-0.965150970800928));
#33013=CARTESIAN_POINT('Ctrl Pts',(-0.70305147134073,0.478517673019022,
-0.954717008198448));
#33014=CARTESIAN_POINT('Ctrl Pts',(-0.845564538846855,0.0910007927061355,
-0.944283045595966));
#33015=CARTESIAN_POINT('Ctrl Pts',(-0.788770096702248,-0.317965829356403,
-0.933849082993488));
#33016=CARTESIAN_POINT('Ctrl Pts',(-0.546055127582366,-0.651984916701293,
-0.923415120391005));
#33017=CARTESIAN_POINT('Ctrl Pts',(-0.174629831956392,-0.832325030110572,
-0.912981157788527));
#33018=CARTESIAN_POINT('Ctrl Pts',(0.237957356762351,-0.816478309791072,
-0.902547195186044));
#33019=CARTESIAN_POINT('Ctrl Pts',(0.594455759539154,-0.608179976581174,
-0.892113232583563));
#33020=CARTESIAN_POINT('Ctrl Pts',(0.810835351688311,-0.256527905763963,
-0.881679269981084));
#33021=CARTESIAN_POINT('Ctrl Pts',(0.836093429239885,0.155590203920442,
-0.871245307378603));
#33022=CARTESIAN_POINT('Ctrl Pts',(0.664276425899861,0.531034239923244,
-0.860811344776122));
#33023=CARTESIAN_POINT('Ctrl Pts',(0.335883224496111,0.78130851363521,-0.850377382173643));
#33024=CARTESIAN_POINT('Ctrl Pts',(-0.0716808103619117,0.847421026056225,
-0.83994341957116));
#33025=CARTESIAN_POINT('Ctrl Pts',(-0.462349004389065,0.71378843652532,
-0.829509456968681));
#33026=CARTESIAN_POINT('Ctrl Pts',(-0.744037191807753,0.411909202596062,
-0.819075494366199));
#33027=CARTESIAN_POINT('Ctrl Pts',(-0.850348818857665,0.0129390974967706,
-0.808641531763719));
#33028=CARTESIAN_POINT('Ctrl Pts',(-0.756225235669137,-0.389080874515506,
-0.798207569161239));
#33029=CARTESIAN_POINT('Ctrl Pts',(-0.483852255600829,-0.699390826881936,
-0.787773606558758));
#33030=CARTESIAN_POINT('Ctrl Pts',(-0.0974307504743614,-0.844847786786836,
-0.777339643956278));
#33031=CARTESIAN_POINT('Ctrl Pts',(0.31195609842859,-0.791166181424495,
-0.766905681353797));
#33032=CARTESIAN_POINT('Ctrl Pts',(0.647811962414489,-0.550999269808316,
-0.756471718751317));
#33033=CARTESIAN_POINT('Ctrl Pts',(0.830972457156651,-0.180956650675363,
-0.746037756148836));
#33034=CARTESIAN_POINT('Ctrl Pts',(0.818264932259306,0.231739152089763,
-0.735603793546355));
#33035=CARTESIAN_POINT('Ctrl Pts',(0.61268467079679,0.589811858262647,-0.725169830943875));
#33036=CARTESIAN_POINT('Ctrl Pts',(0.262688872936024,0.808860364965553,
-0.714735868341393));
#33037=CARTESIAN_POINT('Ctrl Pts',(-0.149225161660734,0.837252880021286,
-0.704301905738914));
#33038=CARTESIAN_POINT('Ctrl Pts',(-0.525965422875296,0.668297020729717,
-0.693867943136432));
#33039=CARTESIAN_POINT('Ctrl Pts',(-0.778730689623806,0.341817271381425,
-0.683433980533953));
#33040=CARTESIAN_POINT('Ctrl Pts',(-0.847941812434698,-0.0652320220563909,
-0.673000017931471));
#33041=CARTESIAN_POINT('Ctrl Pts',(-0.717285079048034,-0.456905514687298,
-0.662566055328991));
#33042=CARTESIAN_POINT('Ctrl Pts',(-0.417557509750833,-0.740882082404002,
-0.652132092726511));
#33043=CARTESIAN_POINT('Ctrl Pts',(-0.0194077101906125,-0.850225778697497,
-0.64169813012403));
#33044=CARTESIAN_POINT('Ctrl Pts',(0.383316669102108,-0.759163266475053,
-0.631264167521549));
#33045=CARTESIAN_POINT('Ctrl Pts',(0.695689706150894,-0.489158835893097,
-0.620830204919068));
#33046=CARTESIAN_POINT('Ctrl Pts',(0.844082139686513,-0.103855069394059,
-0.610396242316588));
#33047=CARTESIAN_POINT('Ctrl Pts',(0.793516478173853,0.305928313242129,
-0.599962279714107));
#33048=CARTESIAN_POINT('Ctrl Pts',(0.555911523369753,0.643601516593404,
-0.589528317111627));
#33049=CARTESIAN_POINT('Ctrl Pts',(0.187272996707217,0.829571792360918,
-0.579094354509145));
#33050=CARTESIAN_POINT('Ctrl Pts',(-0.225507535723485,0.820004198348112,
-0.568660391906667));
#33051=CARTESIAN_POINT('Ctrl Pts',(-0.585133822119268,0.617153906403178,
-0.558226429304184));
#33052=CARTESIAN_POINT('Ctrl Pts',(-0.806838566139564,0.26883463721489,
-0.547792466701705));
#33053=CARTESIAN_POINT('Ctrl Pts',(-0.838363875501719,-0.142851483122668,
-0.537358504099224));
#33054=CARTESIAN_POINT('Ctrl Pts',(-0.672278938438019,-0.520866166024689,
-0.526924541496743));
#33055=CARTESIAN_POINT('Ctrl Pts',(-0.347731535882056,-0.776107797235484,
-0.516490578894263));
#33056=CARTESIAN_POINT('Ctrl Pts',(0.0587794585027788,-0.848413524900876,
-0.506056616291782));
#33057=CARTESIAN_POINT('Ctrl Pts',(0.451435581967082,-0.720740209306132,
-0.495622653689302));
#33058=CARTESIAN_POINT('Ctrl Pts',(0.737684095078984,-0.423181651119364,
-0.485188691086821));
#33059=CARTESIAN_POINT('Ctrl Pts',(0.8500535324426,-0.0258751996797192,
-0.474754728484341));
#33060=CARTESIAN_POINT('Ctrl Pts',(0.762057361351743,0.377530279562069,
-0.46432076588186));
#33061=CARTESIAN_POINT('Ctrl Pts',(0.494437106533239,0.691948322969061,
-0.453886803279379));
#33062=CARTESIAN_POINT('Ctrl Pts',(0.110273377789823,0.843267642049257,
-0.443452840676899));
#33063=CARTESIAN_POINT('Ctrl Pts',(-0.299882822714386,0.795820850831186,
-0.433018878074418));
#33064=CARTESIAN_POINT('Ctrl Pts',(-0.639353822881232,0.560791604023703,
-0.422584915471937));
#33065=CARTESIAN_POINT('Ctrl Pts',(-0.828123116802314,0.193578504473992,
-0.412150952869457));
#33066=CARTESIAN_POINT('Ctrl Pts',(-0.821696007390509,-0.219262868301153,
-0.401716990266975));
#33067=CARTESIAN_POINT('Ctrl Pts',(-0.621587424751339,-0.580421921850917,
-0.391283027664496));
#33068=CARTESIAN_POINT('Ctrl Pts',(-0.274964842917688,-0.804770072220882,
-0.380849065062014));
#33069=CARTESIAN_POINT('Ctrl Pts',(0.13646953717677,-0.839426351377121,
-0.370415102459534));
#33070=CARTESIAN_POINT('Ctrl Pts',(0.515736764486322,-0.676221948589213,
-0.359981139857054));
#33071=CARTESIAN_POINT('Ctrl Pts',(0.773439988269239,-0.353625675685122,
-0.349547177254573));
#33072=CARTESIAN_POINT('Ctrl Pts',(0.848836136151768,0.052323493078395,
-0.339113214652093));
#33073=CARTESIAN_POINT('Ctrl Pts',(0.724153627343063,0.445939522912988,
-0.328679252049611));
#33074=CARTESIAN_POINT('Ctrl Pts',(0.428781301197021,0.734443414683683,
-0.318245289447132));
#33075=CARTESIAN_POINT('Ctrl Pts',(0.0323411916877329,0.849832090513251,
-0.30781132684465));
#33076=CARTESIAN_POINT('Ctrl Pts',(-0.37172204082515,0.764907351918341,
-0.297377364242171));
#33077=CARTESIAN_POINT('Ctrl Pts',(-0.688166893772679,0.499686763789961,
-0.286943401639689));
#33078=CARTESIAN_POINT('Ctrl Pts',(-0.842404341196427,0.116685300780257,
-0.276509439037209));
#33079=CARTESIAN_POINT('Ctrl Pts',(-0.798079165673276,-0.293819969988382,
-0.266075476434728));
#33080=CARTESIAN_POINT('Ctrl Pts',(-0.56563923004628,-0.635069140343264,
-0.255641513832248));
#33081=CARTESIAN_POINT('Ctrl Pts',(-0.199872807661205,-0.826626488317452,
-0.245207551229767));
#33082=CARTESIAN_POINT('Ctrl Pts',(0.213005508499054,-0.823340312573245,
-0.234773588627286));
#33083=CARTESIAN_POINT('Ctrl Pts',(0.575676435516449,-0.625984868845308,
-0.224339626024806));
#33084=CARTESIAN_POINT('Ctrl Pts',(0.802654992386147,-0.281079332570895,
-0.213905663422325));
#33085=CARTESIAN_POINT('Ctrl Pts',(0.840440266860438,0.130080080884023,
-0.203471700819845));
#33086=CARTESIAN_POINT('Ctrl Pts',(0.680125782303056,0.510576753259704,
-0.193037738217364));
#33087=CARTESIAN_POINT('Ctrl Pts',(0.359499429618306,0.770728914207567,
-0.182603775614884));
#33088=CARTESIAN_POINT('Ctrl Pts',(-0.0458646565737043,0.849206679729667,
-0.172169813012403));
#33089=CARTESIAN_POINT('Ctrl Pts',(-0.440417346097005,0.727530918967195,
-0.161735850409922));
#33090=CARTESIAN_POINT('Ctrl Pts',(-0.731160844709421,0.434344745947389,
-0.151301887807442));
#33091=CARTESIAN_POINT('Ctrl Pts',(-0.849560168473914,0.0388279800983712,
-0.140867925204961));
#33092=CARTESIAN_POINT('Ctrl Pts',(-0.767716584589541,-0.365940025647496,
-0.13043396260248));
#33093=CARTESIAN_POINT('Ctrl Pts',(-0.59249742112771,-0.578121984952217,
-0.12347798753416));
#33094=CARTESIAN_POINT('Ctrl Pts',(-0.485033396983252,-0.657408515958416,
-0.12));
#33095=CARTESIAN_POINT('',(-0.814921455736581,-0.139942643537172,-0.12));
#33096=CARTESIAN_POINT('',(-0.485033396983251,-0.657408515958417,-0.12));
#33097=CARTESIAN_POINT('Ctrl Pts',(-0.81492145573658,-0.139942643537173,
-0.12));
#33098=CARTESIAN_POINT('Ctrl Pts',(-0.797805299826961,-0.239614354303276,
-0.12));
#33099=CARTESIAN_POINT('Ctrl Pts',(-0.761989157288878,-0.335286098400442,
-0.12));
#33100=CARTESIAN_POINT('Ctrl Pts',(-0.676216606680943,-0.475719941382464,
-0.12));
#33101=CARTESIAN_POINT('Ctrl Pts',(-0.636663795100042,-0.525852834710436,
-0.12));
#33102=CARTESIAN_POINT('Ctrl Pts',(-0.553238444854268,-0.608184477072056,
-0.12));
#33103=CARTESIAN_POINT('Ctrl Pts',(-0.516370109403214,-0.63662333474392,
-0.12));
#33104=CARTESIAN_POINT('Ctrl Pts',(-0.485033396983252,-0.657408515958416,
-0.12));
#33105=CARTESIAN_POINT('',(0.826819918308061,8.40321746433153E-9,-1.12624999033503));
#33106=CARTESIAN_POINT('Ctrl Pts',(0.82685,-3.02682447659827E-15,-1.12625));
#33107=CARTESIAN_POINT('Ctrl Pts',(0.82685,0.135161967341268,-1.12277201246584));
#33108=CARTESIAN_POINT('Ctrl Pts',(0.793089927145679,0.270260225604108,
-1.11929402493168));
#33109=CARTESIAN_POINT('Ctrl Pts',(0.729464420950725,0.389454322909825,
-1.11581603739752));
#33110=CARTESIAN_POINT('Ctrl Pts',(0.66583891475577,0.508648420215542,-1.11233804986336));
#33111=CARTESIAN_POINT('Ctrl Pts',(0.572347975220182,0.611938356564135,
-1.1088600623292));
#33112=CARTESIAN_POINT('Ctrl Pts',(0.460059281045226,0.687121564557402,
-1.10538207479504));
#33113=CARTESIAN_POINT('Ctrl Pts',(0.34777058687027,0.762304772550668,-1.10190408726088));
#33114=CARTESIAN_POINT('Ctrl Pts',(0.216684138055947,0.809381252188609,
-1.09842609972672));
#33115=CARTESIAN_POINT('Ctrl Pts',(0.0822281335574654,0.822816371973694,
-1.09494811219256));
#33116=CARTESIAN_POINT('Ctrl Pts',(-0.0522278709410159,0.836251491758778,
-1.0914701246584));
#33117=CARTESIAN_POINT('Ctrl Pts',(-0.190053431123656,0.816045251691006,
-1.08799213712424));
#33118=CARTESIAN_POINT('Ctrl Pts',(-0.31499483556927,0.764572277302742,
-1.08451414959008));
#33119=CARTESIAN_POINT('Ctrl Pts',(-0.439936240014884,0.713099302914477,
-1.08103616205592));
#33120=CARTESIAN_POINT('Ctrl Pts',(-0.551993488723474,0.630359594205718,
-1.07755817452176));
#33121=CARTESIAN_POINT('Ctrl Pts',(-0.637965330037046,0.526107851543765,
-1.0740801869876));
#33122=CARTESIAN_POINT('Ctrl Pts',(-0.723937171350618,0.421856108881812,
-1.07060219945344));
#33123=CARTESIAN_POINT('Ctrl Pts',(-0.783823605269174,0.296092332266663,
-1.06712421191928));
#33124=CARTESIAN_POINT('Ctrl Pts',(-0.810564079439898,0.1636366258683,-1.06364622438512));
#33125=CARTESIAN_POINT('Ctrl Pts',(-0.837304553610622,0.0311809194699361,
-1.06016823685096));
#33126=CARTESIAN_POINT('Ctrl Pts',(-0.830899068033515,-0.107966716711643,
-1.0566902493168));
#33127=CARTESIAN_POINT('Ctrl Pts',(-0.792103889995617,-0.237406190245859,
-1.05321226178264));
#33128=CARTESIAN_POINT('Ctrl Pts',(-0.75330871195772,-0.366845663780076,
-1.04973427424848));
#33129=CARTESIAN_POINT('Ctrl Pts',(-0.682123841459031,-0.48657697466693,
-1.04625628671432));
#33130=CARTESIAN_POINT('Ctrl Pts',(-0.5869380627173,-0.582489677808408,
-1.04277829918015));
#33131=CARTESIAN_POINT('Ctrl Pts',(-0.491752283975569,-0.678402380949886,
-1.03930031164599));
#33132=CARTESIAN_POINT('Ctrl Pts',(-0.372565596990794,-0.750496476345988,
-1.03582232411183));
#33133=CARTESIAN_POINT('Ctrl Pts',(-0.243425062820331,-0.790275105642179,
-1.03234433657767));
#33134=CARTESIAN_POINT('Ctrl Pts',(-0.114284528649868,-0.83005373493837,
-1.02886634904351));
#33135=CARTESIAN_POINT('Ctrl Pts',(0.0248098527062832,-0.837516898134649,
-1.02538836150935));
#33136=CARTESIAN_POINT('Ctrl Pts',(0.157465332643303,-0.811785143597848,
-1.02191037397519));
#33137=CARTESIAN_POINT('Ctrl Pts',(0.290120812580322,-0.786053389061048,
-1.01843238644103));
#33138=CARTESIAN_POINT('Ctrl Pts',(0.416337391098209,-0.727126716791168,
-1.01495439890687));
#33139=CARTESIAN_POINT('Ctrl Pts',(0.52123976058448,-0.641949852425352,
-1.01147641137271));
#33140=CARTESIAN_POINT('Ctrl Pts',(0.626142130070751,-0.556772988059536,
-1.00799842383855));
#33141=CARTESIAN_POINT('Ctrl Pts',(0.709730290525405,-0.445345931597784,
-1.00452043630439));
#33142=CARTESIAN_POINT('Ctrl Pts',(0.762153030458448,-0.320800915734334,
-1.00104244877023));
#33143=CARTESIAN_POINT('Ctrl Pts',(0.814575770391491,-0.196255899870884,
-0.997564461236072));
#33144=CARTESIAN_POINT('Ctrl Pts',(0.835833089802923,-0.0585929246057353,
-0.994086473701912));
#33145=CARTESIAN_POINT('Ctrl Pts',(0.823419690225198,0.0759637968315887,
-0.990608486167752));
#33146=CARTESIAN_POINT('Ctrl Pts',(0.811006290647473,0.210520518268912,
-0.987130498633591));
#33147=CARTESIAN_POINT('Ctrl Pts',(0.764922172080592,0.34197098587841,-0.983652511099432));
#33148=CARTESIAN_POINT('Ctrl Pts',(0.690598576442014,0.454823136345075,
-0.980174523565272));
#33149=CARTESIAN_POINT('Ctrl Pts',(0.616274980803435,0.567675286811741,
-0.976696536031112));
#33150=CARTESIAN_POINT('Ctrl Pts',(0.513711908093158,0.661929120135573,
-0.973218548496951));
#33151=CARTESIAN_POINT('Ctrl Pts',(0.394996892421945,0.726476383047986,
-0.969740560962791));
#33152=CARTESIAN_POINT('Ctrl Pts',(0.276281876750733,0.791023645960399,
-0.96626257342863));
#33153=CARTESIAN_POINT('Ctrl Pts',(0.141414918118584,0.825864338461393,
-0.962784585894471));
#33154=CARTESIAN_POINT('Ctrl Pts',(0.00629072459520486,0.826892319144936,
-0.95930659836031));
#33155=CARTESIAN_POINT('Ctrl Pts',(-0.128833468928174,0.827920299828479,
-0.95582861082615));
#33156=CARTESIAN_POINT('Ctrl Pts',(-0.264214897342785,0.79513556869457,
-0.952350623291989));
#33157=CARTESIAN_POINT('Ctrl Pts',(-0.383898224562581,0.732401961438677,
-0.948872635757829));
#33158=CARTESIAN_POINT('Ctrl Pts',(-0.503581551782376,0.669668354182784,
-0.945394648223669));
#33159=CARTESIAN_POINT('Ctrl Pts',(-0.607566777807355,0.576985870804906,
-0.941916660689509));
#33160=CARTESIAN_POINT('Ctrl Pts',(-0.683598754197441,0.465277577070771,
-0.938438673155349));
#33161=CARTESIAN_POINT('Ctrl Pts',(-0.759630730587527,0.353569283336635,
-0.934960685621189));
#33162=CARTESIAN_POINT('Ctrl Pts',(-0.807709457342717,0.222835179246241,
-0.931482698087028));
#33163=CARTESIAN_POINT('Ctrl Pts',(-0.822168630942393,0.0884828937125682,
-0.928004710552868));
#33164=CARTESIAN_POINT('Ctrl Pts',(-0.83662780454207,-0.0458693918211047,
-0.924526723018708));
#33165=CARTESIAN_POINT('Ctrl Pts',(-0.817467424986232,-0.183839858798057,
-0.921048735484548));
#33166=CARTESIAN_POINT('Ctrl Pts',(-0.766945632855927,-0.309168039331662,
-0.917570747950388));
#33167=CARTESIAN_POINT('Ctrl Pts',(-0.716423840725621,-0.434496219865267,
-0.914092760416228));
#33168=CARTESIAN_POINT('Ctrl Pts',(-0.634540636020849,-0.547182113955525,
-0.910614772882067));
#33169=CARTESIAN_POINT('Ctrl Pts',(-0.530946339389745,-0.633945159267193,
-0.907136785347907));
#33170=CARTESIAN_POINT('Ctrl Pts',(-0.42735204275864,-0.720708204578862,
-0.903658797813747));
#33171=CARTESIAN_POINT('Ctrl Pts',(-0.302046654201204,-0.781548401111942,
-0.900180810279587));
#33172=CARTESIAN_POINT('Ctrl Pts',(-0.169798002666679,-0.809295445778767,
-0.896702822745426));
#33173=CARTESIAN_POINT('Ctrl Pts',(-0.0375493511321535,-0.837042490445593,
-0.893224835211266));
#33174=CARTESIAN_POINT('Ctrl Pts',(0.101642563379461,-0.831696383246165,
-0.889746847677106));
#33175=CARTESIAN_POINT('Ctrl Pts',(0.231373319484613,-0.793887188023754,
-0.886268860142946));
#33176=CARTESIAN_POINT('Ctrl Pts',(0.361104075589764,-0.756077992801343,
-0.882790872608786));
#33177=CARTESIAN_POINT('Ctrl Pts',(0.481373673288452,-0.68580570955595,
-0.879312885074626));
#33178=CARTESIAN_POINT('Ctrl Pts',(0.578007775213605,-0.59135225717159,
-0.875834897540465));
#33179=CARTESIAN_POINT('Ctrl Pts',(0.67464187713876,-0.49689880478723,-0.872356910006305));
#33180=CARTESIAN_POINT('Ctrl Pts',(0.74764048329038,-0.378264183263903,
-0.868878922472145));
#33181=CARTESIAN_POINT('Ctrl Pts',(0.788400364817746,-0.249430040350934,
-0.865400934937985));
#33182=CARTESIAN_POINT('Ctrl Pts',(0.829160246345112,-0.120595897437964,
-0.861922947403825));
#33183=CARTESIAN_POINT('Ctrl Pts',(0.837681403248224,0.0184377668646483,
-0.858444959869665));
#33184=CARTESIAN_POINT('Ctrl Pts',(0.812959577138439,0.151285181729251,
-0.854966972335504));
#33185=CARTESIAN_POINT('Ctrl Pts',(0.788237751028653,0.284132596593853,
-0.851488984801344));
#33186=CARTESIAN_POINT('Ctrl Pts',(0.73027294190597,0.410793762020446,-0.848010997267183));
#33187=CARTESIAN_POINT('Ctrl Pts',(0.645896574970356,0.516341064330821,
-0.844533009733023));
#33188=CARTESIAN_POINT('Ctrl Pts',(0.561520208034741,0.621888366641197,
-0.841055022198863));
#33189=CARTESIAN_POINT('Ctrl Pts',(0.450732283286195,0.706321805835355,
-0.837577034664703));
#33190=CARTESIAN_POINT('Ctrl Pts',(0.326589678383616,0.759690504248876,
-0.834099047130543));
#33191=CARTESIAN_POINT('Ctrl Pts',(0.202447073481038,0.813059202662397,
-0.830621059596383));
#33192=CARTESIAN_POINT('Ctrl Pts',(0.0649497884244267,0.835363160295282,
-0.827143072062222));
#33193=CARTESIAN_POINT('Ctrl Pts',(-0.0696974754768556,0.823973750907556,
-0.823665084528062));
#33194=CARTESIAN_POINT('Ctrl Pts',(-0.204344739378138,0.81258434151983,
-0.820187096993902));
#33195=CARTESIAN_POINT('Ctrl Pts',(-0.336141982124091,0.767501565111493,
-0.816709109459742));
#33196=CARTESIAN_POINT('Ctrl Pts',(-0.449556279182337,0.694038638780559,
-0.813231121925582));
#33197=CARTESIAN_POINT('Ctrl Pts',(-0.562970576240583,0.620575712449625,
-0.809753134391421));
#33198=CARTESIAN_POINT('Ctrl Pts',(-0.658001927611122,0.518732636196093,
-0.806275146857261));
#33199=CARTESIAN_POINT('Ctrl Pts',(-0.723450441867888,0.400512095240222,
-0.802797159323101));
#33200=CARTESIAN_POINT('Ctrl Pts',(-0.788898956124655,0.282291554284351,
-0.799319171788941));
#33201=CARTESIAN_POINT('Ctrl Pts',(-0.824764633267649,0.147693548626141,
-0.795841184254781));
#33202=CARTESIAN_POINT('Ctrl Pts',(-0.826820534669346,0.012581085871065,
-0.79236319672062));
#33203=CARTESIAN_POINT('Ctrl Pts',(-0.828876436071042,-0.122531376884011,
-0.78888520918646));
#33204=CARTESIAN_POINT('Ctrl Pts',(-0.79712256173144,-0.258158296735951,
-0.7854072216523));
#33205=CARTESIAN_POINT('Ctrl Pts',(-0.735301254991326,-0.378315403705378,
-0.78192923411814));
#33206=CARTESIAN_POINT('Ctrl Pts',(-0.673479948251211,-0.498472510674805,
-0.77845124658398));
#33207=CARTESIAN_POINT('Ctrl Pts',(-0.581591209110582,-0.603159804761718,
-0.77497325904982));
#33208=CARTESIAN_POINT('Ctrl Pts',(-0.470464557373384,-0.68003939630587,
-0.771495271515659));
#33209=CARTESIAN_POINT('Ctrl Pts',(-0.359337905636187,-0.756918987850021,
-0.768017283981499));
#33210=CARTESIAN_POINT('Ctrl Pts',(-0.228973341302421,-0.805990876851411,
-0.764539296447338));
#33211=CARTESIAN_POINT('Ctrl Pts',(-0.0947349410194661,-0.821471710543111,
-0.761061308913178));
#33212=CARTESIAN_POINT('Ctrl Pts',(0.0395034592634902,-0.83695254423481,
-0.757583321379018));
#33213=CARTESIAN_POINT('Ctrl Pts',(0.177615695495635,-0.818842322616818,
-0.754105333844858));
#33214=CARTESIAN_POINT('Ctrl Pts',(0.3033245914807,-0.769275420428634,-0.750627346310698));
#33215=CARTESIAN_POINT('Ctrl Pts',(0.429033487465763,-0.719708518240451,
-0.747149358776538));
#33216=CARTESIAN_POINT('Ctrl Pts',(0.542339043203749,-0.638684935482076,
-0.743671371242377));
#33217=CARTESIAN_POINT('Ctrl Pts',(0.62988766639119,-0.535753682209321,
-0.740193383708217));
#33218=CARTESIAN_POINT('Ctrl Pts',(0.717436289578632,-0.432822428936566,
-0.736715396174057));
#33219=CARTESIAN_POINT('Ctrl Pts',(0.779227980215528,-0.307983505149432,
-0.733237408639897));
#33220=CARTESIAN_POINT('Ctrl Pts',(0.807980297126493,-0.175949764785204,
-0.729759421105737));
#33221=CARTESIAN_POINT('Ctrl Pts',(0.836732614037458,-0.0439160244209771,
-0.726281433571577));
#33222=CARTESIAN_POINT('Ctrl Pts',(0.83244555722249,0.0953125325203408,
-0.722803446037417));
#33223=CARTESIAN_POINT('Ctrl Pts',(0.795624376477292,0.225327166199963,
-0.719325458503256));
#33224=CARTESIAN_POINT('Ctrl Pts',(0.758803195732095,0.355341799879584,
-0.715847470969096));
#33225=CARTESIAN_POINT('Ctrl Pts',(0.689447891056669,0.476142510297508,
-0.712369483434936));
#33226=CARTESIAN_POINT('Ctrl Pts',(0.59573231109141,0.573492365942453,-0.708891495900776));
#33227=CARTESIAN_POINT('Ctrl Pts',(0.502016731126151,0.670842221587399,
-0.705413508366616));
#33228=CARTESIAN_POINT('Ctrl Pts',(0.383940875871057,0.744741222459364,
-0.701935520832455));
#33229=CARTESIAN_POINT('Ctrl Pts',(0.255420539849086,0.786480023964873,
-0.698457533298295));
#33230=CARTESIAN_POINT('Ctrl Pts',(0.126900203827114,0.828218825470382,
-0.694979545764135));
#33231=CARTESIAN_POINT('Ctrl Pts',(-0.0120646129617348,0.837797427609435,
-0.691501558229975));
#33232=CARTESIAN_POINT('Ctrl Pts',(-0.145096253695276,0.814086947098516,
-0.688023570695815));
#33233=CARTESIAN_POINT('Ctrl Pts',(-0.278127894428818,0.790376466587597,
-0.684545583161654));
#33234=CARTESIAN_POINT('Ctrl Pts',(-0.405226359107052,0.733376903426706,
-0.681067595627494));
#33235=CARTESIAN_POINT('Ctrl Pts',(-0.511412496278359,0.649805924044189,
-0.677589608093334));
#33236=CARTESIAN_POINT('Ctrl Pts',(-0.617598633449666,0.566234944661672,
-0.674111620559174));
#33237=CARTESIAN_POINT('Ctrl Pts',(-0.702872443114046,0.456092549057529,
-0.670633633025014));
#33238=CARTESIAN_POINT('Ctrl Pts',(-0.757184005997863,0.332359536245936,
-0.667155645490853));
#33239=CARTESIAN_POINT('Ctrl Pts',(-0.81149556888168,0.208626523434343,
-0.663677657956693));
#33240=CARTESIAN_POINT('Ctrl Pts',(-0.834844884984934,0.0713028934153015,
-0.660199670422533));
#33241=CARTESIAN_POINT('Ctrl Pts',(-0.824480127658202,-0.0634271185637466,
-0.656721682888372));
#33242=CARTESIAN_POINT('Ctrl Pts',(-0.814115370331471,-0.198157130542796,
-0.653243695354212));
#33243=CARTESIAN_POINT('Ctrl Pts',(-0.770036539574754,-0.330293524481848,
-0.649765707820052));
#33244=CARTESIAN_POINT('Ctrl Pts',(-0.697438532772425,-0.444263405286585,
-0.646287720285892));
#33245=CARTESIAN_POINT('Ctrl Pts',(-0.624840525970098,-0.55823328609132,
-0.642809732751732));
#33246=CARTESIAN_POINT('Ctrl Pts',(-0.523723343122158,-0.654036653761739,
-0.639331745217572));
#33247=CARTESIAN_POINT('Ctrl Pts',(-0.406004119499086,-0.720382631122071,
-0.635853757683412));
#33248=CARTESIAN_POINT('Ctrl Pts',(-0.288284895876013,-0.786728608482403,
-0.632375770149252));
#33249=CARTESIAN_POINT('Ctrl Pts',(-0.153963631477806,-0.823617195532651,
-0.628897782615091));
#33250=CARTESIAN_POINT('Ctrl Pts',(-0.0188707186517489,-0.82670089890489,
-0.625419795080931));
#33251=CARTESIAN_POINT('Ctrl Pts',(0.116222194174309,-0.829784602277128,
-0.621941807546771));
#33252=CARTESIAN_POINT('Ctrl Pts',(0.252086755428217,-0.799063421971358,
-0.61846382001261));
#33253=CARTESIAN_POINT('Ctrl Pts',(0.372710687974431,-0.738157993482569,
-0.61498583247845));
#33254=CARTESIAN_POINT('Ctrl Pts',(0.493334620520646,-0.677252564993779,
-0.61150784494429));
#33255=CARTESIAN_POINT('Ctrl Pts',(0.598717924359166,-0.58616288832197,
-0.60802985741013));
#33256=CARTESIAN_POINT('Ctrl Pts',(0.676440681809118,-0.47562431000339,
-0.604551869875969));
#33257=CARTESIAN_POINT('Ctrl Pts',(0.754163439259069,-0.365085731684811,
-0.601073882341809));
#33258=CARTESIAN_POINT('Ctrl Pts',(0.804225650320452,-0.235098251719462,
-0.597595894807649));
#33259=CARTESIAN_POINT('Ctrl Pts',(0.820727248116851,-0.100981505589522,
-0.594117907273489));
#33260=CARTESIAN_POINT('Ctrl Pts',(0.837228845913249,0.0331352405404172,
-0.590639919739329));
#33261=CARTESIAN_POINT('Ctrl Pts',(0.820169830444663,0.171381252834947,
-0.587161932205169));
#33262=CARTESIAN_POINT('Ctrl Pts',(0.771560686864994,0.297463588960067,
-0.583683944671009));
#33263=CARTESIAN_POINT('Ctrl Pts',(0.722951543285326,0.423545925085188,
-0.580205957136848));
#33264=CARTESIAN_POINT('Ctrl Pts',(0.642792271594576,0.5374645850409,-0.576727969602688));
#33265=CARTESIAN_POINT('Ctrl Pts',(0.540530018726793,0.625793719309964,
-0.573249982068528));
#33266=CARTESIAN_POINT('Ctrl Pts',(0.43826776585901,0.714122853579028,-0.569771994534367));
#33267=CARTESIAN_POINT('Ctrl Pts',(0.313902531814194,0.776862462161444,
-0.566294007000207));
#33268=CARTESIAN_POINT('Ctrl Pts',(0.182091343967062,0.80661838729653,-0.562816019466047));
#33269=CARTESIAN_POINT('Ctrl Pts',(0.0502801561199304,0.836374312431615,
-0.559338031931886));
#33270=CARTESIAN_POINT('Ctrl Pts',(-0.0889769855295178,0.833146554119371,
-0.555860044397727));
#33271=CARTESIAN_POINT('Ctrl Pts',(-0.219267972300287,0.797315518848032,
-0.552382056863567));
#33272=CARTESIAN_POINT('Ctrl Pts',(-0.349558959071054,0.761484483576693,
-0.548904069329407));
#33273=CARTESIAN_POINT('Ctrl Pts',(-0.470883790963143,0.69305017134626,
-0.545426081795246));
#33274=CARTESIAN_POINT('Ctrl Pts',(-0.56894376628606,0.600077887508629,
-0.541948094261086));
#33275=CARTESIAN_POINT('Ctrl Pts',(-0.667003741608978,0.507105603670996,
-0.538470106726926));
#33276=CARTESIAN_POINT('Ctrl Pts',(-0.741798860362724,0.389595348226163,
-0.534992119192766));
#33277=CARTESIAN_POINT('Ctrl Pts',(-0.784514166249512,0.261396257101012,
-0.531514131658606));
#33278=CARTESIAN_POINT('Ctrl Pts',(-0.8272294721363,0.133197165975861,-0.528036144124446));
#33279=CARTESIAN_POINT('Ctrl Pts',(-0.837864965156129,-0.0056907608296099,
-0.524558156590285));
#33280=CARTESIAN_POINT('Ctrl Pts',(-0.815167202467579,-0.138898928339155,
-0.521080169056125));
#33281=CARTESIAN_POINT('Ctrl Pts',(-0.792469439779029,-0.2721070958487,
-0.517602181521964));
#33282=CARTESIAN_POINT('Ctrl Pts',(-0.7364384213821,-0.399635504062319,
-0.514124193987804));
#33283=CARTESIAN_POINT('Ctrl Pts',(-0.653677666152339,-0.506454330661924,
-0.510646206453644));
#33284=CARTESIAN_POINT('Ctrl Pts',(-0.570916910922577,-0.61327315726153,
-0.507168218919484));
#33285=CARTESIAN_POINT('Ctrl Pts',(-0.461426418859984,-0.699382402247121,
-0.503690231385324));
#33286=CARTESIAN_POINT('Ctrl Pts',(-0.338110159082283,-0.754633686365735,
-0.500212243851163));
#33287=CARTESIAN_POINT('Ctrl Pts',(-0.214793899304584,-0.809884970484349,
-0.496734256317003));
#33288=CARTESIAN_POINT('Ctrl Pts',(-0.0776518718117775,-0.834278293735987,
-0.493256268782843));
#33289=CARTESIAN_POINT('Ctrl Pts',(0.0571530908599799,-0.824938788321738,
-0.489778281248683));
#33290=CARTESIAN_POINT('Ctrl Pts',(0.191958053531737,-0.815599282907488,
-0.486300293714522));
#33291=CARTESIAN_POINT('Ctrl Pts',(0.324425951382446,-0.772526948827351,
-0.482822306180362));
#33292=CARTESIAN_POINT('Ctrl Pts',(0.438944820023654,-0.700798063101624,
-0.479344318646202));
#33293=CARTESIAN_POINT('Ctrl Pts',(0.553463688664857,-0.6290691773759,-0.475866331112042));
#33294=CARTESIAN_POINT('Ctrl Pts',(0.650033528096561,-0.528683740004589,
-0.472388343577882));
#33295=CARTESIAN_POINT('Ctrl Pts',(0.717273128843357,-0.411472646614386,
-0.468910356043722));
#33296=CARTESIAN_POINT('Ctrl Pts',(0.784512729590156,-0.294261553224178,
-0.465432368509562));
#33297=CARTESIAN_POINT('Ctrl Pts',(0.822422091652043,-0.160224803815075,
-0.461954380975402));
#33298=CARTESIAN_POINT('Ctrl Pts',(0.826533418528118,-0.0251592593056256,
-0.458476393441242));
#33299=CARTESIAN_POINT('Ctrl Pts',(0.830644745404194,0.109906285203826,
-0.454998405907081));
#33300=CARTESIAN_POINT('Ctrl Pts',(0.800958037094456,0.246000624813626,
-0.451520418372921));
#33301=CARTESIAN_POINT('Ctrl Pts',(0.740972011706928,0.367084401928998,
-0.44804243083876));
#33302=CARTESIAN_POINT('Ctrl Pts',(0.680985986319401,0.488168179044368,
-0.4445644433046));
#33303=CARTESIAN_POINT('Ctrl Pts',(0.590700643854085,0.594241393665312,
-0.44108645577044));
#33304=CARTESIAN_POINT('Ctrl Pts',(0.480756536280454,0.672802818882485,
-0.43760846823628));
#33305=CARTESIAN_POINT('Ctrl Pts',(0.370812428706824,0.751364244099657,
-0.43413048070212));
#33306=CARTESIAN_POINT('Ctrl Pts',(0.241209556024878,0.802413879913057,
-0.43065249316796));
#33307=CARTESIAN_POINT('Ctrl Pts',(0.107222225940717,0.819935286798217,
-0.427174505633799));
#33308=CARTESIAN_POINT('Ctrl Pts',(-0.026765104143441,0.837456693683376,
-0.423696518099639));
#33309=CARTESIAN_POINT('Ctrl Pts',(-0.165136891629814,0.821449871640294,
-0.420218530565479));
#33310=CARTESIAN_POINT('Ctrl Pts',(-0.291585370986883,0.773801299882005,
-0.416740543031319));
#33311=CARTESIAN_POINT('Ctrl Pts',(-0.418033850343953,0.726152728123715,
-0.413262555497159));
#33312=CARTESIAN_POINT('Ctrl Pts',(-0.532559021571719,0.646862406650216,
-0.409784567962998));
#33313=CARTESIAN_POINT('Ctrl Pts',(-0.621663554948784,0.545275072528494,
-0.406306580428838));
#33314=CARTESIAN_POINT('Ctrl Pts',(-0.710768088325849,0.443687738406773,
-0.402828592894678));
#33315=CARTESIAN_POINT('Ctrl Pts',(-0.774451983852214,0.31980339163683,
-0.399350605360518));
#33316=CARTESIAN_POINT('Ctrl Pts',(-0.805209795112537,0.188222384767201,
-0.395872617826358));
#33317=CARTESIAN_POINT('Ctrl Pts',(-0.835967606372859,0.0566413778975711,
-0.392394630292197));
#33318=CARTESIAN_POINT('Ctrl Pts',(-0.833799333367139,-0.0826362890717455,
-0.388916642758037));
#33319=CARTESIAN_POINT('Ctrl Pts',(-0.798960517260377,-0.213196088453219,
-0.385438655223877));
#33320=CARTESIAN_POINT('Ctrl Pts',(-0.764121701153614,-0.343755887834692,
-0.381960667689717));
#33321=CARTESIAN_POINT('Ctrl Pts',(-0.69661234194581,-0.465597819628322,
-0.378482680155557));
#33322=CARTESIAN_POINT('Ctrl Pts',(-0.604388734927787,-0.564362239491933,
-0.375004692621396));
#33323=CARTESIAN_POINT('Ctrl Pts',(-0.512165127909764,-0.663126659355544,
-0.371526705087236));
#33324=CARTESIAN_POINT('Ctrl Pts',(-0.395227273081522,-0.738813567289136,
-0.368048717553076));
#33325=CARTESIAN_POINT('Ctrl Pts',(-0.267356846266645,-0.782502905444176,
-0.364570730018916));
#33326=CARTESIAN_POINT('Ctrl Pts',(-0.139486419451767,-0.826192243599216,
-0.361092742484755));
#33327=CARTESIAN_POINT('Ctrl Pts',(-0.00068342065025373,-0.837884011975705,
-0.357614754950595));
#33328=CARTESIAN_POINT('Ctrl Pts',(0.132693564325645,-0.816200280725187,
-0.354136767416435));
#33329=CARTESIAN_POINT('Ctrl Pts',(0.266070549301539,-0.794516549474669,
-0.350658779882275));
#33330=CARTESIAN_POINT('Ctrl Pts',(0.394021520451819,-0.739457318597146,
-0.347180792348115));
#33331=CARTESIAN_POINT('Ctrl Pts',(0.501466854431064,-0.657511577224771,
-0.343702804813955));
#33332=CARTESIAN_POINT('Ctrl Pts',(0.608912188410314,-0.575565835852392,
-0.340224817279795));
#33333=CARTESIAN_POINT('Ctrl Pts',(0.695851885218527,-0.466733583985158,
-0.336746829745634));
#33334=CARTESIAN_POINT('Ctrl Pts',(0.752039692950406,-0.343841214072583,
-0.333268842211474));
#33335=CARTESIAN_POINT('Ctrl Pts',(0.808227500682283,-0.22094884416001,
-0.329790854677314));
#33336=CARTESIAN_POINT('Ctrl Pts',(0.833663419337829,-0.0839963562020974,
-0.326312867143154));
#33337=CARTESIAN_POINT('Ctrl Pts',(0.825349706352788,0.0508757554542803,
-0.322834879608993));
#33338=CARTESIAN_POINT('Ctrl Pts',(0.817035993367747,0.185747867110658,
-0.319356892074833));
#33339=CARTESIAN_POINT('Ctrl Pts',(0.77497264874212,0.318539602465501,-0.315878904540673));
#33340=CARTESIAN_POINT('Ctrl Pts',(0.704117035339799,0.433600831232199,
-0.312400917006513));
#33341=CARTESIAN_POINT('Ctrl Pts',(0.633261421937478,0.548662059998898,
-0.308922929472353));
#33342=CARTESIAN_POINT('Ctrl Pts',(0.533613539758462,0.645992782177453,
-0.305444941938192));
#33343=CARTESIAN_POINT('Ctrl Pts',(0.416917360096601,0.714122114932397,
-0.301966954404032));
#33344=CARTESIAN_POINT('Ctrl Pts',(0.300221180434741,0.782251447687341,
-0.298488966869872));
#33345=CARTESIAN_POINT('Ctrl Pts',(0.166476703290036,0.821179391018675,
-0.295010979335712));
#33346=CARTESIAN_POINT('Ctrl Pts',(0.0314463438949348,0.826318103348088,
-0.291532991801552));
#33347=CARTESIAN_POINT('Ctrl Pts',(-0.103584015500168,0.831456815677501,
-0.288055004267391));
#33348=CARTESIAN_POINT('Ctrl Pts',(-0.239900257145666,0.802806297004992,
-0.284577016733231));
#33349=CARTESIAN_POINT('Ctrl Pts',(-0.361436871197806,0.743743146577004,
-0.281099029199071));
#33350=CARTESIAN_POINT('Ctrl Pts',(-0.482973485249941,0.684679996149019,
-0.277621041664911));
#33351=CARTESIAN_POINT('Ctrl Pts',(-0.589730471708718,0.595204213965558,
-0.27414305413075));
#33352=CARTESIAN_POINT('Ctrl Pts',(-0.669126018040221,0.485860939630323,
-0.27066506659659));
#33353=CARTESIAN_POINT('Ctrl Pts',(-0.748521564371728,0.376517665295085,
-0.26718707906243));
#33354=CARTESIAN_POINT('Ctrl Pts',(-0.800555670575959,0.247306898808072,
-0.26370909152827));
#33355=CARTESIAN_POINT('Ctrl Pts',(-0.819095872468406,0.113456740014413,
-0.26023110399411));
#33356=CARTESIAN_POINT('Ctrl Pts',(-0.837636074360853,-0.0203934187792456,
-0.25675311645995));
#33357=CARTESIAN_POINT('Ctrl Pts',(-0.822682371941516,-0.158882969879551,
-0.25327512892579));
#33358=CARTESIAN_POINT('Ctrl Pts',(-0.775997129713515,-0.28569027602439,
-0.249797141391629));
#33359=CARTESIAN_POINT('Ctrl Pts',(-0.729311887485514,-0.412497582169228,
-0.246319153857469));
#33360=CARTESIAN_POINT('Ctrl Pts',(-0.650895105448849,-0.5276226433586,
-0.242841166323309));
#33361=CARTESIAN_POINT('Ctrl Pts',(-0.549988569180364,-0.61749741574404,
-0.239363178789149));
#33362=CARTESIAN_POINT('Ctrl Pts',(-0.449082032911878,-0.70737218812948,
-0.235885191254988));
#33363=CARTESIAN_POINT('Ctrl Pts',(-0.325685742411572,-0.771996671710988,
-0.232407203720828));
#33364=CARTESIAN_POINT('Ctrl Pts',(-0.194342531999381,-0.803754595401515,
-0.228929216186668));
#33365=CARTESIAN_POINT('Ctrl Pts',(-0.062999321587187,-0.835512519092041,
-0.225451228652508));
#33366=CARTESIAN_POINT('Ctrl Pts',(0.0762908087368925,-0.834403882891585,
-0.221973241118347));
#33367=CARTESIAN_POINT('Ctrl Pts',(0.20711186536151,-0.800559289665402,
-0.218495253584187));
#33368=CARTESIAN_POINT('Ctrl Pts',(0.337932921986123,-0.766714696439221,
-0.215017266050027));
#33369=CARTESIAN_POINT('Ctrl Pts',(0.460284904911274,-0.700134146187317,
-0.211539278515867));
#33370=CARTESIAN_POINT('Ctrl Pts',(0.559748052092242,-0.608664578014513,
-0.208061290981707));
#33371=CARTESIAN_POINT('Ctrl Pts',(0.659211199273213,-0.517195009841706,
-0.204583303447547));
#33372=CARTESIAN_POINT('Ctrl Pts',(0.73578551071,-0.400836423747998,-0.201105315913387));
#33373=CARTESIAN_POINT('Ctrl Pts',(0.780446355236759,-0.273302013173154,
-0.197627328379226));
#33374=CARTESIAN_POINT('Ctrl Pts',(0.825107199763518,-0.145767602598309,
-0.194149340845066));
#33375=CARTESIAN_POINT('Ctrl Pts',(0.837854577380248,-0.00705736754232866,
-0.190671353310906));
#33376=CARTESIAN_POINT('Ctrl Pts',(0.817186127412104,0.126480620590223,
-0.187193365776746));
#33377=CARTESIAN_POINT('Ctrl Pts',(0.79651767744396,0.260018608722774,-0.183715378242586));
#33378=CARTESIAN_POINT('Ctrl Pts',(0.742433399890941,0.388384349931897,
-0.180237390708425));
#33379=CARTESIAN_POINT('Ctrl Pts',(0.661307424905583,0.496450160114778,
-0.176759403174265));
#33380=CARTESIAN_POINT('Ctrl Pts',(0.580181449920225,0.604515970297661,
-0.173281415640105));
#33381=CARTESIAN_POINT('Ctrl Pts',(0.472013777502527,0.692281849454302,
-0.169803428105944));
#33382=CARTESIAN_POINT('Ctrl Pts',(0.349552390106817,0.749402561227557,
-0.166325440571784));
#33383=CARTESIAN_POINT('Ctrl Pts',(0.227091002711111,0.80652327300081,-0.162847453037624));
#33384=CARTESIAN_POINT('Ctrl Pts',(0.0903359003373931,0.832998817390679,
-0.159369465503464));
#33385=CARTESIAN_POINT('Ctrl Pts',(-0.0445955159864317,0.825712101000813,
-0.155891477969304));
#33386=CARTESIAN_POINT('Ctrl Pts',(-0.179526932310259,0.818425384610948,
-0.152413490435144));
#33387=CARTESIAN_POINT('Ctrl Pts',(-0.312634662584192,0.777376407441347,
-0.148935502900983));
#33388=CARTESIAN_POINT('Ctrl Pts',(-0.428231669765076,0.707396742051747,
-0.145457515366823));
#33389=CARTESIAN_POINT('Ctrl Pts',(-0.543828676945959,0.637417076662149,
-0.141979527832663));
#33390=CARTESIAN_POINT('Ctrl Pts',(-0.641914961033792,0.538506723052553,
-0.138501540298503));
#33391=CARTESIAN_POINT('Ctrl Pts',(-0.710929916311705,0.422335058963057,
-0.135023552764343));
#33392=CARTESIAN_POINT('Ctrl Pts',(-0.779944871589619,0.30616339487356,
-0.131545565230183));
#33393=CARTESIAN_POINT('Ctrl Pts',(-0.819888498057611,0.172730420304163,
-0.128067577696022));
#33394=CARTESIAN_POINT('Ctrl Pts',(-0.826054786734804,0.0377369297661925,
-0.124589590161862));
#33395=CARTESIAN_POINT('Ctrl Pts',(-0.828767153927046,-0.0216426961432587,
-0.123059726774575));
#33396=CARTESIAN_POINT('Ctrl Pts',(-0.824944083444905,-0.081324259846495,
-0.121529863387287));
#33397=CARTESIAN_POINT('Ctrl Pts',(-0.814862045042685,-0.139933199781797,
-0.12));
#33398=CARTESIAN_POINT('',(0.589301091561375,0.565833523687252,-1.12625));
#33399=CARTESIAN_POINT('Ctrl Pts',(0.589301091561376,0.565833523687252,
-1.12625));
#33400=CARTESIAN_POINT('Ctrl Pts',(0.616667481029594,0.540044898914141,
-1.12625));
#33401=CARTESIAN_POINT('Ctrl Pts',(0.648190221269374,0.505777024736575,
-1.12625));
#33402=CARTESIAN_POINT('Ctrl Pts',(0.716478059012939,0.410513493212782,
-1.12625));
#33403=CARTESIAN_POINT('Ctrl Pts',(0.746976021141474,0.354408470381556,
-1.12625));
#33404=CARTESIAN_POINT('Ctrl Pts',(0.807743006623441,0.201482947924198,
-1.12625));
#33405=CARTESIAN_POINT('Ctrl Pts',(0.82685,0.101130131372722,-1.12625));
#33406=CARTESIAN_POINT('Ctrl Pts',(0.82685,-2.41473507855972E-15,-1.12625));
#33407=CARTESIAN_POINT('Ctrl Pts',(0.589258732516949,0.565791827419059,
-1.12625));
#33408=CARTESIAN_POINT('Ctrl Pts',(0.548574338866325,0.608188043340019,
-1.12472013661271));
#33409=CARTESIAN_POINT('Ctrl Pts',(0.400588145741329,0.732737761006617,
-1.11971228569126));
#33410=CARTESIAN_POINT('Ctrl Pts',(0.0845750992767496,0.846226087845691,
-1.11122644723566));
#33411=CARTESIAN_POINT('Ctrl Pts',(-0.323961995775536,0.786331547179378,
-1.10079248463318));
#33412=CARTESIAN_POINT('Ctrl Pts',(-0.656117677249231,0.541077762637851,
-1.0903585220307));
#33413=CARTESIAN_POINT('Ctrl Pts',(-0.833630685095572,0.168293731192072,
-1.07992455942822));
#33414=CARTESIAN_POINT('Ctrl Pts',(-0.814643797129343,-0.244162209445383,
-1.06949059682573));
#33415=CARTESIAN_POINT('Ctrl Pts',(-0.603640408739919,-0.59906504366349,
-1.05905663422325));
#33416=CARTESIAN_POINT('Ctrl Pts',(-0.250351927233723,-0.812763520669616,
-1.04862267162077));
#33417=CARTESIAN_POINT('Ctrl Pts',(0.161946157548482,-0.83488553496122,
-1.03818870901829));
#33418=CARTESIAN_POINT('Ctrl Pts',(0.536072366553592,-0.660217414778481,
-1.02775474641581));
#33419=CARTESIAN_POINT('Ctrl Pts',(0.783841098330601,-0.329929724332764,
-1.01732078381333));
#33420=CARTESIAN_POINT('Ctrl Pts',(0.846851206973997,0.0781254429130721,
-1.00688682121085));
#33421=CARTESIAN_POINT('Ctrl Pts',(0.710250478470445,0.467765739743977,
-0.99645285860837));
#33422=CARTESIAN_POINT('Ctrl Pts',(0.406237059412559,0.747149238803469,
-0.98601889600589));
#33423=CARTESIAN_POINT('Ctrl Pts',(0.00646973450489124,0.850422646762807,
-0.975584933403409));
#33424=CARTESIAN_POINT('Ctrl Pts',(-0.394822561461415,0.753243438481206,
-0.965150970800928));
#33425=CARTESIAN_POINT('Ctrl Pts',(-0.70305147134073,0.478517673019022,
-0.954717008198448));
#33426=CARTESIAN_POINT('Ctrl Pts',(-0.845564538846855,0.0910007927061355,
-0.944283045595966));
#33427=CARTESIAN_POINT('Ctrl Pts',(-0.788770096702248,-0.317965829356403,
-0.933849082993488));
#33428=CARTESIAN_POINT('Ctrl Pts',(-0.546055127582366,-0.651984916701293,
-0.923415120391005));
#33429=CARTESIAN_POINT('Ctrl Pts',(-0.174629831956392,-0.832325030110572,
-0.912981157788527));
#33430=CARTESIAN_POINT('Ctrl Pts',(0.237957356762351,-0.816478309791072,
-0.902547195186044));
#33431=CARTESIAN_POINT('Ctrl Pts',(0.594455759539154,-0.608179976581174,
-0.892113232583563));
#33432=CARTESIAN_POINT('Ctrl Pts',(0.810835351688311,-0.256527905763963,
-0.881679269981084));
#33433=CARTESIAN_POINT('Ctrl Pts',(0.836093429239885,0.155590203920442,
-0.871245307378603));
#33434=CARTESIAN_POINT('Ctrl Pts',(0.664276425899861,0.531034239923244,
-0.860811344776122));
#33435=CARTESIAN_POINT('Ctrl Pts',(0.335883224496111,0.78130851363521,-0.850377382173643));
#33436=CARTESIAN_POINT('Ctrl Pts',(-0.0716808103619117,0.847421026056225,
-0.83994341957116));
#33437=CARTESIAN_POINT('Ctrl Pts',(-0.462349004389065,0.71378843652532,
-0.829509456968681));
#33438=CARTESIAN_POINT('Ctrl Pts',(-0.744037191807753,0.411909202596062,
-0.819075494366199));
#33439=CARTESIAN_POINT('Ctrl Pts',(-0.850348818857665,0.0129390974967706,
-0.808641531763719));
#33440=CARTESIAN_POINT('Ctrl Pts',(-0.756225235669137,-0.389080874515506,
-0.798207569161239));
#33441=CARTESIAN_POINT('Ctrl Pts',(-0.483852255600829,-0.699390826881936,
-0.787773606558758));
#33442=CARTESIAN_POINT('Ctrl Pts',(-0.0974307504743614,-0.844847786786836,
-0.777339643956278));
#33443=CARTESIAN_POINT('Ctrl Pts',(0.31195609842859,-0.791166181424495,
-0.766905681353797));
#33444=CARTESIAN_POINT('Ctrl Pts',(0.647811962414489,-0.550999269808316,
-0.756471718751317));
#33445=CARTESIAN_POINT('Ctrl Pts',(0.830972457156651,-0.180956650675363,
-0.746037756148836));
#33446=CARTESIAN_POINT('Ctrl Pts',(0.818264932259306,0.231739152089763,
-0.735603793546355));
#33447=CARTESIAN_POINT('Ctrl Pts',(0.61268467079679,0.589811858262647,-0.725169830943875));
#33448=CARTESIAN_POINT('Ctrl Pts',(0.262688872936024,0.808860364965553,
-0.714735868341393));
#33449=CARTESIAN_POINT('Ctrl Pts',(-0.149225161660734,0.837252880021286,
-0.704301905738914));
#33450=CARTESIAN_POINT('Ctrl Pts',(-0.525965422875296,0.668297020729717,
-0.693867943136432));
#33451=CARTESIAN_POINT('Ctrl Pts',(-0.778730689623806,0.341817271381425,
-0.683433980533953));
#33452=CARTESIAN_POINT('Ctrl Pts',(-0.847941812434698,-0.0652320220563909,
-0.673000017931471));
#33453=CARTESIAN_POINT('Ctrl Pts',(-0.717285079048034,-0.456905514687298,
-0.662566055328991));
#33454=CARTESIAN_POINT('Ctrl Pts',(-0.417557509750833,-0.740882082404002,
-0.652132092726511));
#33455=CARTESIAN_POINT('Ctrl Pts',(-0.0194077101906125,-0.850225778697497,
-0.64169813012403));
#33456=CARTESIAN_POINT('Ctrl Pts',(0.383316669102108,-0.759163266475053,
-0.631264167521549));
#33457=CARTESIAN_POINT('Ctrl Pts',(0.695689706150894,-0.489158835893097,
-0.620830204919068));
#33458=CARTESIAN_POINT('Ctrl Pts',(0.844082139686513,-0.103855069394059,
-0.610396242316588));
#33459=CARTESIAN_POINT('Ctrl Pts',(0.793516478173853,0.305928313242129,
-0.599962279714107));
#33460=CARTESIAN_POINT('Ctrl Pts',(0.555911523369753,0.643601516593404,
-0.589528317111627));
#33461=CARTESIAN_POINT('Ctrl Pts',(0.187272996707217,0.829571792360918,
-0.579094354509145));
#33462=CARTESIAN_POINT('Ctrl Pts',(-0.225507535723485,0.820004198348112,
-0.568660391906667));
#33463=CARTESIAN_POINT('Ctrl Pts',(-0.585133822119268,0.617153906403178,
-0.558226429304184));
#33464=CARTESIAN_POINT('Ctrl Pts',(-0.806838566139564,0.26883463721489,
-0.547792466701705));
#33465=CARTESIAN_POINT('Ctrl Pts',(-0.838363875501719,-0.142851483122668,
-0.537358504099224));
#33466=CARTESIAN_POINT('Ctrl Pts',(-0.672278938438019,-0.520866166024689,
-0.526924541496743));
#33467=CARTESIAN_POINT('Ctrl Pts',(-0.347731535882056,-0.776107797235484,
-0.516490578894263));
#33468=CARTESIAN_POINT('Ctrl Pts',(0.0587794585027788,-0.848413524900876,
-0.506056616291782));
#33469=CARTESIAN_POINT('Ctrl Pts',(0.451435581967082,-0.720740209306132,
-0.495622653689302));
#33470=CARTESIAN_POINT('Ctrl Pts',(0.737684095078984,-0.423181651119364,
-0.485188691086821));
#33471=CARTESIAN_POINT('Ctrl Pts',(0.8500535324426,-0.0258751996797192,
-0.474754728484341));
#33472=CARTESIAN_POINT('Ctrl Pts',(0.762057361351743,0.377530279562069,
-0.46432076588186));
#33473=CARTESIAN_POINT('Ctrl Pts',(0.494437106533239,0.691948322969061,
-0.453886803279379));
#33474=CARTESIAN_POINT('Ctrl Pts',(0.110273377789823,0.843267642049257,
-0.443452840676899));
#33475=CARTESIAN_POINT('Ctrl Pts',(-0.299882822714386,0.795820850831186,
-0.433018878074418));
#33476=CARTESIAN_POINT('Ctrl Pts',(-0.639353822881232,0.560791604023703,
-0.422584915471937));
#33477=CARTESIAN_POINT('Ctrl Pts',(-0.828123116802314,0.193578504473992,
-0.412150952869457));
#33478=CARTESIAN_POINT('Ctrl Pts',(-0.821696007390509,-0.219262868301153,
-0.401716990266975));
#33479=CARTESIAN_POINT('Ctrl Pts',(-0.621587424751339,-0.580421921850917,
-0.391283027664496));
#33480=CARTESIAN_POINT('Ctrl Pts',(-0.274964842917688,-0.804770072220882,
-0.380849065062014));
#33481=CARTESIAN_POINT('Ctrl Pts',(0.13646953717677,-0.839426351377121,
-0.370415102459534));
#33482=CARTESIAN_POINT('Ctrl Pts',(0.515736764486322,-0.676221948589213,
-0.359981139857054));
#33483=CARTESIAN_POINT('Ctrl Pts',(0.773439988269239,-0.353625675685122,
-0.349547177254573));
#33484=CARTESIAN_POINT('Ctrl Pts',(0.848836136151768,0.052323493078395,
-0.339113214652093));
#33485=CARTESIAN_POINT('Ctrl Pts',(0.724153627343063,0.445939522912988,
-0.328679252049611));
#33486=CARTESIAN_POINT('Ctrl Pts',(0.428781301197021,0.734443414683683,
-0.318245289447132));
#33487=CARTESIAN_POINT('Ctrl Pts',(0.0323411916877329,0.849832090513251,
-0.30781132684465));
#33488=CARTESIAN_POINT('Ctrl Pts',(-0.37172204082515,0.764907351918341,
-0.297377364242171));
#33489=CARTESIAN_POINT('Ctrl Pts',(-0.688166893772679,0.499686763789961,
-0.286943401639689));
#33490=CARTESIAN_POINT('Ctrl Pts',(-0.842404341196427,0.116685300780257,
-0.276509439037209));
#33491=CARTESIAN_POINT('Ctrl Pts',(-0.798079165673276,-0.293819969988382,
-0.266075476434728));
#33492=CARTESIAN_POINT('Ctrl Pts',(-0.56563923004628,-0.635069140343264,
-0.255641513832248));
#33493=CARTESIAN_POINT('Ctrl Pts',(-0.199872807661205,-0.826626488317452,
-0.245207551229767));
#33494=CARTESIAN_POINT('Ctrl Pts',(0.213005508499054,-0.823340312573245,
-0.234773588627286));
#33495=CARTESIAN_POINT('Ctrl Pts',(0.575676435516449,-0.625984868845308,
-0.224339626024806));
#33496=CARTESIAN_POINT('Ctrl Pts',(0.802654992386147,-0.281079332570895,
-0.213905663422325));
#33497=CARTESIAN_POINT('Ctrl Pts',(0.840440266860438,0.130080080884023,
-0.203471700819845));
#33498=CARTESIAN_POINT('Ctrl Pts',(0.680125782303056,0.510576753259704,
-0.193037738217364));
#33499=CARTESIAN_POINT('Ctrl Pts',(0.359499429618306,0.770728914207567,
-0.182603775614884));
#33500=CARTESIAN_POINT('Ctrl Pts',(-0.0458646565737043,0.849206679729667,
-0.172169813012403));
#33501=CARTESIAN_POINT('Ctrl Pts',(-0.440417346097005,0.727530918967195,
-0.161735850409922));
#33502=CARTESIAN_POINT('Ctrl Pts',(-0.731160844709421,0.434344745947389,
-0.151301887807442));
#33503=CARTESIAN_POINT('Ctrl Pts',(-0.849560168473914,0.0388279800983712,
-0.140867925204961));
#33504=CARTESIAN_POINT('Ctrl Pts',(-0.767716584589541,-0.365940025647496,
-0.13043396260248));
#33505=CARTESIAN_POINT('Ctrl Pts',(-0.59249742112771,-0.578121984952217,
-0.12347798753416));
#33506=CARTESIAN_POINT('Ctrl Pts',(-0.485033396983252,-0.657408515958416,
-0.12));
#33507=CARTESIAN_POINT('Ctrl Pts',(0.546314451000132,0.524558727749236,
-1.15727273924394));
#33508=CARTESIAN_POINT('Ctrl Pts',(0.45933042519086,0.615150357993716,-1.15374460067508));
#33509=CARTESIAN_POINT('Ctrl Pts',(0.239517155169429,0.752140157504836,
-1.14668832353737));
#33510=CARTESIAN_POINT('Ctrl Pts',(-0.148496413265637,0.775239352992086,
-1.1361039078308));
#33511=CARTESIAN_POINT('Ctrl Pts',(-0.50041587773332,0.61042793059028,-1.12551949212423));
#33512=CARTESIAN_POINT('Ctrl Pts',(-0.731074678445066,0.297631408040497,
-1.11493507641766));
#33513=CARTESIAN_POINT('Ctrl Pts',(-0.784486575071109,-0.0873109114175124,
-1.10435066071109));
#33514=CARTESIAN_POINT('Ctrl Pts',(-0.647739858405562,-0.451090008407746,
-1.09376624500451));
#33515=CARTESIAN_POINT('Ctrl Pts',(-0.353965525798943,-0.705517309450159,
-1.08318182929794));
#33516=CARTESIAN_POINT('Ctrl Pts',(0.0256119661671953,-0.788917676587972,
-1.07259741359137));
#33517=CARTESIAN_POINT('Ctrl Pts',(0.398982356900775,-0.68107280850569,
-1.0620129978848));
#33518=CARTESIAN_POINT('Ctrl Pts',(0.675632891112325,-0.408126282767527,
-1.05142858217823));
#33519=CARTESIAN_POINT('Ctrl Pts',(0.788500750688368,-0.036244024752235,
-1.04084416647166));
#33520=CARTESIAN_POINT('Ctrl Pts',(0.710224521156416,0.344424265850668,
-1.03025975076509));
#33521=CARTESIAN_POINT('Ctrl Pts',(0.459779801870052,0.641599200064964,
-1.01967533505852));
#33522=CARTESIAN_POINT('Ctrl Pts',(0.0978778173933265,0.783241287520997,
-1.00909091935195));
#33523=CARTESIAN_POINT('Ctrl Pts',(-0.287751124101883,0.735014472176636,
-0.998506503645377));
#33524=CARTESIAN_POINT('Ctrl Pts',(-0.603625085401646,0.508609617298404,
-0.987922087938806));
#33525=CARTESIAN_POINT('Ctrl Pts',(-0.773171671953705,0.158910506780705,
-0.977337672232235));
#33526=CARTESIAN_POINT('Ctrl Pts',(-0.755290373416536,-0.229310787602247,
-0.966753256525666));
#33527=CARTESIAN_POINT('Ctrl Pts',(-0.554315867123394,-0.561943861908008,
-0.956168840819094));
#33528=CARTESIAN_POINT('Ctrl Pts',(-0.218967255152568,-0.758353694545466,
-0.945584425112523));
#33529=CARTESIAN_POINT('Ctrl Pts',(0.169462156609871,-0.770927728297872,
-0.935000009405953));
#33530=CARTESIAN_POINT('Ctrl Pts',(0.516811513855877,-0.596617837396195,
-0.924415593699381));
#33531=CARTESIAN_POINT('Ctrl Pts',(0.738878357065634,-0.277679236275885,
-0.913831177992811));
#33532=CARTESIAN_POINT('Ctrl Pts',(0.781830502198585,0.108572789396221,
-0.90324676228624));
#33533=CARTESIAN_POINT('Ctrl Pts',(0.635255734092279,0.468505215644773,
-0.892662346579668));
#33534=CARTESIAN_POINT('Ctrl Pts',(0.334685876135463,0.714865266390365,
-0.882077930873099));
#33535=CARTESIAN_POINT('Ctrl Pts',(-0.0470166324849965,0.78793173628669,
-0.871493515166526));
#33536=CARTESIAN_POINT('Ctrl Pts',(-0.417321635893158,0.669992266368472,
-0.860909099459958));
#33537=CARTESIAN_POINT('Ctrl Pts',(-0.686461896723765,0.389637073600391,
-0.850324683753385));
#33538=CARTESIAN_POINT('Ctrl Pts',(-0.789193960383511,0.0148282727314076,
-0.839740268046816));
#33539=CARTESIAN_POINT('Ctrl Pts',(-0.700614103026784,-0.363575113859105,
-0.829155852340243));
#33540=CARTESIAN_POINT('Ctrl Pts',(-0.442195350963467,-0.653842684721737,
-0.818571436633674));
#33541=CARTESIAN_POINT('Ctrl Pts',(-0.0765821114814572,-0.785609422664233,
-0.807987020927103));
#33542=CARTESIAN_POINT('Ctrl Pts',(0.30759572884442,-0.726933182881659,
-0.797402605220531));
#33543=CARTESIAN_POINT('Ctrl Pts',(0.617207958261565,-0.492037926420709,
-0.786818189513962));
#33544=CARTESIAN_POINT('Ctrl Pts',(0.777200137236411,-0.137865628267143,
-0.776233773807389));
#33545=CARTESIAN_POINT('Ctrl Pts',(0.748787869734938,0.249727273071264,
-0.76564935810082));
#33546=CARTESIAN_POINT('Ctrl Pts',(0.538858696398576,0.576782706132405,
-0.755064942394247));
#33547=CARTESIAN_POINT('Ctrl Pts',(0.198302456030384,0.764017748949664,
-0.744480526687679));
#33548=CARTESIAN_POINT('Ctrl Pts',(-0.190325140315885,0.76604394504593,
-0.733896110981106));
#33549=CARTESIAN_POINT('Ctrl Pts',(-0.532815196286454,0.582370115462685,
-0.723311695274537));
#33550=CARTESIAN_POINT('Ctrl Pts',(-0.746143216224096,0.257521427575564,
-0.712727279567965));
#33551=CARTESIAN_POINT('Ctrl Pts',(-0.778595432221924,-0.129754143290103,
-0.702142863861395));
#33552=CARTESIAN_POINT('Ctrl Pts',(-0.622304962251661,-0.48557545112449,
-0.691558448154824));
#33553=CARTESIAN_POINT('Ctrl Pts',(-0.315158855058534,-0.723686313851511,
-0.680974032448253));
#33554=CARTESIAN_POINT('Ctrl Pts',(0.0683862731776844,-0.786365247463709,
-0.670389616741682));
#33555=CARTESIAN_POINT('Ctrl Pts',(0.435353589178261,-0.65841798059242,
-0.659805201035111));
#33556=CARTESIAN_POINT('Ctrl Pts',(0.696784958823666,-0.37086076354192,
-0.649220785328541));
#33557=CARTESIAN_POINT('Ctrl Pts',(0.789305673168616,0.00659841508485431,
-0.638636369621969));
#33558=CARTESIAN_POINT('Ctrl Pts',(0.690487385718299,0.382458043374308,
-0.628051953915399));
#33559=CARTESIAN_POINT('Ctrl Pts',(0.424285064899531,0.665604363327791,
-0.617467538208828));
#33560=CARTESIAN_POINT('Ctrl Pts',(0.0552299665647796,0.787398650983761,
-0.606883122502258));
#33561=CARTESIAN_POINT('Ctrl Pts',(-0.32721366682163,0.71831622633972,-0.596298706795686));
#33562=CARTESIAN_POINT('Ctrl Pts',(-0.630336020111219,0.475103658718963,
-0.585714291089116));
#33563=CARTESIAN_POINT('Ctrl Pts',(-0.780655892709756,0.116719158475916,
-0.575129875382544));
#33564=CARTESIAN_POINT('Ctrl Pts',(-0.74173359420234,-0.269959737756342,
-0.564545459675975));
#33565=CARTESIAN_POINT('Ctrl Pts',(-0.523004447299988,-0.591196526446348,
-0.553961043969403));
#33566=CARTESIAN_POINT('Ctrl Pts',(-0.177491530455713,-0.769118808373767,
-0.543376628262832));
#33567=CARTESIAN_POINT('Ctrl Pts',(0.211047875895698,-0.760595673704307,
-0.532792212556262));
#33568=CARTESIAN_POINT('Ctrl Pts',(0.548426253918519,-0.567693252373757,
-0.522207796849691));
#33569=CARTESIAN_POINT('Ctrl Pts',(0.752858251913652,-0.237173854594718,
-0.511623381143121));
#33570=CARTESIAN_POINT('Ctrl Pts',(0.774786625126501,0.150839882998086,
-0.501038965436549));
#33571=CARTESIAN_POINT('Ctrl Pts',(0.608895621771471,0.502287872206101,
-0.490454549729978));
#33572=CARTESIAN_POINT('Ctrl Pts',(0.295399597411619,0.731974086035049,
-0.479870134023408));
#33573=CARTESIAN_POINT('Ctrl Pts',(-0.0897055208909264,0.784219296051476,
-0.469285718316836));
#33574=CARTESIAN_POINT('Ctrl Pts',(-0.453064735918975,0.646358514947008,
-0.458701302610267));
#33575=CARTESIAN_POINT('Ctrl Pts',(-0.706594568913721,0.351811170884782,
-0.448116886903694));
#33576=CARTESIAN_POINT('Ctrl Pts',(-0.788835756602106,-0.0280202406126237,
-0.437532471197125));
#33577=CARTESIAN_POINT('Ctrl Pts',(-0.679851857001817,-0.401059144402229,
-0.426948055490553));
#33578=CARTESIAN_POINT('Ctrl Pts',(-0.40606212854654,-0.676875566510091,
-0.416363639783983));
#33579=CARTESIAN_POINT('Ctrl Pts',(-0.0338371233843339,-0.788607655212058,
-0.405779224077412));
#33580=CARTESIAN_POINT('Ctrl Pts',(0.346590485190772,-0.709169951669667,
-0.395194808370841));
#33581=CARTESIAN_POINT('Ctrl Pts',(0.642999595336511,-0.45781929315021,
-0.38461039266427));
#33582=CARTESIAN_POINT('Ctrl Pts',(0.783536392737088,-0.0954866798141,-0.374025976957699));
#33583=CARTESIAN_POINT('Ctrl Pts',(0.734132744595485,0.28999327252795,-0.363441561251129));
#33584=CARTESIAN_POINT('Ctrl Pts',(0.506764802819446,0.605174701533931,
-0.352857145544558));
#33585=CARTESIAN_POINT('Ctrl Pts',(0.156549813679539,0.773653113881336,
-0.342272729837987));
#33586=CARTESIAN_POINT('Ctrl Pts',(-0.231615093084909,0.754586929064556,
-0.331688314131416));
#33587=CARTESIAN_POINT('Ctrl Pts',(-0.563633182964224,0.552598063281501,
-0.321103898424845));
#33588=CARTESIAN_POINT('Ctrl Pts',(-0.759018516340419,0.216651511277543,
-0.310519482718275));
#33589=CARTESIAN_POINT('Ctrl Pts',(-0.770406886705711,-0.171814470849813,
-0.299935067011703));
#33590=CARTESIAN_POINT('Ctrl Pts',(-0.595037595541406,-0.51863016343718,
-0.289350651305133));
#33591=CARTESIAN_POINT('Ctrl Pts',(-0.275422660164455,-0.739722476337532,
-0.278766235598562));
#33592=CARTESIAN_POINT('Ctrl Pts',(0.110958659106209,-0.781495462293021,
-0.268181819891991));
#33593=CARTESIAN_POINT('Ctrl Pts',(0.470442038027584,-0.633822758023187,
-0.25759740418542));
#33594=CARTESIAN_POINT('Ctrl Pts',(0.715883472822076,-0.332502328862273,
-0.24701298847885));
#33595=CARTESIAN_POINT('Ctrl Pts',(0.787784607225334,0.0494214101901685,
-0.236428572772279));
#33596=CARTESIAN_POINT('Ctrl Pts',(0.668715255345631,0.419364726111373,
-0.225844157065708));
#33597=CARTESIAN_POINT('Ctrl Pts',(0.387540164029798,0.687647957073736,
-0.215259741359137));
#33598=CARTESIAN_POINT('Ctrl Pts',(0.0124189653017137,0.789235606485634,
-0.204675325652566));
#33599=CARTESIAN_POINT('Ctrl Pts',(-0.36571115764945,0.699500976810335,
-0.194090909945996));
#33600=CARTESIAN_POINT('Ctrl Pts',(-0.655190820886875,0.440197805626221,
-0.183506494239425));
#33601=CARTESIAN_POINT('Ctrl Pts',(-0.785836630350134,0.0741833682121673,
-0.172922078532854));
#33602=CARTESIAN_POINT('Ctrl Pts',(-0.725996588748235,-0.309812190918388,
-0.162337662826283));
#33603=CARTESIAN_POINT('Ctrl Pts',(-0.490140575868305,-0.618708756217194,
-0.151753247119712));
#33604=CARTESIAN_POINT('Ctrl Pts',(-0.135514917188149,-0.777613622822952,
-0.141168831413142));
#33605=CARTESIAN_POINT('Ctrl Pts',(0.252058240770721,-0.748030699511341,
-0.130584415706571));
#33606=CARTESIAN_POINT('Ctrl Pts',(0.469550542503074,-0.607385125337196,
-0.123528138568857));
#33607=CARTESIAN_POINT('Ctrl Pts',(0.555007866453731,-0.51535192480862,
-0.12));
#33608=CARTESIAN_POINT('Ctrl Pts',(0.560643331187213,0.538316993061908,
-1.14693182616263));
#33609=CARTESIAN_POINT('Ctrl Pts',(0.471377865299377,0.631284684590047,
-1.14340368759377));
#33610=CARTESIAN_POINT('Ctrl Pts',(0.245799274584155,0.771867488863268,
-1.13634741045605));
#33611=CARTESIAN_POINT('Ctrl Pts',(-0.152391216542393,0.795572536170745,
-1.12576299474948));
#33612=CARTESIAN_POINT('Ctrl Pts',(-0.513540917978231,0.626438396109293,
-1.11517857904291));
#33613=CARTESIAN_POINT('Ctrl Pts',(-0.750249498836639,0.30543776347905,
-1.10459416333634));
#33614=CARTESIAN_POINT('Ctrl Pts',(-0.80506229684085,-0.0896009251384309,
-1.09400974762977));
#33615=CARTESIAN_POINT('Ctrl Pts',(-0.664728951054492,-0.46292131668127,
-1.0834253319232));
#33616=CARTESIAN_POINT('Ctrl Pts',(-0.363249427405876,-0.724021804395361,
-1.07284091621663));
#33617=CARTESIAN_POINT('Ctrl Pts',(0.0262837236026674,-0.809609618462482,
-1.06225650051006));
#33618=CARTESIAN_POINT('Ctrl Pts',(0.409446971882722,-0.698936166602645,
-1.05167208480349));
#33619=CARTESIAN_POINT('Ctrl Pts',(0.69335356961438,-0.41883072706013,-1.04108766909692));
#33620=CARTESIAN_POINT('Ctrl Pts',(0.809181757319902,-0.0371946426376338,
-1.03050325339035));
#33621=CARTESIAN_POINT('Ctrl Pts',(0.728852478097601,0.353457916763366,
-1.01991883768378));
#33622=CARTESIAN_POINT('Ctrl Pts',(0.47183902834919,0.658427233899741,-1.00933442197721));
#33623=CARTESIAN_POINT('Ctrl Pts',(0.100444982724272,0.803784347558888,
-0.998750006270634));
#33624=CARTESIAN_POINT('Ctrl Pts',(-0.295298336835145,0.754292626522195,
-0.988165590564065));
#33625=CARTESIAN_POINT('Ctrl Pts',(-0.619457124094387,0.521949565115864,
-0.977581174857492));
#33626=CARTESIAN_POINT('Ctrl Pts',(-0.793450623446179,0.163078453661775,
-0.966996759150923));
#33627=CARTESIAN_POINT('Ctrl Pts',(-0.775100329472668,-0.235325211703865,
-0.956412343444351));
#33628=CARTESIAN_POINT('Ctrl Pts',(-0.568854610572828,-0.576682674425972,
-0.945827927737781));
#33629=CARTESIAN_POINT('Ctrl Pts',(-0.224710386344195,-0.778243996199906,
-0.93524351203121));
#33630=CARTESIAN_POINT('Ctrl Pts',(0.173906854958709,-0.791147825041526,
-0.924659096324638));
#33631=CARTESIAN_POINT('Ctrl Pts',(0.530366583189642,-0.612266088131418,
-0.914074680618069));
#33632=CARTESIAN_POINT('Ctrl Pts',(0.75825785440794,-0.284962280866329,
-0.903490264911497));
#33633=CARTESIAN_POINT('Ctrl Pts',(0.802336559785201,0.111420465286886,
-0.892905849204926));
#33634=CARTESIAN_POINT('Ctrl Pts',(0.651917389820589,0.480793294588515,
-0.882321433498356));
#33635=CARTESIAN_POINT('Ctrl Pts',(0.343464105982164,0.733614942027283,
-0.871737017791784));
#33636=CARTESIAN_POINT('Ctrl Pts',(-0.0482497971806109,0.808597818657717,
-0.861152602085213));
#33637=CARTESIAN_POINT('Ctrl Pts',(-0.428267258344188,0.687565001070053,
-0.850568186378644));
#33638=CARTESIAN_POINT('Ctrl Pts',(-0.704466601254543,0.399856578015558,
-0.839983770672072));
#33639=CARTESIAN_POINT('Ctrl Pts',(-0.809893148702622,0.0152171925979075,
-0.829399354965503));
#33640=CARTESIAN_POINT('Ctrl Pts',(-0.718989995374629,-0.373111058288095,
-0.81881493925893));
#33641=CARTESIAN_POINT('Ctrl Pts',(-0.453793367804575,-0.670991843916457,
-0.80823052355236));
#33642=CARTESIAN_POINT('Ctrl Pts',(-0.0785907273946608,-0.806214594778186,
-0.797646107845789));
#33643=CARTESIAN_POINT('Ctrl Pts',(0.315663431129433,-0.745999379030153,
-0.787061692139219));
#33644=CARTESIAN_POINT('Ctrl Pts',(0.633396252142959,-0.504943227538546,
-0.776477276432648));
#33645=CARTESIAN_POINT('Ctrl Pts',(0.797584748383812,-0.141481604497939,
-0.765892860726077));
#33646=CARTESIAN_POINT('Ctrl Pts',(0.768427276401428,0.256277186163867,
-0.755308445019506));
#33647=CARTESIAN_POINT('Ctrl Pts',(0.552992025078289,0.591910715788788,
-0.744724029312936));
#33648=CARTESIAN_POINT('Ctrl Pts',(0.20350358539473,0.784056608923918,-0.734139613606364));
#33649=CARTESIAN_POINT('Ctrl Pts',(-0.195317038529785,0.786135948628314,
-0.723555197899794));
#33650=CARTESIAN_POINT('Ctrl Pts',(-0.546790014443777,0.597644673171574,
-0.712970782193222));
#33651=CARTESIAN_POINT('Ctrl Pts',(-0.765713258217504,0.264275767817858,
-0.702386366486653));
#33652=CARTESIAN_POINT('Ctrl Pts',(-0.799016639535941,-0.133157369343483,
-0.691801950780081));
#33653=CARTESIAN_POINT('Ctrl Pts',(-0.638626941704349,-0.498311252727784,
-0.681217535073511));
#33654=CARTESIAN_POINT('Ctrl Pts',(-0.323424925022022,-0.742667350258704,
-0.670633119366939));
#33655=CARTESIAN_POINT('Ctrl Pts',(0.0701799264720645,-0.806990243550787,
-0.660048703660369));
#33656=CARTESIAN_POINT('Ctrl Pts',(0.446772158478287,-0.675687141859632,
-0.649464287953797));
#33657=CARTESIAN_POINT('Ctrl Pts',(0.715060419362678,-0.380587797921394,
-0.638879872247227));
#33658=CARTESIAN_POINT('Ctrl Pts',(0.810007791520257,0.00677148006419363,
-0.628295456540657));
#33659=CARTESIAN_POINT('Ctrl Pts',(0.708597671841128,0.392489254282354,
-0.617711040834085));
#33660=CARTESIAN_POINT('Ctrl Pts',(0.435413326011759,0.683062010945683,
-0.607126625127515));
#33661=CARTESIAN_POINT('Ctrl Pts',(0.056678552763067,0.808050751452202,
-0.596542209420944));
#33662=CARTESIAN_POINT('Ctrl Pts',(-0.335795913582409,0.73715641466865,
-0.585957793714373));
#33663=CARTESIAN_POINT('Ctrl Pts',(-0.646868640277571,0.487564803376157,
-0.575373378007802));
#33664=CARTESIAN_POINT('Ctrl Pts',(-0.801131142327443,0.119780499493487,
-0.564788962301232));
#33665=CARTESIAN_POINT('Ctrl Pts',(-0.761187979460869,-0.277040313294047,
-0.554204546594661));
#33666=CARTESIAN_POINT('Ctrl Pts',(-0.536721946533173,-0.606702585601401,
-0.54362013088809));
#33667=CARTESIAN_POINT('Ctrl Pts',(-0.182146825349461,-0.78929146028631,
-0.533035715181518));
#33668=CARTESIAN_POINT('Ctrl Pts',(0.216583295509642,-0.780544778582221,
-0.522451299474949));
#33669=CARTESIAN_POINT('Ctrl Pts',(0.562810523032143,-0.58258286142837,
-0.511866883768377));
#33670=CARTESIAN_POINT('Ctrl Pts',(0.772604417642524,-0.243394513301027,
-0.501282468061807));
#33671=CARTESIAN_POINT('Ctrl Pts',(0.795107934038735,0.154796151419974,
-0.490698052355236));
#33672=CARTESIAN_POINT('Ctrl Pts',(0.624865897488743,0.5154620116181,-0.480113636648665));
#33673=CARTESIAN_POINT('Ctrl Pts',(0.303147416329596,0.751172496327223,
-0.469529220942095));
#33674=CARTESIAN_POINT('Ctrl Pts',(-0.0920583410636534,0.804788007556265,
-0.458944805235523));
#33675=CARTESIAN_POINT('Ctrl Pts',(-0.464947837868942,0.663311377353669,
-0.448360389528953));
#33676=CARTESIAN_POINT('Ctrl Pts',(-0.725127318505594,0.36103856750015,
-0.437775973822382));
#33677=CARTESIAN_POINT('Ctrl Pts',(-0.809525549857519,-0.0287551629084119,
-0.427191558115811));
#33678=CARTESIAN_POINT('Ctrl Pts',(-0.697683191659193,-0.411578229917086,
-0.41660714240924));
#33679=CARTESIAN_POINT('Ctrl Pts',(-0.416712433655261,-0.694628838231771,
-0.40602272670267));
#33680=CARTESIAN_POINT('Ctrl Pts',(-0.0347246124228582,-0.809291465763771,
-0.395438310996098));
#33681=CARTESIAN_POINT('Ctrl Pts',(0.355680952278343,-0.727770249082904,
-0.384853895289528));
#33682=CARTESIAN_POINT('Ctrl Pts',(0.659864359109556,-0.469827098887135,
-0.374269479582957));
#33683=CARTESIAN_POINT('Ctrl Pts',(0.804087192872788,-0.0979911297549973,
-0.363685063876386));
#33684=CARTESIAN_POINT('Ctrl Pts',(0.753387772756398,0.297599292924272,
-0.353100648169815));
#33685=CARTESIAN_POINT('Ctrl Pts',(0.520056364353901,0.621047383969216,
-0.342516232463245));
#33686=CARTESIAN_POINT('Ctrl Pts',(0.160655843676399,0.793944692760265,
-0.331931816756674));
#33687=CARTESIAN_POINT('Ctrl Pts',(-0.237689955121337,0.774378434995818,
-0.321347401050103));
#33688=CARTESIAN_POINT('Ctrl Pts',(-0.578416303442498,0.567091751716574,
-0.310762985343532));
#33689=CARTESIAN_POINT('Ctrl Pts',(-0.778926255117066,0.222333904525174,
-0.300178569636962));
#33690=CARTESIAN_POINT('Ctrl Pts',(-0.790613322678069,-0.17632086631987,
-0.28959415393039));
#33691=CARTESIAN_POINT('Ctrl Pts',(-0.610644399274519,-0.532232932794082,
-0.27900973822382));
#33692=CARTESIAN_POINT('Ctrl Pts',(-0.282646518678684,-0.759124113463783,
-0.268425322517249));
#33693=CARTESIAN_POINT('Ctrl Pts',(0.113868912219852,-0.801992732364212,
-0.257840906810678));
#33694=CARTESIAN_POINT('Ctrl Pts',(0.482780916462016,-0.650446829275436,
-0.247256491104107));
#33695=CARTESIAN_POINT('Ctrl Pts',(0.734659854247096,-0.341223288052482,
-0.236672075397537));
#33696=CARTESIAN_POINT('Ctrl Pts',(0.808446830656353,0.0507176480326692,
-0.226087659690966));
#33697=CARTESIAN_POINT('Ctrl Pts',(0.686254496263712,0.43036393527404,-0.215503243984395));
#33698=CARTESIAN_POINT('Ctrl Pts',(0.397704670145094,0.705683769909664,
-0.204918828277824));
#33699=CARTESIAN_POINT('Ctrl Pts',(0.0127446932145117,0.809935887109747,
-0.194334412571253));
#33700=CARTESIAN_POINT('Ctrl Pts',(-0.375303126800996,0.717847673788811,
-0.183749996864682));
#33701=CARTESIAN_POINT('Ctrl Pts',(-0.672375339354173,0.4517434303189,-0.173165581158112));
#33702=CARTESIAN_POINT('Ctrl Pts',(-0.80644776172748,0.0761290692512678,
-0.162581165451541));
#33703=CARTESIAN_POINT('Ctrl Pts',(-0.745038219657612,-0.31793802715801,
-0.15199674974497));
#33704=CARTESIAN_POINT('Ctrl Pts',(-0.50299611277308,-0.63493641342506,
-0.141412334038399));
#33705=CARTESIAN_POINT('Ctrl Pts',(-0.139069238345857,-0.798009078979886,
-0.130827918331829));
#33706=CARTESIAN_POINT('Ctrl Pts',(0.258669291101823,-0.767650246916566,
-0.120243502625257));
#33707=CARTESIAN_POINT('Ctrl Pts',(0.481866038556653,-0.623315783353728,
-0.113187225487544));
#33708=CARTESIAN_POINT('Ctrl Pts',(0.569564759844972,-0.528868711654082,
-0.109659086918687));
#33709=CARTESIAN_POINT('Ctrl Pts',(0.574972211374295,0.552075258374579,
-1.13659091308131));
#33710=CARTESIAN_POINT('Ctrl Pts',(0.483425305407893,0.647419011186379,
-1.13306277451246));
#33711=CARTESIAN_POINT('Ctrl Pts',(0.252081393998882,0.791594820221698,
-1.12600649737474));
#33712=CARTESIAN_POINT('Ctrl Pts',(-0.156286019819149,0.815905719349405,
-1.11542208166817));
#33713=CARTESIAN_POINT('Ctrl Pts',(-0.526665958223143,0.642448861628305,
-1.1048376659616));
#33714=CARTESIAN_POINT('Ctrl Pts',(-0.769424319228211,0.313244118917604,
-1.09425325025503));
#33715=CARTESIAN_POINT('Ctrl Pts',(-0.825638018610591,-0.0918909388593487,
-1.08366883454846));
#33716=CARTESIAN_POINT('Ctrl Pts',(-0.681718043703422,-0.474752624954795,
-1.07308441884189));
#33717=CARTESIAN_POINT('Ctrl Pts',(-0.372533329012808,-0.742526299340564,
-1.06250000313532));
#33718=CARTESIAN_POINT('Ctrl Pts',(0.0269554810381386,-0.830301560336992,
-1.05191558742875));
#33719=CARTESIAN_POINT('Ctrl Pts',(0.41991158686467,-0.716799524699601,
-1.04133117172218));
#33720=CARTESIAN_POINT('Ctrl Pts',(0.711074248116434,-0.429535171352733,
-1.0307467560156));
#33721=CARTESIAN_POINT('Ctrl Pts',(0.829862763951439,-0.0381452605230327,
-1.02016234030904));
#33722=CARTESIAN_POINT('Ctrl Pts',(0.747480435038786,0.362491567676063,
-1.00957792460246));
#33723=CARTESIAN_POINT('Ctrl Pts',(0.483898254828326,0.675255267734519,
-0.998993508895893));
#33724=CARTESIAN_POINT('Ctrl Pts',(0.103012148055218,0.82432740759678,-0.988409093189321));
#33725=CARTESIAN_POINT('Ctrl Pts',(-0.302845549568408,0.773570780867754,
-0.977824677482751));
#33726=CARTESIAN_POINT('Ctrl Pts',(-0.635289162787124,0.535289512933325,
-0.967240261776179));
#33727=CARTESIAN_POINT('Ctrl Pts',(-0.813729574938655,0.167246400542845,
-0.956655846069609));
#33728=CARTESIAN_POINT('Ctrl Pts',(-0.794910285528797,-0.241339635805483,
-0.946071430363039));
#33729=CARTESIAN_POINT('Ctrl Pts',(-0.583393354022263,-0.591421486943936,
-0.935487014656467));
#33730=CARTESIAN_POINT('Ctrl Pts',(-0.230453517535821,-0.798134297854346,
-0.924902598949897));
#33731=CARTESIAN_POINT('Ctrl Pts',(0.178351553307548,-0.811367921785181,
-0.914318183243325));
#33732=CARTESIAN_POINT('Ctrl Pts',(0.543921652523408,-0.627914338866641,
-0.903733767536756));
#33733=CARTESIAN_POINT('Ctrl Pts',(0.777637351750247,-0.292245325456773,
-0.893149351830183));
#33734=CARTESIAN_POINT('Ctrl Pts',(0.822842617371817,0.114268141177552,
-0.882564936123615));
#33735=CARTESIAN_POINT('Ctrl Pts',(0.668579045548899,0.493081373532257,
-0.871980520417042));
#33736=CARTESIAN_POINT('Ctrl Pts',(0.352242335828866,0.7523646176642,-0.861396104710472));
#33737=CARTESIAN_POINT('Ctrl Pts',(-0.049482961876225,0.829263901028744,
-0.8508116890039));
#33738=CARTESIAN_POINT('Ctrl Pts',(-0.439212880795219,0.705137735771634,
-0.840227273297331));
#33739=CARTESIAN_POINT('Ctrl Pts',(-0.72247130578532,0.410076082430724,
-0.829642857590758));
#33740=CARTESIAN_POINT('Ctrl Pts',(-0.830592337021733,0.0156061124644078,
-0.819058441884189));
#33741=CARTESIAN_POINT('Ctrl Pts',(-0.737365887722474,-0.382647002717086,
-0.808474026177617));
#33742=CARTESIAN_POINT('Ctrl Pts',(-0.465391384645683,-0.688141003111176,
-0.797889610471047));
#33743=CARTESIAN_POINT('Ctrl Pts',(-0.0805993433078642,-0.82681976689214,
-0.787305194764476));
#33744=CARTESIAN_POINT('Ctrl Pts',(0.323731133414446,-0.765065575178646,
-0.776720779057905));
#33745=CARTESIAN_POINT('Ctrl Pts',(0.649584546024354,-0.517848528656383,
-0.766136363351335));
#33746=CARTESIAN_POINT('Ctrl Pts',(0.817969359531213,-0.145097580728736,
-0.755551947644764));
#33747=CARTESIAN_POINT('Ctrl Pts',(0.788066683067918,0.262827099256472,
-0.744967531938192));
#33748=CARTESIAN_POINT('Ctrl Pts',(0.567125353758003,0.607038725445171,
-0.734383116231623));
#33749=CARTESIAN_POINT('Ctrl Pts',(0.208704714759077,0.804095468898173,
-0.72379870052505));
#33750=CARTESIAN_POINT('Ctrl Pts',(-0.200308936743686,0.806227952210697,
-0.713214284818482));
#33751=CARTESIAN_POINT('Ctrl Pts',(-0.560764832601099,0.612919230880464,
-0.702629869111908));
#33752=CARTESIAN_POINT('Ctrl Pts',(-0.785283300210913,0.271030108060151,
-0.692045453405339));
#33753=CARTESIAN_POINT('Ctrl Pts',(-0.819437846849956,-0.136560595396861,
-0.681461037698768));
#33754=CARTESIAN_POINT('Ctrl Pts',(-0.654948921157037,-0.511047054331079,
-0.670876621992197));
#33755=CARTESIAN_POINT('Ctrl Pts',(-0.33169099498551,-0.761648386665895,
-0.660292206285627));
#33756=CARTESIAN_POINT('Ctrl Pts',(0.0719735797664441,-0.827615239637866,
-0.649707790579055));
#33757=CARTESIAN_POINT('Ctrl Pts',(0.458190727778314,-0.692956303126841,
-0.639123374872485));
#33758=CARTESIAN_POINT('Ctrl Pts',(0.733335879901689,-0.390314832300869,
-0.628538959165914));
#33759=CARTESIAN_POINT('Ctrl Pts',(0.830709909871898,0.00694454504353371,
-0.617954543459343));
#33760=CARTESIAN_POINT('Ctrl Pts',(0.726707957963956,0.4025204651904,-0.607370127752773));
#33761=CARTESIAN_POINT('Ctrl Pts',(0.446541587123989,0.700519658563575,
-0.596785712046201));
#33762=CARTESIAN_POINT('Ctrl Pts',(0.0581271389613537,0.828702851920643,
-0.586201296339631));
#33763=CARTESIAN_POINT('Ctrl Pts',(-0.344378160343187,0.75599660299758,
-0.575616880633059));
#33764=CARTESIAN_POINT('Ctrl Pts',(-0.663401260443925,0.500025948033351,
-0.56503246492649));
#33765=CARTESIAN_POINT('Ctrl Pts',(-0.82160639194513,0.122841840511059,
-0.554448049219918));
#33766=CARTESIAN_POINT('Ctrl Pts',(-0.780642364719398,-0.284120888831752,
-0.543863633513348));
#33767=CARTESIAN_POINT('Ctrl Pts',(-0.550439445766359,-0.622208644756453,
-0.533279217806777));
#33768=CARTESIAN_POINT('Ctrl Pts',(-0.186802120243209,-0.809464112198856,
-0.522694802100206));
#33769=CARTESIAN_POINT('Ctrl Pts',(0.222118715123586,-0.800493883460134,
-0.512110386393635));
#33770=CARTESIAN_POINT('Ctrl Pts',(0.577194792145768,-0.597472470482985,
-0.501525970687065));
#33771=CARTESIAN_POINT('Ctrl Pts',(0.792350583371396,-0.249615172007336,
-0.490941554980494));
#33772=CARTESIAN_POINT('Ctrl Pts',(0.815429242950967,0.158752419841862,
-0.480357139273923));
#33773=CARTESIAN_POINT('Ctrl Pts',(0.640836173206014,0.528636151030098,
-0.469772723567352));
#33774=CARTESIAN_POINT('Ctrl Pts',(0.310895235247574,0.770370906619397,
-0.459188307860781));
#33775=CARTESIAN_POINT('Ctrl Pts',(-0.0944111612363807,0.825356719061054,
-0.44860389215421));
#33776=CARTESIAN_POINT('Ctrl Pts',(-0.476830939818908,0.68026423976033,
-0.43801947644764));
#33777=CARTESIAN_POINT('Ctrl Pts',(-0.743660068097467,0.370265964115517,
-0.427435060741069));
#33778=CARTESIAN_POINT('Ctrl Pts',(-0.830215343112932,-0.0294900852041995,
-0.416850645034497));
#33779=CARTESIAN_POINT('Ctrl Pts',(-0.71551452631657,-0.422097315431943,
-0.406266229327927));
#33780=CARTESIAN_POINT('Ctrl Pts',(-0.427362738763982,-0.71238210995345,
-0.395681813621356));
#33781=CARTESIAN_POINT('Ctrl Pts',(-0.0356121014613823,-0.829975276315481,
-0.385097397914785));
#33782=CARTESIAN_POINT('Ctrl Pts',(0.364771419365913,-0.746370546496145,
-0.374512982208215));
#33783=CARTESIAN_POINT('Ctrl Pts',(0.676729122882603,-0.481834904624058,
-0.363928566501644));
#33784=CARTESIAN_POINT('Ctrl Pts',(0.824637993008486,-0.100495579695895,
-0.353344150795073));
#33785=CARTESIAN_POINT('Ctrl Pts',(0.772642800917313,0.305205313320593,
-0.342759735088502));
#33786=CARTESIAN_POINT('Ctrl Pts',(0.533347925888355,0.636920066404502,
-0.332175319381931));
#33787=CARTESIAN_POINT('Ctrl Pts',(0.164761873673258,0.814236271639193,
-0.321590903675361));
#33788=CARTESIAN_POINT('Ctrl Pts',(-0.243764817157765,0.794169940927082,
-0.311006487968789));
#33789=CARTESIAN_POINT('Ctrl Pts',(-0.593199423920774,0.581585440151646,
-0.300422072262219));
#33790=CARTESIAN_POINT('Ctrl Pts',(-0.798833993893712,0.228016297772806,
-0.289837656555648));
#33791=CARTESIAN_POINT('Ctrl Pts',(-0.810819758650429,-0.180827261789927,
-0.279253240849077));
#33792=CARTESIAN_POINT('Ctrl Pts',(-0.62625120300763,-0.545835702150984,
-0.268668825142506));
#33793=CARTESIAN_POINT('Ctrl Pts',(-0.289870377192915,-0.778525750590034,
-0.258084409435936));
#33794=CARTESIAN_POINT('Ctrl Pts',(0.116779165333497,-0.822490002435403,
-0.247499993729365));
#33795=CARTESIAN_POINT('Ctrl Pts',(0.495119794896445,-0.667070900527686,
-0.236915578022794));
#33796=CARTESIAN_POINT('Ctrl Pts',(0.753436235672117,-0.34994424724269,
-0.226331162316223));
#33797=CARTESIAN_POINT('Ctrl Pts',(0.82910905408737,0.0520138858751696,
-0.215746746609652));
#33798=CARTESIAN_POINT('Ctrl Pts',(0.703793737181796,0.441363144436706,
-0.205162330903082));
#33799=CARTESIAN_POINT('Ctrl Pts',(0.407869176260388,0.723719582745591,
-0.194577915196511));
#33800=CARTESIAN_POINT('Ctrl Pts',(0.0130704211273114,0.830636167733861,
-0.18399349948994));
#33801=CARTESIAN_POINT('Ctrl Pts',(-0.384895095952544,0.736194370767287,
-0.173409083783369));
#33802=CARTESIAN_POINT('Ctrl Pts',(-0.68955985782147,0.463289055011579,
-0.162824668076798));
#33803=CARTESIAN_POINT('Ctrl Pts',(-0.827058893104828,0.0780747702903682,
-0.152240252370227));
#33804=CARTESIAN_POINT('Ctrl Pts',(-0.764079850566988,-0.326063863397633,
-0.141655836663657));
#33805=CARTESIAN_POINT('Ctrl Pts',(-0.515851649677855,-0.651164070632928,
-0.131071420957086));
#33806=CARTESIAN_POINT('Ctrl Pts',(-0.142623559503565,-0.818404535136818,
-0.120487005250515));
#33807=CARTESIAN_POINT('Ctrl Pts',(0.265280341432924,-0.787269794321791,
-0.109902589543944));
#33808=CARTESIAN_POINT('Ctrl Pts',(0.494181534610232,-0.639246441370259,
-0.10284631240623));
#33809=CARTESIAN_POINT('Ctrl Pts',(0.584121653236212,-0.542385498499545,
-0.0993181738373734));
#33810=CARTESIAN_POINT('Ctrl Pts',(0.589301091561376,0.565833523687251,
-1.12625));
#33811=CARTESIAN_POINT('Ctrl Pts',(0.49547274551641,0.663553337782711,-1.12272186143114));
#33812=CARTESIAN_POINT('Ctrl Pts',(0.258363513413608,0.81132215158013,-1.11566558429343));
#33813=CARTESIAN_POINT('Ctrl Pts',(-0.160180823095904,0.836238902528062,
-1.10508116858686));
#33814=CARTESIAN_POINT('Ctrl Pts',(-0.539790998468055,0.658459327147319,
-1.09449675288029));
#33815=CARTESIAN_POINT('Ctrl Pts',(-0.788599139619784,0.321050474356156,
-1.08391233717372));
#33816=CARTESIAN_POINT('Ctrl Pts',(-0.846213740380332,-0.0941809525802668,
-1.07332792146714));
#33817=CARTESIAN_POINT('Ctrl Pts',(-0.698707136352351,-0.486583933228319,
-1.06274350576058));
#33818=CARTESIAN_POINT('Ctrl Pts',(-0.381817230619741,-0.761030794285767,
-1.052159090054));
#33819=CARTESIAN_POINT('Ctrl Pts',(0.0276272384736108,-0.850993502211501,
-1.04157467434743));
#33820=CARTESIAN_POINT('Ctrl Pts',(0.430376201846617,-0.734662882796558,
-1.03099025864086));
#33821=CARTESIAN_POINT('Ctrl Pts',(0.728794926618489,-0.440239615645336,
-1.02040584293429));
#33822=CARTESIAN_POINT('Ctrl Pts',(0.850543770582973,-0.0390958784084322,
-1.00982142722772));
#33823=CARTESIAN_POINT('Ctrl Pts',(0.766108391979972,0.371525218588761,
-0.99923701152115));
#33824=CARTESIAN_POINT('Ctrl Pts',(0.495957481307464,0.692083301569296,
-0.988652595814578));
#33825=CARTESIAN_POINT('Ctrl Pts',(0.105579313386164,0.844870467634671,
-0.978068180108008));
#33826=CARTESIAN_POINT('Ctrl Pts',(-0.31039276230167,0.792848935213314,
-0.967483764401438));
#33827=CARTESIAN_POINT('Ctrl Pts',(-0.651121201479864,0.548629460750785,
-0.956899348694866));
#33828=CARTESIAN_POINT('Ctrl Pts',(-0.834008526431131,0.171414347423915,
-0.946314932988296));
#33829=CARTESIAN_POINT('Ctrl Pts',(-0.814720241584927,-0.247354059907101,
-0.935730517281725));
#33830=CARTESIAN_POINT('Ctrl Pts',(-0.597932097471697,-0.606160299461901,
-0.925146101575155));
#33831=CARTESIAN_POINT('Ctrl Pts',(-0.236196648727449,-0.818024599508785,
-0.914561685868583));
#33832=CARTESIAN_POINT('Ctrl Pts',(0.182796251656386,-0.831588018528835,
-0.903977270162012));
#33833=CARTESIAN_POINT('Ctrl Pts',(0.557476721857173,-0.643562589601863,
-0.893392854455442));
#33834=CARTESIAN_POINT('Ctrl Pts',(0.797016849092553,-0.299528370047217,
-0.88280843874887));
#33835=CARTESIAN_POINT('Ctrl Pts',(0.843348674958434,0.117115817068219,
-0.8722240230423));
#33836=CARTESIAN_POINT('Ctrl Pts',(0.685240701277208,0.505369452475997,
-0.86163960733573));
#33837=CARTESIAN_POINT('Ctrl Pts',(0.361020565675568,0.771114293301119,
-0.851055191629158));
#33838=CARTESIAN_POINT('Ctrl Pts',(-0.0507161265718393,0.84992998339977,
-0.840470775922587));
#33839=CARTESIAN_POINT('Ctrl Pts',(-0.45015850324625,0.722710470473215,
-0.829886360216017));
#33840=CARTESIAN_POINT('Ctrl Pts',(-0.740476010316097,0.420295586845891,
-0.819301944509446));
#33841=CARTESIAN_POINT('Ctrl Pts',(-0.851291525340844,0.0159950323309077,
-0.808717528802875));
#33842=CARTESIAN_POINT('Ctrl Pts',(-0.755741780070319,-0.392182947146075,
-0.798133113096305));
#33843=CARTESIAN_POINT('Ctrl Pts',(-0.476989401486791,-0.705290162305896,
-0.787548697389733));
#33844=CARTESIAN_POINT('Ctrl Pts',(-0.0826079592210675,-0.847424939006093,
-0.776964281683163));
#33845=CARTESIAN_POINT('Ctrl Pts',(0.33179883569946,-0.78413177132714,-0.766379865976592));
#33846=CARTESIAN_POINT('Ctrl Pts',(0.665772839905748,-0.530753829774219,
-0.755795450270021));
#33847=CARTESIAN_POINT('Ctrl Pts',(0.838353970678615,-0.148713556959532,
-0.74521103456345));
#33848=CARTESIAN_POINT('Ctrl Pts',(0.807706089734408,0.269377012349075,
-0.73462661885688));
#33849=CARTESIAN_POINT('Ctrl Pts',(0.581258682437717,0.622166735101554,
-0.724042203150308));
#33850=CARTESIAN_POINT('Ctrl Pts',(0.213905844123423,0.824134328872426,
-0.713457787443738));
#33851=CARTESIAN_POINT('Ctrl Pts',(-0.205300834957585,0.826319955793079,
-0.702873371737167));
#33852=CARTESIAN_POINT('Ctrl Pts',(-0.574739650758423,0.628193788589353,
-0.692288956030596));
#33853=CARTESIAN_POINT('Ctrl Pts',(-0.804853342204321,0.277784448302445,
-0.681704540324025));
#33854=CARTESIAN_POINT('Ctrl Pts',(-0.839859054163973,-0.13996382145024,
-0.671120124617455));
#33855=CARTESIAN_POINT('Ctrl Pts',(-0.671270900609725,-0.523782855934373,
-0.660535708910883));
#33856=CARTESIAN_POINT('Ctrl Pts',(-0.339957064948998,-0.780629423073089,
-0.649951293204314));
#33857=CARTESIAN_POINT('Ctrl Pts',(0.0737672330608236,-0.848240235724943,
-0.639366877497742));
#33858=CARTESIAN_POINT('Ctrl Pts',(0.469609297078341,-0.710225464394054,
-0.628782461791172));
#33859=CARTESIAN_POINT('Ctrl Pts',(0.751611340440699,-0.400041866680343,
-0.618198046084599));
#33860=CARTESIAN_POINT('Ctrl Pts',(0.85141202822354,0.00711761002287252,
-0.607613630378031));
#33861=CARTESIAN_POINT('Ctrl Pts',(0.744818244086785,0.412551676098446,
-0.597029214671458));
#33862=CARTESIAN_POINT('Ctrl Pts',(0.457669848236219,0.717977306181466,
-0.58644479896489));
#33863=CARTESIAN_POINT('Ctrl Pts',(0.0595757251596406,0.849354952389083,
-0.575860383258316));
#33864=CARTESIAN_POINT('Ctrl Pts',(-0.352960407103966,0.77483679132651,
-0.565275967551747));
#33865=CARTESIAN_POINT('Ctrl Pts',(-0.679933880610278,0.512487092690545,
-0.554691551845175));
#33866=CARTESIAN_POINT('Ctrl Pts',(-0.842081641562816,0.12590318152863,
-0.544107136138606));
#33867=CARTESIAN_POINT('Ctrl Pts',(-0.800096749977928,-0.291201464369457,
-0.533522720432034));
#33868=CARTESIAN_POINT('Ctrl Pts',(-0.564156944999544,-0.637714703911506,
-0.522938304725464));
#33869=CARTESIAN_POINT('Ctrl Pts',(-0.191457415136958,-0.829636764111399,
-0.512353889018893));
#33870=CARTESIAN_POINT('Ctrl Pts',(0.22765413473753,-0.820442988338048,
-0.501769473312322));
#33871=CARTESIAN_POINT('Ctrl Pts',(0.591579061259393,-0.6123620795376,-0.491185057605751));
#33872=CARTESIAN_POINT('Ctrl Pts',(0.812096749100267,-0.255835830713644,
-0.48060064189918));
#33873=CARTESIAN_POINT('Ctrl Pts',(0.835750551863201,0.162708688263749,
-0.47001622619261));
#33874=CARTESIAN_POINT('Ctrl Pts',(0.656806448923285,0.541810290442097,
-0.459431810486038));
#33875=CARTESIAN_POINT('Ctrl Pts',(0.318643054165552,0.789569316911571,
-0.448847394779468));
#33876=CARTESIAN_POINT('Ctrl Pts',(-0.0967639814091079,0.845925430565843,
-0.438262979072897));
#33877=CARTESIAN_POINT('Ctrl Pts',(-0.488714041768874,0.697217102166991,
-0.427678563366326));
#33878=CARTESIAN_POINT('Ctrl Pts',(-0.762192817689339,0.379493360730885,
-0.417094147659756));
#33879=CARTESIAN_POINT('Ctrl Pts',(-0.850905136368346,-0.0302250074999876,
-0.406509731953184));
#33880=CARTESIAN_POINT('Ctrl Pts',(-0.733345860973945,-0.4326164009468,
-0.395925316246614));
#33881=CARTESIAN_POINT('Ctrl Pts',(-0.438013043872703,-0.730135381675129,
-0.385340900540043));
#33882=CARTESIAN_POINT('Ctrl Pts',(-0.0364995904999063,-0.850659086867193,
-0.374756484833472));
#33883=CARTESIAN_POINT('Ctrl Pts',(0.373861886453484,-0.764970843909383,
-0.364172069126902));
#33884=CARTESIAN_POINT('Ctrl Pts',(0.693593886655648,-0.493842710360983,
-0.35358765342033));
#33885=CARTESIAN_POINT('Ctrl Pts',(0.845188793144185,-0.103000029636792,
-0.34300323771376));
#33886=CARTESIAN_POINT('Ctrl Pts',(0.791897829078227,0.312811333716915,
-0.332418822007189));
#33887=CARTESIAN_POINT('Ctrl Pts',(0.54663948742281,0.652792748839787,-0.321834406300618));
#33888=CARTESIAN_POINT('Ctrl Pts',(0.168867903670117,0.834527850518123,
-0.311249990594047));
#33889=CARTESIAN_POINT('Ctrl Pts',(-0.249839679194194,0.813961446858345,
-0.300665574887476));
#33890=CARTESIAN_POINT('Ctrl Pts',(-0.607982544399048,0.596079128586719,
-0.290081159180906));
#33891=CARTESIAN_POINT('Ctrl Pts',(-0.818741732670359,0.233698691020436,
-0.279496743474335));
#33892=CARTESIAN_POINT('Ctrl Pts',(-0.831026194622787,-0.185333657259983,
-0.268912327767764));
#33893=CARTESIAN_POINT('Ctrl Pts',(-0.641858006740743,-0.559438471507887,
-0.258327912061193));
#33894=CARTESIAN_POINT('Ctrl Pts',(-0.297094235707144,-0.797927387716284,
-0.247743496354622));
#33895=CARTESIAN_POINT('Ctrl Pts',(0.119689418447141,-0.842987272506595,
-0.237159080648052));
#33896=CARTESIAN_POINT('Ctrl Pts',(0.507458673330876,-0.683694971779935,
-0.226574664941481));
#33897=CARTESIAN_POINT('Ctrl Pts',(0.772212617097137,-0.358665206432899,
-0.21599024923491));
#33898=CARTESIAN_POINT('Ctrl Pts',(0.849771277518388,0.0533101237176703,
-0.205405833528339));
#33899=CARTESIAN_POINT('Ctrl Pts',(0.721332978099877,0.452362353599373,
-0.194821417821768));
#33900=CARTESIAN_POINT('Ctrl Pts',(0.418033682375684,0.741755395581518,
-0.184237002115198));
#33901=CARTESIAN_POINT('Ctrl Pts',(0.0133961490401099,0.851336448357973,
-0.173652586408627));
#33902=CARTESIAN_POINT('Ctrl Pts',(-0.39448706510409,0.754541067745763,
-0.163068170702056));
#33903=CARTESIAN_POINT('Ctrl Pts',(-0.706744376288768,0.474834679704258,
-0.152483754995485));
#33904=CARTESIAN_POINT('Ctrl Pts',(-0.847670024482173,0.0800204713294688,
-0.141899339288914));
#33905=CARTESIAN_POINT('Ctrl Pts',(-0.783121481476366,-0.334189699637256,
-0.131314923582344));
#33906=CARTESIAN_POINT('Ctrl Pts',(-0.528707186582629,-0.667391727840794,
-0.120730507875773));
#33907=CARTESIAN_POINT('Ctrl Pts',(-0.146177880661274,-0.838799991293752,
-0.110146092169202));
#33908=CARTESIAN_POINT('Ctrl Pts',(0.271891391764026,-0.806889341727016,
-0.099561676462631));
#33909=CARTESIAN_POINT('Ctrl Pts',(0.506497030663811,-0.65517709938679,
-0.0925053993249171));
#33910=CARTESIAN_POINT('Ctrl Pts',(0.598678546627452,-0.555902285345007,
-0.0889772607560602));
#33911=CARTESIAN_POINT('',(0.555007866453735,-0.515351924808616,-0.12));
#33912=CARTESIAN_POINT('Ctrl Pts',(-0.485074560134038,-0.657451903693333,
-0.12));
#33913=CARTESIAN_POINT('Ctrl Pts',(-0.453585509292975,-0.678311536271596,
-0.12));
#33914=CARTESIAN_POINT('Ctrl Pts',(-0.420738538427646,-0.69688883557989,
-0.12));
#33915=CARTESIAN_POINT('Ctrl Pts',(-0.386803943986752,-0.713111122122748,
-0.12));
#33916=CARTESIAN_POINT('Ctrl Pts',(-0.352869989073431,-0.729333102942208,
-0.12));
#33917=CARTESIAN_POINT('Ctrl Pts',(-0.317847265092479,-0.743200535648918,
-0.12));
#33918=CARTESIAN_POINT('Ctrl Pts',(-0.281986661943899,-0.754592743143177,
-0.12));
#33919=CARTESIAN_POINT('Ctrl Pts',(-0.25594917278718,-0.762864340747765,
-0.12));
#33920=CARTESIAN_POINT('Ctrl Pts',(-0.229469505296541,-0.769830064822657,
-0.12));
#33921=CARTESIAN_POINT('Ctrl Pts',(-0.202642618162792,-0.775426102639142,
-0.12));
#33922=CARTESIAN_POINT('Ctrl Pts',(-0.195274171502223,-0.776963146648598,
-0.12));
#33923=CARTESIAN_POINT('Ctrl Pts',(-0.187880255104256,-0.778396492223848,
-0.12));
#33924=CARTESIAN_POINT('Ctrl Pts',(-0.180475767737279,-0.77972273894194,
-0.12));
#33925=CARTESIAN_POINT('Ctrl Pts',(-0.166033419323757,-0.782309564502668,
-0.12));
#33926=CARTESIAN_POINT('Ctrl Pts',(-0.151538081912919,-0.784491790556042,
-0.12));
#33927=CARTESIAN_POINT('Ctrl Pts',(-0.137004865545513,-0.786263720842398,
-0.12));
#33928=CARTESIAN_POINT('Ctrl Pts',(-0.100095238310191,-0.790763845570673,
-0.12));
#33929=CARTESIAN_POINT('Ctrl Pts',(-0.062941216534269,-0.792621345331588,
-0.12));
#33930=CARTESIAN_POINT('Ctrl Pts',(-0.0258198641282856,-0.791883010674467,
-0.12));
#33931=CARTESIAN_POINT('Ctrl Pts',(0.0040257252501598,-0.79128938917169,
-0.12));
#33932=CARTESIAN_POINT('Ctrl Pts',(0.033850610796128,-0.789016694488584,
-0.12));
#33933=CARTESIAN_POINT('Ctrl Pts',(0.0635063571245307,-0.78506522308135,
-0.12));
#33934=CARTESIAN_POINT('Ctrl Pts',(0.0773427424554382,-0.783221597889486,
-0.12));
#33935=CARTESIAN_POINT('Ctrl Pts',(0.0911422070143154,-0.78101223318484,
-0.12));
#33936=CARTESIAN_POINT('Ctrl Pts',(0.104888951391214,-0.778435636708654,
-0.12));
#33937=CARTESIAN_POINT('Ctrl Pts',(0.11244272845885,-0.777019807997451,
-0.12));
#33938=CARTESIAN_POINT('Ctrl Pts',(0.119978617799766,-0.775493331514105,
-0.12));
#33939=CARTESIAN_POINT('Ctrl Pts',(0.127482778723967,-0.773858786231397,
-0.12));
#33940=CARTESIAN_POINT('Ctrl Pts',(0.163232326177276,-0.766071872445965,
-0.12));
#33941=CARTESIAN_POINT('Ctrl Pts',(0.19833507148298,-0.755823166544053,
-0.12));
#33942=CARTESIAN_POINT('Ctrl Pts',(0.232522340421131,-0.743135834967468,
-0.12));
#33943=CARTESIAN_POINT('Ctrl Pts',(0.23781323037933,-0.741172318216354,
-0.12));
#33944=CARTESIAN_POINT('Ctrl Pts',(0.24308215822664,-0.739150297994117,
-0.12));
#33945=CARTESIAN_POINT('Ctrl Pts',(0.248328083260998,-0.737069756703629,
-0.12));
#33946=CARTESIAN_POINT('Ctrl Pts',(0.277906408593185,-0.725338951029881,
-0.12));
#33947=CARTESIAN_POINT('Ctrl Pts',(0.306754972760513,-0.711749564176307,
-0.12));
#33948=CARTESIAN_POINT('Ctrl Pts',(0.33471754468048,-0.696396977944507,
-0.12));
#33949=CARTESIAN_POINT('Ctrl Pts',(0.341939489363331,-0.69243183736938,
-0.12));
#33950=CARTESIAN_POINT('Ctrl Pts',(0.349102231022204,-0.688348968693442,
-0.12));
#33951=CARTESIAN_POINT('Ctrl Pts',(0.356202844546331,-0.68414978827903,
-0.12));
#33952=CARTESIAN_POINT('Ctrl Pts',(0.363162967591196,-0.680033691511815,
-0.12));
#33953=CARTESIAN_POINT('Ctrl Pts',(0.370055970561641,-0.675810190933559,
-0.12));
#33954=CARTESIAN_POINT('Ctrl Pts',(0.376876658719866,-0.671483106788984,
-0.12));
#33955=CARTESIAN_POINT('Ctrl Pts',(0.407456234430149,-0.652083246520597,
-0.12));
#33956=CARTESIAN_POINT('Ctrl Pts',(0.436604118223066,-0.630593159063361,
-0.12));
#33957=CARTESIAN_POINT('Ctrl Pts',(0.464102331907716,-0.607172277822429,
-0.12));
#33958=CARTESIAN_POINT('Ctrl Pts',(0.491112633064527,-0.584166963261629,
-0.12));
#33959=CARTESIAN_POINT('Ctrl Pts',(0.516532076728422,-0.559297921849101,
-0.12));
#33960=CARTESIAN_POINT('Ctrl Pts',(0.540116340222347,-0.53268395928398,
-0.12));
#33961=CARTESIAN_POINT('Ctrl Pts',(0.545165350090399,-0.526986339782151,
-0.12));
#33962=CARTESIAN_POINT('Ctrl Pts',(0.550130085793828,-0.521208653508965,
-0.12));
#33963=CARTESIAN_POINT('Ctrl Pts',(0.555007866453731,-0.51535192480862,
-0.12));
#33964=CARTESIAN_POINT('',(-0.45977880844898,0.601851132366392,-1.12625));
#33965=CARTESIAN_POINT('Ctrl Pts',(-0.459817636075324,0.601890711574507,
-1.12625));
#33966=CARTESIAN_POINT('Ctrl Pts',(-0.432503985120159,0.625165263761499,
-1.12625));
#33967=CARTESIAN_POINT('Ctrl Pts',(-0.403593713496176,0.646405611026526,
-1.12625));
#33968=CARTESIAN_POINT('Ctrl Pts',(-0.373360039769516,0.665530294929992,
-1.12625));
#33969=CARTESIAN_POINT('Ctrl Pts',(-0.342830078355216,0.684842399271405,
-1.12625));
#33970=CARTESIAN_POINT('Ctrl Pts',(-0.31094965018966,0.701997871851396,
-1.12625));
#33971=CARTESIAN_POINT('Ctrl Pts',(-0.27796322910615,0.716874587570177,
-1.12625));
#33972=CARTESIAN_POINT('Ctrl Pts',(-0.26649732981665,0.722045652468616,
-1.12625));
#33973=CARTESIAN_POINT('Ctrl Pts',(-0.25489754895223,0.726941007906489,
-1.12625));
#33974=CARTESIAN_POINT('Ctrl Pts',(-0.243173471025965,0.731554211541679,
-1.12625));
#33975=CARTESIAN_POINT('Ctrl Pts',(-0.235772847933684,0.734466217207855,
-1.12625));
#33976=CARTESIAN_POINT('Ctrl Pts',(-0.228323386858712,0.737265362583718,
-1.12625));
#33977=CARTESIAN_POINT('Ctrl Pts',(-0.220840169235029,0.739945834207436,
-1.12625));
#33978=CARTESIAN_POINT('Ctrl Pts',(-0.196274161507377,0.748745322600449,
-1.12625));
#33979=CARTESIAN_POINT('Ctrl Pts',(-0.171310177389595,0.756280719951804,
-1.12625));
#33980=CARTESIAN_POINT('Ctrl Pts',(-0.146041756546094,0.762513765607056,
-1.12625));
#33981=CARTESIAN_POINT('Ctrl Pts',(-0.114363689392252,0.770327900097807,
-1.12625));
#33982=CARTESIAN_POINT('Ctrl Pts',(-0.0822071438969236,0.776096397271709,
-1.12625));
#33983=CARTESIAN_POINT('Ctrl Pts',(-0.0497689197316195,0.779842549380837,
-1.12625));
#33984=CARTESIAN_POINT('Ctrl Pts',(-0.0298100993333156,0.782147508393075,
-1.12625));
#33985=CARTESIAN_POINT('Ctrl Pts',(-0.00974437858918223,0.783686221448921,
-1.12625));
#33986=CARTESIAN_POINT('Ctrl Pts',(0.0103835877242539,0.784457979579485,
-1.12625));
#33987=CARTESIAN_POINT('Ctrl Pts',(0.0199668006279772,0.784825424673551,
-1.12625));
#33988=CARTESIAN_POINT('Ctrl Pts',(0.0295667334937316,0.785018756675132,
-1.12625));
#33989=CARTESIAN_POINT('Ctrl Pts',(0.0391548342290692,0.785038051041727,
-1.12625));
#33990=CARTESIAN_POINT('Ctrl Pts',(0.0764066796325684,0.785113013829603,
-1.12625));
#33991=CARTESIAN_POINT('Ctrl Pts',(0.113553048502875,0.78256936197534,-1.12625));
#33992=CARTESIAN_POINT('Ctrl Pts',(0.150309494086452,0.777450709617537,
-1.12625));
#33993=CARTESIAN_POINT('Ctrl Pts',(0.181105692019783,0.773162073198534,
-1.12625));
#33994=CARTESIAN_POINT('Ctrl Pts',(0.211628935935288,0.767064947824063,
-1.12625));
#33995=CARTESIAN_POINT('Ctrl Pts',(0.241714208481675,0.759156929049669,
-1.12625));
#33996=CARTESIAN_POINT('Ctrl Pts',(0.258311234815943,0.754794342815885,
-1.12625));
#33997=CARTESIAN_POINT('Ctrl Pts',(0.274774951161251,0.7498801751997,-1.12625));
#33998=CARTESIAN_POINT('Ctrl Pts',(0.291082790748263,0.744427662964886,
-1.12625));
#33999=CARTESIAN_POINT('Ctrl Pts',(0.302253486658688,0.740692750329893,
-1.12625));
#34000=CARTESIAN_POINT('Ctrl Pts',(0.313351031746933,0.736705191681684,
-1.12625));
#34001=CARTESIAN_POINT('Ctrl Pts',(0.324367932126046,0.732468638719791,
-1.12625));
#34002=CARTESIAN_POINT('Ctrl Pts',(0.331410788639504,0.729760305740867,
-1.12625));
#34003=CARTESIAN_POINT('Ctrl Pts',(0.338411390393548,0.726953771030822,
-1.12625));
#34004=CARTESIAN_POINT('Ctrl Pts',(0.345367277998784,0.72405101276316,-1.12625));
#34005=CARTESIAN_POINT('Ctrl Pts',(0.379999812823046,0.709598525532694,
-1.12625));
#34006=CARTESIAN_POINT('Ctrl Pts',(0.413530302275784,0.692762730520492,
-1.12625));
#34007=CARTESIAN_POINT('Ctrl Pts',(0.445738862386387,0.673721922806366,
-1.12625));
#34008=CARTESIAN_POINT('Ctrl Pts',(0.478055825617878,0.654617030172785,
-1.12625));
#34009=CARTESIAN_POINT('Ctrl Pts',(0.509043040539765,0.633291742439725,
-1.12625));
#34010=CARTESIAN_POINT('Ctrl Pts',(0.538461112130543,0.609877570946797,
-1.12625));
#34011=CARTESIAN_POINT('Ctrl Pts',(0.555983532412802,0.595931281089083,
-1.12625));
#34012=CARTESIAN_POINT('Ctrl Pts',(0.57294884620594,0.58124300692065,-1.12625));
#34013=CARTESIAN_POINT('Ctrl Pts',(0.589301091561376,0.565833523687251,
-1.12625));
#34014=CARTESIAN_POINT('Ctrl Pts',(-0.45981763607532,0.60189071157451,-1.12625));
#34015=CARTESIAN_POINT('Ctrl Pts',(-0.466706837362044,0.59663400030589,
-1.12600649737474));
#34016=CARTESIAN_POINT('Ctrl Pts',(-0.571995661495496,0.513358547689712,
-1.12223485618063));
#34017=CARTESIAN_POINT('Ctrl Pts',(-0.731074678445066,0.297631408040497,
-1.11493507641766));
#34018=CARTESIAN_POINT('Ctrl Pts',(-0.784486575071109,-0.0873109114175124,
-1.10435066071109));
#34019=CARTESIAN_POINT('Ctrl Pts',(-0.647739858405562,-0.451090008407746,
-1.09376624500451));
#34020=CARTESIAN_POINT('Ctrl Pts',(-0.353965525798943,-0.705517309450159,
-1.08318182929794));
#34021=CARTESIAN_POINT('Ctrl Pts',(0.0256119661671953,-0.788917676587972,
-1.07259741359137));
#34022=CARTESIAN_POINT('Ctrl Pts',(0.398982356900775,-0.68107280850569,
-1.0620129978848));
#34023=CARTESIAN_POINT('Ctrl Pts',(0.675632891112325,-0.408126282767527,
-1.05142858217823));
#34024=CARTESIAN_POINT('Ctrl Pts',(0.788500750688368,-0.036244024752235,
-1.04084416647166));
#34025=CARTESIAN_POINT('Ctrl Pts',(0.710224521156416,0.344424265850668,
-1.03025975076509));
#34026=CARTESIAN_POINT('Ctrl Pts',(0.459779801870052,0.641599200064964,
-1.01967533505852));
#34027=CARTESIAN_POINT('Ctrl Pts',(0.0978778173933265,0.783241287520997,
-1.00909091935195));
#34028=CARTESIAN_POINT('Ctrl Pts',(-0.287751124101883,0.735014472176636,
-0.998506503645377));
#34029=CARTESIAN_POINT('Ctrl Pts',(-0.603625085401646,0.508609617298404,
-0.987922087938806));
#34030=CARTESIAN_POINT('Ctrl Pts',(-0.773171671953705,0.158910506780705,
-0.977337672232235));
#34031=CARTESIAN_POINT('Ctrl Pts',(-0.755290373416536,-0.229310787602247,
-0.966753256525666));
#34032=CARTESIAN_POINT('Ctrl Pts',(-0.554315867123394,-0.561943861908008,
-0.956168840819094));
#34033=CARTESIAN_POINT('Ctrl Pts',(-0.218967255152568,-0.758353694545466,
-0.945584425112523));
#34034=CARTESIAN_POINT('Ctrl Pts',(0.169462156609871,-0.770927728297872,
-0.935000009405953));
#34035=CARTESIAN_POINT('Ctrl Pts',(0.516811513855877,-0.596617837396195,
-0.924415593699381));
#34036=CARTESIAN_POINT('Ctrl Pts',(0.738878357065634,-0.277679236275885,
-0.913831177992811));
#34037=CARTESIAN_POINT('Ctrl Pts',(0.781830502198585,0.108572789396221,
-0.90324676228624));
#34038=CARTESIAN_POINT('Ctrl Pts',(0.635255734092279,0.468505215644773,
-0.892662346579668));
#34039=CARTESIAN_POINT('Ctrl Pts',(0.334685876135463,0.714865266390365,
-0.882077930873099));
#34040=CARTESIAN_POINT('Ctrl Pts',(-0.0470166324849965,0.78793173628669,
-0.871493515166526));
#34041=CARTESIAN_POINT('Ctrl Pts',(-0.417321635893158,0.669992266368472,
-0.860909099459958));
#34042=CARTESIAN_POINT('Ctrl Pts',(-0.686461896723765,0.389637073600391,
-0.850324683753385));
#34043=CARTESIAN_POINT('Ctrl Pts',(-0.789193960383511,0.0148282727314076,
-0.839740268046816));
#34044=CARTESIAN_POINT('Ctrl Pts',(-0.700614103026784,-0.363575113859105,
-0.829155852340243));
#34045=CARTESIAN_POINT('Ctrl Pts',(-0.442195350963467,-0.653842684721737,
-0.818571436633674));
#34046=CARTESIAN_POINT('Ctrl Pts',(-0.0765821114814572,-0.785609422664233,
-0.807987020927103));
#34047=CARTESIAN_POINT('Ctrl Pts',(0.30759572884442,-0.726933182881659,
-0.797402605220531));
#34048=CARTESIAN_POINT('Ctrl Pts',(0.617207958261565,-0.492037926420709,
-0.786818189513962));
#34049=CARTESIAN_POINT('Ctrl Pts',(0.777200137236411,-0.137865628267143,
-0.776233773807389));
#34050=CARTESIAN_POINT('Ctrl Pts',(0.748787869734938,0.249727273071264,
-0.76564935810082));
#34051=CARTESIAN_POINT('Ctrl Pts',(0.538858696398576,0.576782706132405,
-0.755064942394247));
#34052=CARTESIAN_POINT('Ctrl Pts',(0.198302456030384,0.764017748949664,
-0.744480526687679));
#34053=CARTESIAN_POINT('Ctrl Pts',(-0.190325140315885,0.76604394504593,
-0.733896110981106));
#34054=CARTESIAN_POINT('Ctrl Pts',(-0.532815196286454,0.582370115462685,
-0.723311695274537));
#34055=CARTESIAN_POINT('Ctrl Pts',(-0.746143216224096,0.257521427575564,
-0.712727279567965));
#34056=CARTESIAN_POINT('Ctrl Pts',(-0.778595432221924,-0.129754143290103,
-0.702142863861395));
#34057=CARTESIAN_POINT('Ctrl Pts',(-0.622304962251661,-0.48557545112449,
-0.691558448154824));
#34058=CARTESIAN_POINT('Ctrl Pts',(-0.315158855058534,-0.723686313851511,
-0.680974032448253));
#34059=CARTESIAN_POINT('Ctrl Pts',(0.0683862731776844,-0.786365247463709,
-0.670389616741682));
#34060=CARTESIAN_POINT('Ctrl Pts',(0.435353589178261,-0.65841798059242,
-0.659805201035111));
#34061=CARTESIAN_POINT('Ctrl Pts',(0.696784958823666,-0.37086076354192,
-0.649220785328541));
#34062=CARTESIAN_POINT('Ctrl Pts',(0.789305673168616,0.00659841508485431,
-0.638636369621969));
#34063=CARTESIAN_POINT('Ctrl Pts',(0.690487385718299,0.382458043374308,
-0.628051953915399));
#34064=CARTESIAN_POINT('Ctrl Pts',(0.424285064899531,0.665604363327791,
-0.617467538208828));
#34065=CARTESIAN_POINT('Ctrl Pts',(0.0552299665647796,0.787398650983761,
-0.606883122502258));
#34066=CARTESIAN_POINT('Ctrl Pts',(-0.32721366682163,0.71831622633972,-0.596298706795686));
#34067=CARTESIAN_POINT('Ctrl Pts',(-0.630336020111219,0.475103658718963,
-0.585714291089116));
#34068=CARTESIAN_POINT('Ctrl Pts',(-0.780655892709756,0.116719158475916,
-0.575129875382544));
#34069=CARTESIAN_POINT('Ctrl Pts',(-0.74173359420234,-0.269959737756342,
-0.564545459675975));
#34070=CARTESIAN_POINT('Ctrl Pts',(-0.523004447299988,-0.591196526446348,
-0.553961043969403));
#34071=CARTESIAN_POINT('Ctrl Pts',(-0.177491530455713,-0.769118808373767,
-0.543376628262832));
#34072=CARTESIAN_POINT('Ctrl Pts',(0.211047875895698,-0.760595673704307,
-0.532792212556262));
#34073=CARTESIAN_POINT('Ctrl Pts',(0.548426253918519,-0.567693252373757,
-0.522207796849691));
#34074=CARTESIAN_POINT('Ctrl Pts',(0.752858251913652,-0.237173854594718,
-0.511623381143121));
#34075=CARTESIAN_POINT('Ctrl Pts',(0.774786625126501,0.150839882998086,
-0.501038965436549));
#34076=CARTESIAN_POINT('Ctrl Pts',(0.608895621771471,0.502287872206101,
-0.490454549729978));
#34077=CARTESIAN_POINT('Ctrl Pts',(0.295399597411619,0.731974086035049,
-0.479870134023408));
#34078=CARTESIAN_POINT('Ctrl Pts',(-0.0897055208909264,0.784219296051476,
-0.469285718316836));
#34079=CARTESIAN_POINT('Ctrl Pts',(-0.453064735918975,0.646358514947008,
-0.458701302610267));
#34080=CARTESIAN_POINT('Ctrl Pts',(-0.706594568913721,0.351811170884782,
-0.448116886903694));
#34081=CARTESIAN_POINT('Ctrl Pts',(-0.788835756602106,-0.0280202406126237,
-0.437532471197125));
#34082=CARTESIAN_POINT('Ctrl Pts',(-0.679851857001817,-0.401059144402229,
-0.426948055490553));
#34083=CARTESIAN_POINT('Ctrl Pts',(-0.40606212854654,-0.676875566510091,
-0.416363639783983));
#34084=CARTESIAN_POINT('Ctrl Pts',(-0.0338371233843339,-0.788607655212058,
-0.405779224077412));
#34085=CARTESIAN_POINT('Ctrl Pts',(0.346590485190772,-0.709169951669667,
-0.395194808370841));
#34086=CARTESIAN_POINT('Ctrl Pts',(0.642999595336511,-0.45781929315021,
-0.38461039266427));
#34087=CARTESIAN_POINT('Ctrl Pts',(0.783536392737088,-0.0954866798141,-0.374025976957699));
#34088=CARTESIAN_POINT('Ctrl Pts',(0.734132744595485,0.28999327252795,-0.363441561251129));
#34089=CARTESIAN_POINT('Ctrl Pts',(0.506764802819446,0.605174701533931,
-0.352857145544558));
#34090=CARTESIAN_POINT('Ctrl Pts',(0.156549813679539,0.773653113881336,
-0.342272729837987));
#34091=CARTESIAN_POINT('Ctrl Pts',(-0.231615093084909,0.754586929064556,
-0.331688314131416));
#34092=CARTESIAN_POINT('Ctrl Pts',(-0.563633182964224,0.552598063281501,
-0.321103898424845));
#34093=CARTESIAN_POINT('Ctrl Pts',(-0.759018516340419,0.216651511277543,
-0.310519482718275));
#34094=CARTESIAN_POINT('Ctrl Pts',(-0.770406886705711,-0.171814470849813,
-0.299935067011703));
#34095=CARTESIAN_POINT('Ctrl Pts',(-0.595037595541406,-0.51863016343718,
-0.289350651305133));
#34096=CARTESIAN_POINT('Ctrl Pts',(-0.275422660164455,-0.739722476337532,
-0.278766235598562));
#34097=CARTESIAN_POINT('Ctrl Pts',(0.110958659106209,-0.781495462293021,
-0.268181819891991));
#34098=CARTESIAN_POINT('Ctrl Pts',(0.470442038027584,-0.633822758023187,
-0.25759740418542));
#34099=CARTESIAN_POINT('Ctrl Pts',(0.715883472822076,-0.332502328862273,
-0.24701298847885));
#34100=CARTESIAN_POINT('Ctrl Pts',(0.787784607225334,0.0494214101901685,
-0.236428572772279));
#34101=CARTESIAN_POINT('Ctrl Pts',(0.668715255345631,0.419364726111373,
-0.225844157065708));
#34102=CARTESIAN_POINT('Ctrl Pts',(0.387540164029798,0.687647957073736,
-0.215259741359137));
#34103=CARTESIAN_POINT('Ctrl Pts',(0.0124189653017137,0.789235606485634,
-0.204675325652566));
#34104=CARTESIAN_POINT('Ctrl Pts',(-0.36571115764945,0.699500976810335,
-0.194090909945996));
#34105=CARTESIAN_POINT('Ctrl Pts',(-0.655190820886875,0.440197805626221,
-0.183506494239425));
#34106=CARTESIAN_POINT('Ctrl Pts',(-0.785836630350134,0.0741833682121673,
-0.172922078532854));
#34107=CARTESIAN_POINT('Ctrl Pts',(-0.725996588748235,-0.309812190918388,
-0.162337662826283));
#34108=CARTESIAN_POINT('Ctrl Pts',(-0.490140575868305,-0.618708756217194,
-0.151753247119712));
#34109=CARTESIAN_POINT('Ctrl Pts',(-0.135514917188149,-0.777613622822952,
-0.141168831413142));
#34110=CARTESIAN_POINT('Ctrl Pts',(0.252058240770721,-0.748030699511341,
-0.130584415706571));
#34111=CARTESIAN_POINT('Ctrl Pts',(0.469550542503074,-0.607385125337196,
-0.123528138568857));
#34112=CARTESIAN_POINT('Ctrl Pts',(0.555007866453731,-0.51535192480862,
-0.12));
#34113=CARTESIAN_POINT('Ctrl Pts',(-0.453782243834444,0.594001620520161,
-1.1425283350431));
#34114=CARTESIAN_POINT('Ctrl Pts',(-0.550881388338776,0.519823594492225,
-1.13905034750894));
#34115=CARTESIAN_POINT('Ctrl Pts',(-0.707932320584144,0.323031319671974,
-1.13209437244062));
#34116=CARTESIAN_POINT('Ctrl Pts',(-0.776614466270609,-0.0485165662670082,
-1.12166040983814));
#34117=CARTESIAN_POINT('Ctrl Pts',(-0.662248238305507,-0.408538693637011,
-1.11122644723566));
#34118=CARTESIAN_POINT('Ctrl Pts',(-0.391780881856493,-0.672308433025167,
-1.10079248463318));
#34119=CARTESIAN_POINT('Ctrl Pts',(-0.0289685614302378,-0.777586532369439,
-1.0903585220307));
#34120=CARTESIAN_POINT('Ctrl Pts',(0.34067266544482,-0.699591456600571,
-1.07992455942821));
#34121=CARTESIAN_POINT('Ctrl Pts',(0.630013764781801,-0.456690366635246,
-1.06949059682574));
#34122=CARTESIAN_POINT('Ctrl Pts',(0.770854889346008,-0.10614597677494,
-1.05905663422325));
#34123=CARTESIAN_POINT('Ctrl Pts',(0.729998172573568,0.269419497799131,
-1.04862267162077));
#34124=CARTESIAN_POINT('Ctrl Pts',(0.517074073818031,0.581479511865621,
-1.03818870901829));
#34125=CARTESIAN_POINT('Ctrl Pts',(0.182270729955255,0.756479721113076,
-1.02775474641581));
#34126=CARTESIAN_POINT('Ctrl Pts',(-0.195495525574094,0.753170354596226,
-1.01732078381333));
#34127=CARTESIAN_POINT('Ctrl Pts',(-0.527181654493517,0.572331754114923,
-1.00688682121085));
#34128=CARTESIAN_POINT('Ctrl Pts',(-0.734606108414347,0.256589128857389,
-0.99645285860837));
#34129=CARTESIAN_POINT('Ctrl Pts',(-0.768876998658737,-0.119633940618221,
-0.98601889600589));
#34130=CARTESIAN_POINT('Ctrl Pts',(-0.621916351700688,-0.467658178639457,
-0.975584933403408));
#34131=CARTESIAN_POINT('Ctrl Pts',(-0.328364174807739,-0.705450981188055,
-0.965150970800928));
#34132=CARTESIAN_POINT('Ctrl Pts',(0.0425865250681795,-0.776962359283856,
-0.954717008198448));
#34133=CARTESIAN_POINT('Ctrl Pts',(0.403499180542327,-0.665336403825431,
-0.944283045595967));
#34134=CARTESIAN_POINT('Ctrl Pts',(0.669303286159028,-0.39688440440999,
-0.933849082993487));
#34135=CARTESIAN_POINT('Ctrl Pts',(0.777346315469044,-0.0348830195569227,
-0.923415120391006));
#34136=CARTESIAN_POINT('Ctrl Pts',(0.702161510858137,0.335340620697416,
-0.912981157788526));
#34137=CARTESIAN_POINT('Ctrl Pts',(0.461470637519422,0.626521324425118,
-0.902547195186045));
#34138=CARTESIAN_POINT('Ctrl Pts',(0.112006796904714,0.770025062366403,
-0.892113232583564));
#34139=CARTESIAN_POINT('Ctrl Pts',(-0.263858098652974,0.732026654580471,
-0.881679269981083));
#34140=CARTESIAN_POINT('Ctrl Pts',(-0.577529159980994,0.521482682939162,
-0.871245307378604));
#34141=CARTESIAN_POINT('Ctrl Pts',(-0.75507116928701,0.188020340781936,
-0.860811344776122));
#34142=CARTESIAN_POINT('Ctrl Pts',(-0.754635806007903,-0.189760163171063,
-0.850377382173643));
#34143=CARTESIAN_POINT('Ctrl Pts',(-0.576325689361536,-0.522812412838008,
-0.83994341957116));
#34144=CARTESIAN_POINT('Ctrl Pts',(-0.262170190030731,-0.732632862145289,
-0.82950945696868));
#34145=CARTESIAN_POINT('Ctrl Pts',(0.113781287599418,-0.769764858789943,
-0.819075494366201));
#34146=CARTESIAN_POINT('Ctrl Pts',(0.462913446150841,-0.625456042107332,
-0.808641531763718));
#34147=CARTESIAN_POINT('Ctrl Pts',(0.702932553865032,-0.333721356752229,
-0.79820756916124));
#34148=CARTESIAN_POINT('Ctrl Pts',(0.77726385077405,0.0366745895092527,
-0.787773606558758));
#34149=CARTESIAN_POINT('Ctrl Pts',(0.668386751451239,0.398425990267,-0.777339643956278));
#34150=CARTESIAN_POINT('Ctrl Pts',(0.401964611697131,0.666264639748313,
-0.766905681353798));
#34151=CARTESIAN_POINT('Ctrl Pts',(0.040795634331005,0.777058450475451,
-0.756471718751315));
#34152=CARTESIAN_POINT('Ctrl Pts',(-0.329989257542916,0.704692279751986,
-0.746037756148836));
#34153=CARTESIAN_POINT('Ctrl Pts',(-0.622992579377319,0.46622351428963,
-0.735603793546354));
#34154=CARTESIAN_POINT('Ctrl Pts',(-0.769150693862395,0.117861483813719,
-0.725169830943875));
#34155=CARTESIAN_POINT('Ctrl Pts',(-0.734012759466783,-0.258281606344191,
-0.714735868341394));
#34156=CARTESIAN_POINT('Ctrl Pts',(-0.525861117638763,-0.573545293931951,
-0.704301905738913));
#34157=CARTESIAN_POINT('Ctrl Pts',(-0.193759067069451,-0.753618964174968,
-0.693867943136433));
#34158=CARTESIAN_POINT('Ctrl Pts',(0.184013817024176,-0.756057560229359,
-0.683433980533952));
#34159=CARTESIAN_POINT('Ctrl Pts',(0.518412914638575,-0.580286282081279,
-0.673000017931472));
#34160=CARTESIAN_POINT('Ctrl Pts',(0.73061721497504,-0.267736072313561,
-0.66256605532899));
#34161=CARTESIAN_POINT('Ctrl Pts',(0.770608169635336,0.107922046529211,
-0.652132092726511));
#34162=CARTESIAN_POINT('Ctrl Pts',(0.62895953467438,0.458141924492798,-0.64169813012403));
#34163=CARTESIAN_POINT('Ctrl Pts',(0.339059224908714,0.700373444128258,
-0.63126416752155));
#34164=CARTESIAN_POINT('Ctrl Pts',(-0.0307605314660666,0.777520359180197,
-0.620830204919068));
#34165=CARTESIAN_POINT('Ctrl Pts',(-0.393329741412471,0.671398416557692,
-0.610396242316588));
#34166=CARTESIAN_POINT('Ctrl Pts',(-0.663187433844332,0.407021555727391,
-0.599962279714107));
#34167=CARTESIAN_POINT('Ctrl Pts',(-0.7767256138806,0.0467058880397563,
-0.589528317111627));
#34168=CARTESIAN_POINT('Ctrl Pts',(-0.707182265180476,-0.324618796513675,
-0.579094354509146));
#34169=CARTESIAN_POINT('Ctrl Pts',(-0.470949408769067,-0.619427779176751,
-0.568660391906665));
#34170=CARTESIAN_POINT('Ctrl Pts',(-0.123709349589919,-0.768231811408391,
-0.558226429304186));
#34171=CARTESIAN_POINT('Ctrl Pts',(0.252690166207058,-0.735956383991622,
-0.547792466701704));
#34172=CARTESIAN_POINT('Ctrl Pts',(0.569528234436075,-0.530209118571064,
-0.537358504099224));
#34173=CARTESIAN_POINT('Ctrl Pts',(0.752123144005562,-0.199486579716444,
-0.526924541496743));
#34174=CARTESIAN_POINT('Ctrl Pts',(0.757435558261682,0.178256821234392,
-0.516490578894262));
#34175=CARTESIAN_POINT('Ctrl Pts',(0.58421329122536,0.513983413731816,-0.506056616291782));
#34176=CARTESIAN_POINT('Ctrl Pts',(0.273286459598611,0.728559283954182,
-0.495622653689301));
#34177=CARTESIAN_POINT('Ctrl Pts',(-0.102056559562226,0.77140688218741,
-0.485188691086821));
#34178=CARTESIAN_POINT('Ctrl Pts',(-0.453343888260034,0.63242662674262,
-0.47475472848434));
#34179=CARTESIAN_POINT('Ctrl Pts',(-0.697773800873293,0.344377470300547,
-0.46432076588186));
#34180=CARTESIAN_POINT('Ctrl Pts',(-0.777731869256008,-0.0248446931832595,
-0.453886803279379));
#34181=CARTESIAN_POINT('Ctrl Pts',(-0.674371225051026,-0.388210728933218,
-0.443452840676899));
#34182=CARTESIAN_POINT('Ctrl Pts',(-0.412054943730941,-0.660071846530996,
-0.433018878074418));
#34183=CARTESIAN_POINT('Ctrl Pts',(-0.0526134386847218,-0.776347824950465,
-0.422584915471937));
#34184=CARTESIAN_POINT('Ctrl Pts',(0.319229548446936,-0.709631323036316,
-0.412150952869456));
#34185=CARTESIAN_POINT('Ctrl Pts',(0.615827130120359,-0.475648047450979,
-0.401716990266976));
#34186=CARTESIAN_POINT('Ctrl Pts',(0.767268468189365,-0.129550055793601,
-0.391283027664495));
#34187=CARTESIAN_POINT('Ctrl Pts',(0.737857415668762,0.24708410184319,-0.380849065062015));
#34188=CARTESIAN_POINT('Ctrl Pts',(0.534526434095284,0.565478213973463,
-0.370415102459534));
#34189=CARTESIAN_POINT('Ctrl Pts',(0.205202547258304,0.750583795355781,
-0.359981139857054));
#34190=CARTESIAN_POINT('Ctrl Pts',(-0.172489509004567,0.758769720339229,
-0.349547177254573));
#34191=CARTESIAN_POINT('Ctrl Pts',(-0.509524166428113,0.588106489551379,
-0.339113214652093));
#34192=CARTESIAN_POINT('Ctrl Pts',(-0.726459188269098,0.278821030603052,
-0.328679252049611));
#34193=CARTESIAN_POINT('Ctrl Pts',(-0.772160950053184,-0.0961851660426477,
-0.318245289447131));
#34194=CARTESIAN_POINT('Ctrl Pts',(-0.635857117988058,-0.448519615362849,
-0.307811326844651));
#34195=CARTESIAN_POINT('Ctrl Pts',(-0.349675784487423,-0.695133774103561,
-0.29737736424217));
#34196=CARTESIAN_POINT('Ctrl Pts',(0.0189274157531888,-0.777898369643474,
-0.28694340163969));
#34197=CARTESIAN_POINT('Ctrl Pts',(0.383069251609914,-0.67730500314506,
-0.276509439037209));
#34198=CARTESIAN_POINT('Ctrl Pts',(0.656918053157321,-0.417064487823481,
-0.266075476434728));
#34199=CARTESIAN_POINT('Ctrl Pts',(0.775925115315038,-0.0585179376441977,
-0.255641513832248));
#34200=CARTESIAN_POINT('Ctrl Pts',(0.712039292365909,0.313821812003488,
-0.245207551229767));
#34201=CARTESIAN_POINT('Ctrl Pts',(0.480319196218496,0.612190866640263,
-0.234773588627287));
#34202=CARTESIAN_POINT('Ctrl Pts',(0.135383189993241,0.766260668703223,
-0.224339626024806));
#34203=CARTESIAN_POINT('Ctrl Pts',(-0.241463591288354,0.739715845333339,
-0.213905663422325));
#34204=CARTESIAN_POINT('Ctrl Pts',(-0.561395755032469,0.5388126158932,-0.203471700819845));
#34205=CARTESIAN_POINT('Ctrl Pts',(-0.749000440414916,0.210907029399775,
-0.193037738217364));
#34206=CARTESIAN_POINT('Ctrl Pts',(-0.76006108477016,-0.166712982541228,
-0.182603775614884));
#34207=CARTESIAN_POINT('Ctrl Pts',(-0.591963456523644,-0.505033918677001,
-0.172169813012403));
#34208=CARTESIAN_POINT('Ctrl Pts',(-0.284343786563683,-0.724320025643106,
-0.161735850409922));
#34209=CARTESIAN_POINT('Ctrl Pts',(0.09031673140191,-0.772864465068915,
-0.151301887807442));
#34210=CARTESIAN_POINT('Ctrl Pts',(0.44365235923649,-0.639262442637623,
-0.140867925204961));
#34211=CARTESIAN_POINT('Ctrl Pts',(0.692489824641788,-0.354929918130683,
-0.13043396260248));
#34212=CARTESIAN_POINT('Ctrl Pts',(0.749438361810141,-0.109676867461678,
-0.12347798753416));
#34213=CARTESIAN_POINT('Ctrl Pts',(0.747395528060274,0.012496985056547,
-0.12));
#34214=CARTESIAN_POINT('Ctrl Pts',(-0.453782243834444,0.594001620520161,
-1.13966850381659));
#34215=CARTESIAN_POINT('Ctrl Pts',(-0.550881059946454,0.519823845364613,
-1.13619051628243));
#34216=CARTESIAN_POINT('Ctrl Pts',(-0.707932492103511,0.323031139564096,
-1.12923454121411));
#34217=CARTESIAN_POINT('Ctrl Pts',(-0.776614348027596,-0.0485164852858574,
-1.11880057861163));
#34218=CARTESIAN_POINT('Ctrl Pts',(-0.662248261705559,-0.40853871944569,
-1.10836661600915));
#34219=CARTESIAN_POINT('Ctrl Pts',(-0.391780845205783,-0.67230838997676,
-1.09793265340667));
#34220=CARTESIAN_POINT('Ctrl Pts',(-0.0289685722792028,-0.777586516102956,
-1.08749869080419));
#34221=CARTESIAN_POINT('Ctrl Pts',(0.340672659850851,-0.699591427563088,
-1.07706472820171));
#34222=CARTESIAN_POINT('Ctrl Pts',(0.630013740257188,-0.456690353715162,
-1.06663076559923));
#34223=CARTESIAN_POINT('Ctrl Pts',(0.770854864632094,-0.106145971815373,
-1.05619680299675));
#34224=CARTESIAN_POINT('Ctrl Pts',(0.72999814690911,0.269419487936225,-1.04576284039427));
#34225=CARTESIAN_POINT('Ctrl Pts',(0.517074056599653,0.581479492398165,
-1.03532887779179));
#34226=CARTESIAN_POINT('Ctrl Pts',(0.182270723540412,0.75647969515944,-1.02489491518931));
#34227=CARTESIAN_POINT('Ctrl Pts',(-0.195495518808877,0.753170329021126,
-1.01446095258683));
#34228=CARTESIAN_POINT('Ctrl Pts',(-0.527181636582195,0.572331734566925,
-1.00402698998434));
#34229=CARTESIAN_POINT('Ctrl Pts',(-0.734606083355523,0.256589120137115,
-0.993593027381866));
#34230=CARTESIAN_POINT('Ctrl Pts',(-0.768876972472471,-0.119633936553389,
-0.983159064779384));
#34231=CARTESIAN_POINT('Ctrl Pts',(-0.62191633050167,-0.467658162697799,
-0.972725102176903));
#34232=CARTESIAN_POINT('Ctrl Pts',(-0.328364163622079,-0.705450957152499,
-0.962291139574423));
#34233=CARTESIAN_POINT('Ctrl Pts',(0.0425865236188069,-0.776962332806937,
-0.951857176971942));
#34234=CARTESIAN_POINT('Ctrl Pts',(0.403499166791987,-0.665336381154547,
-0.941423214369462));
#34235=CARTESIAN_POINT('Ctrl Pts',(0.669303263352647,-0.396884390885559,
-0.930989251766981));
#34236=CARTESIAN_POINT('Ctrl Pts',(0.777346288980351,-0.0348830183684687,
-0.920555289164501));
#34237=CARTESIAN_POINT('Ctrl Pts',(0.702161486931755,0.335340609270621,
-0.910121326562019));
#34238=CARTESIAN_POINT('Ctrl Pts',(0.461470621794522,0.626521303076042,
-0.89968736395954));
#34239=CARTESIAN_POINT('Ctrl Pts',(0.112006793088058,0.770025036127444,
-0.889253401357058));
#34240=CARTESIAN_POINT('Ctrl Pts',(-0.263858089661894,0.732026629636288,
-0.878819438754579));
#34241=CARTESIAN_POINT('Ctrl Pts',(-0.577529140301394,0.521482665169388,
-0.868385476152096));
#34242=CARTESIAN_POINT('Ctrl Pts',(-0.75507114355759,0.188020334375047,
-0.857951513549617));
#34243=CARTESIAN_POINT('Ctrl Pts',(-0.754635780293312,-0.189760156704889,
-0.847517550947136));
#34244=CARTESIAN_POINT('Ctrl Pts',(-0.576325669722955,-0.522812395022917,
-0.837083588344655));
#34245=CARTESIAN_POINT('Ctrl Pts',(-0.262170181097151,-0.732632837180461,
-0.826649625742175));
#34246=CARTESIAN_POINT('Ctrl Pts',(0.113781283722264,-0.769764832559825,
-0.816215663139694));
#34247=CARTESIAN_POINT('Ctrl Pts',(0.462913430376836,-0.625456020794608,
-0.805781700537214));
#34248=CARTESIAN_POINT('Ctrl Pts',(0.702932529912257,-0.333721345380509,
-0.795347737934733));
#34249=CARTESIAN_POINT('Ctrl Pts',(0.7772638242884,0.0366745882595479,-0.784913775332253));
#34250=CARTESIAN_POINT('Ctrl Pts',(0.668386728675629,0.398425976690438,
-0.774479812729771));
#34251=CARTESIAN_POINT('Ctrl Pts',(0.401964597999989,0.666264617045014,
-0.764045850127292));
#34252=CARTESIAN_POINT('Ctrl Pts',(0.0407956329408734,0.777058423996801,
-0.75361188752481));
#34253=CARTESIAN_POINT('Ctrl Pts',(-0.329989246298369,0.704692255739247,
-0.74317792492233));
#34254=CARTESIAN_POINT('Ctrl Pts',(-0.622992558148538,0.466223498402834,
-0.732743962319849));
#34255=CARTESIAN_POINT('Ctrl Pts',(-0.769150667653204,0.11786147979753,
-0.722309999717369));
#34256=CARTESIAN_POINT('Ctrl Pts',(-0.734012734454935,-0.258281597543118,
-0.711876037114888));
#34257=CARTESIAN_POINT('Ctrl Pts',(-0.525861099719785,-0.573545274388111,
-0.701442074512408));
#34258=CARTESIAN_POINT('Ctrl Pts',(-0.193759060467015,-0.75361893849503,
-0.691008111909926));
#34259=CARTESIAN_POINT('Ctrl Pts',(0.184013810753814,-0.756057534466323,
-0.680574149307447));
#34260=CARTESIAN_POINT('Ctrl Pts',(0.518412896973398,-0.580286262307737,
-0.670140186704965));
#34261=CARTESIAN_POINT('Ctrl Pts',(0.730617190078897,-0.267736063190322,
-0.659706224102486));
#34262=CARTESIAN_POINT('Ctrl Pts',(0.770608143376481,0.107922042851714,
-0.649272261500004));
#34263=CARTESIAN_POINT('Ctrl Pts',(0.628959513242272,0.458141908881385,
-0.638838298897525));
#34264=CARTESIAN_POINT('Ctrl Pts',(0.339059213355103,0.700373420262687,
-0.628404336295043));
#34265=CARTESIAN_POINT('Ctrl Pts',(-0.0307605304178867,0.777520332685805,
-0.617970373692563));
#34266=CARTESIAN_POINT('Ctrl Pts',(-0.393329728009565,0.671398393679458,
-0.607536411090083));
#34267=CARTESIAN_POINT('Ctrl Pts',(-0.663187411245893,0.40702154185793,
-0.597102448487601));
#34268=CARTESIAN_POINT('Ctrl Pts',(-0.77672558741329,0.0467058864482299,
-0.586668485885122));
#34269=CARTESIAN_POINT('Ctrl Pts',(-0.707182241082891,-0.324618785452129,
-0.57623452328264));
#34270=CARTESIAN_POINT('Ctrl Pts',(-0.470949392721232,-0.619427758069444,
-0.56580056068016));
#34271=CARTESIAN_POINT('Ctrl Pts',(-0.123709345374462,-0.768231785230512,
-0.555366598077679));
#34272=CARTESIAN_POINT('Ctrl Pts',(0.252690157596516,-0.735956358913545,
-0.544932635475199));
#34273=CARTESIAN_POINT('Ctrl Pts',(0.569528215029119,-0.530209100503926,
-0.534498672872717));
#34274=CARTESIAN_POINT('Ctrl Pts',(0.752123118376594,-0.19948657291884,
-0.524064710270238));
#34275=CARTESIAN_POINT('Ctrl Pts',(0.757435532451691,0.178256815160203,
-0.513630747667757));
#34276=CARTESIAN_POINT('Ctrl Pts',(0.584213271318003,0.513983396217577,
-0.503196785065276));
#34277=CARTESIAN_POINT('Ctrl Pts',(0.27328645028624,0.728559259128164,-0.492762822462796));
#34278=CARTESIAN_POINT('Ctrl Pts',(-0.102056556084598,0.771406855901339,
-0.482328859860315));
#34279=CARTESIAN_POINT('Ctrl Pts',(-0.453343872812117,0.63242660519237,
-0.471894897257835));
#34280=CARTESIAN_POINT('Ctrl Pts',(-0.697773777096305,0.344377458565714,
-0.461460934655354));
#34281=CARTESIAN_POINT('Ctrl Pts',(-0.77773184275441,-0.0248446923366639,
-0.451026972052874));
#34282=CARTESIAN_POINT('Ctrl Pts',(-0.674371202071493,-0.388210715704746,
-0.440593009450393));
#34283=CARTESIAN_POINT('Ctrl Pts',(-0.412054929689965,-0.66007182403872,
-0.430159046847912));
#34284=CARTESIAN_POINT('Ctrl Pts',(-0.0526134368918924,-0.776347798496031,
-0.419725084245431));
#34285=CARTESIAN_POINT('Ctrl Pts',(0.31922953756903,-0.709631298855274,
-0.409291121642952));
#34286=CARTESIAN_POINT('Ctrl Pts',(0.615827109135746,-0.475648031243042,
-0.39885715904047));
#34287=CARTESIAN_POINT('Ctrl Pts',(0.767268442044312,-0.129550051379108,
-0.38842319643799));
#34288=CARTESIAN_POINT('Ctrl Pts',(0.737857390525905,0.247084093423657,
-0.377989233835509));
#34289=CARTESIAN_POINT('Ctrl Pts',(0.534526415881033,0.565478194704553,
-0.367555271233028));
#34290=CARTESIAN_POINT('Ctrl Pts',(0.205202540265923,0.750583769779188,
-0.357121308630548));
#34291=CARTESIAN_POINT('Ctrl Pts',(-0.172489503126895,0.758769694483932,
-0.346687346028067));
#34292=CARTESIAN_POINT('Ctrl Pts',(-0.509524149065839,0.58810646951105,
-0.336253383425587));
#34293=CARTESIAN_POINT('Ctrl Pts',(-0.726459163514615,0.278821021102697,
-0.325819420823106));
#34294=CARTESIAN_POINT('Ctrl Pts',(-0.772160923741469,-0.0961851627662888,
-0.315385458220626));
#34295=CARTESIAN_POINT('Ctrl Pts',(-0.63585709632081,-0.448519600076963,
-0.304951495618145));
#34296=CARTESIAN_POINT('Ctrl Pts',(-0.34967577257225,-0.695133750421173,
-0.294517533015665));
#34297=CARTESIAN_POINT('Ctrl Pts',(0.0189274151086266,-0.777898343127075,
-0.284083570413184));
#34298=CARTESIAN_POINT('Ctrl Pts',(0.383069238555855,-0.677304980083515,
-0.273649607810703));
#34299=CARTESIAN_POINT('Ctrl Pts',(0.656918030774058,-0.417064473576466,
-0.263215645208223));
#34300=CARTESIAN_POINT('Ctrl Pts',(0.775925088871968,-0.0585179357197007,
-0.252781682605742));
#34301=CARTESIAN_POINT('Ctrl Pts',(0.712039268108796,0.313821801446672,
-0.242347720003262));
#34302=CARTESIAN_POINT('Ctrl Pts',(0.480319179839619,0.612190845510335,
-0.23191375740078));
#34303=CARTESIAN_POINT('Ctrl Pts',(0.135383185403138,0.766260643122266,
-0.2214797947983));
#34304=CARTESIAN_POINT('Ctrl Pts',(-0.241463583105909,0.73971581908474,
-0.21104583219582));
#34305=CARTESIAN_POINT('Ctrl Pts',(-0.561395735813007,0.538812599584091,
-0.200611869593339));
#34306=CARTESIAN_POINT('Ctrl Pts',(-0.749000415068712,0.210907018176796,
-0.190177906990859));
#34307=CARTESIAN_POINT('Ctrl Pts',(-0.760061058523674,-0.166712968918093,
-0.179743944388378));
#34308=CARTESIAN_POINT('Ctrl Pts',(-0.59196343703511,-0.505033917097267,
-0.169309981785897));
#34309=CARTESIAN_POINT('Ctrl Pts',(-0.284343775530136,-0.724319970193124,
-0.158876019183416));
#34310=CARTESIAN_POINT('Ctrl Pts',(0.0903167256720993,-0.772864499431969,
-0.148442056580936));
#34311=CARTESIAN_POINT('Ctrl Pts',(0.443652349415121,-0.639262299658962,
-0.138008093978455));
#34312=CARTESIAN_POINT('Ctrl Pts',(0.69248978975463,-0.354930164383859,
-0.127574131375975));
#34313=CARTESIAN_POINT('Ctrl Pts',(0.749438354901214,-0.109676454265914,
-0.120618156307654));
#34314=CARTESIAN_POINT('Ctrl Pts',(0.747395528060274,0.012496985056547,
-0.117140168773494));
#34315=CARTESIAN_POINT('Ctrl Pts',(-0.454743647135464,0.59526009884658,
-1.13299148312149));
#34316=CARTESIAN_POINT('Ctrl Pts',(-0.552049078435987,0.520924481859268,
-1.12951349558733));
#34317=CARTESIAN_POINT('Ctrl Pts',(-0.709431880792854,0.323716019874443,
-1.12255752051901));
#34318=CARTESIAN_POINT('Ctrl Pts',(-0.778260040912912,-0.048619495750048,
-1.11212355791653));
#34319=CARTESIAN_POINT('Ctrl Pts',(-0.663651266471094,-0.409404197277858,
-1.10168959531405));
#34320=CARTESIAN_POINT('Ctrl Pts',(-0.392610989723487,-0.673732890143879,
-1.09125563271157));
#34321=CARTESIAN_POINT('Ctrl Pts',(-0.0290299167445311,-0.779233990024141,
-1.08082167010908));
#34322=CARTESIAN_POINT('Ctrl Pts',(0.341394439427495,-0.701073692506756,
-1.0703877075066));
#34323=CARTESIAN_POINT('Ctrl Pts',(0.631348582478227,-0.457657953570587,
-1.05995374490412));
#34324=CARTESIAN_POINT('Ctrl Pts',(0.772488099658164,-0.106370870957121,
-1.04951978230164));
#34325=CARTESIAN_POINT('Ctrl Pts',(0.731544823668042,0.269990319029405,
-1.03908581969916));
#34326=CARTESIAN_POINT('Ctrl Pts',(0.51816959980594,0.582711493978724,-1.02865185709668));
#34327=CARTESIAN_POINT('Ctrl Pts',(0.182656907952848,0.758082477697759,
-1.0182178944942));
#34328=CARTESIAN_POINT('Ctrl Pts',(-0.19590972281978,0.754766099154424,
-1.00778393189172));
#34329=CARTESIAN_POINT('Ctrl Pts',(-0.528298596051656,0.573544355519815,
-0.997349969289239));
#34330=CARTESIAN_POINT('Ctrl Pts',(-0.736162521039286,0.257132765118676,
-0.98691600668676));
#34331=CARTESIAN_POINT('Ctrl Pts',(-0.77050602107108,-0.119887409454019,
-0.976482044084279));
#34332=CARTESIAN_POINT('Ctrl Pts',(-0.623234008102322,-0.46864900769872,
-0.966048081481798));
#34333=CARTESIAN_POINT('Ctrl Pts',(-0.329059881148492,-0.706945622689532,
-0.955614118879318));
#34334=CARTESIAN_POINT('Ctrl Pts',(0.0426767532874504,-0.778608512204756,
-0.945180156276837));
#34335=CARTESIAN_POINT('Ctrl Pts',(0.404354075695015,-0.666746054432853,
-0.934746193674357));
#34336=CARTESIAN_POINT('Ctrl Pts',(0.670721341414739,-0.397725284812044,
-0.924312231071876));
#34337=CARTESIAN_POINT('Ctrl Pts',(0.778993281877019,-0.0349569263343644,
-0.913878268469395));
#34338=CARTESIAN_POINT('Ctrl Pts',(0.703649182952154,0.336051108064826,
-0.903444305866915));
#34339=CARTESIAN_POINT('Ctrl Pts',(0.462448357003043,0.627848737386999,
-0.893010343264434));
#34340=CARTESIAN_POINT('Ctrl Pts',(0.112244106104242,0.771656517208898,
-0.882576380661952));
#34341=CARTESIAN_POINT('Ctrl Pts',(-0.264417135746451,0.733577602061106,
-0.872142418059474));
#34342=CARTESIAN_POINT('Ctrl Pts',(-0.578752773069475,0.522587550157066,
-0.861708455456991));
#34343=CARTESIAN_POINT('Ctrl Pts',(-0.756670941263009,0.188418700147704,
-0.851274492854512));
#34344=CARTESIAN_POINT('Ctrl Pts',(-0.756234655578182,-0.19016220870472,
-0.840840530252031));
#34345=CARTESIAN_POINT('Ctrl Pts',(-0.577546752652513,-0.523920097359396,
-0.83040656764955));
#34346=CARTESIAN_POINT('Ctrl Pts',(-0.262725650946226,-0.734185094000027,
-0.81997260504707));
#34347=CARTESIAN_POINT('Ctrl Pts',(0.114022356418756,-0.771395762338239,
-0.809538642444589));
#34348=CARTESIAN_POINT('Ctrl Pts',(0.463894222518143,-0.626781198051682,
-0.799104679842109));
#34349=CARTESIAN_POINT('Ctrl Pts',(0.70442185957082,-0.334428413379528,
-0.788670717239628));
#34350=CARTESIAN_POINT('Ctrl Pts',(0.778910642463376,0.0367522920926843,
-0.778236754637148));
#34351=CARTESIAN_POINT('Ctrl Pts',(0.669802864842397,0.399270136831811,
-0.767802792034666));
#34352=CARTESIAN_POINT('Ctrl Pts',(0.402816255551772,0.667676257013847,
-0.757368829432186));
#34353=CARTESIAN_POINT('Ctrl Pts',(0.0408820681867802,0.778704806982432,
-0.746934866829706));
#34354=CARTESIAN_POINT('Ctrl Pts',(-0.330688406958327,0.706185313795279,
-0.736500904227224));
#34355=CARTESIAN_POINT('Ctrl Pts',(-0.624312515974406,0.46721130371009,
-0.726066941624745));
#34356=CARTESIAN_POINT('Ctrl Pts',(-0.770780296177272,0.118111197359309,
-0.715632979022264));
#34357=CARTESIAN_POINT('Ctrl Pts',(-0.73556791491489,-0.258828828503577,
-0.705199016419783));
#34358=CARTESIAN_POINT('Ctrl Pts',(-0.526975261461873,-0.574760466389229,
-0.694765053817303));
#34359=CARTESIAN_POINT('Ctrl Pts',(-0.19416958509504,-0.755215659358831,
-0.684331091214822));
#34360=CARTESIAN_POINT('Ctrl Pts',(0.18440368775378,-0.757659422075367,
-0.673897128612342));
#34361=CARTESIAN_POINT('Ctrl Pts',(0.519511277927458,-0.581515736694162,
-0.663463166009861));
#34362=CARTESIAN_POINT('Ctrl Pts',(0.732165176270937,-0.268303325683674,
-0.65302920340738));
#34363=CARTESIAN_POINT('Ctrl Pts',(0.772240859909325,0.108150701353621,
-0.6425952408049));
#34364=CARTESIAN_POINT('Ctrl Pts',(0.63029211348091,0.459112591420168,-0.632161278202419));
#34365=CARTESIAN_POINT('Ctrl Pts',(0.339777590896291,0.701857327839131,
-0.621727315599939));
#34366=CARTESIAN_POINT('Ctrl Pts',(-0.0308257039136559,0.779167694334796,
-0.611293352997458));
#34367=CARTESIAN_POINT('Ctrl Pts',(-0.394163090536681,0.672820910774439,
-0.600859390394977));
#34368=CARTESIAN_POINT('Ctrl Pts',(-0.664592531422757,0.407883913747361,
-0.590425427792497));
#34369=CARTESIAN_POINT('Ctrl Pts',(-0.778371265205501,0.0468048439711169,
-0.579991465190016));
#34370=CARTESIAN_POINT('Ctrl Pts',(-0.708680574764767,-0.325306567514172,
-0.569557502587535));
#34371=CARTESIAN_POINT('Ctrl Pts',(-0.471947210958994,-0.620740163018957,
-0.559123539985055));
#34372=CARTESIAN_POINT('Ctrl Pts',(-0.12397145302956,-0.769859466883738,
-0.548689577382575));
#34373=CARTESIAN_POINT('Ctrl Pts',(0.253225541762308,-0.737515657403935,
-0.538255614780094));
#34374=CARTESIAN_POINT('Ctrl Pts',(0.570734895935091,-0.531332474519237,
-0.527821652177613));
#34375=CARTESIAN_POINT('Ctrl Pts',(0.753716669989902,-0.199909232643481,
-0.517387689575133));
#34376=CARTESIAN_POINT('Ctrl Pts',(0.759040339677031,0.17863449459651,-0.506953726972652));
#34377=CARTESIAN_POINT('Ctrl Pts',(0.585451066006505,0.515072392221348,
-0.496519764370171));
#34378=CARTESIAN_POINT('Ctrl Pts',(0.273865472594036,0.730102885104296,
-0.486085801767691));
#34379=CARTESIAN_POINT('Ctrl Pts',(-0.102272787158506,0.773041264696527,
-0.47565183916521));
#34380=CARTESIAN_POINT('Ctrl Pts',(-0.454304389570946,0.633766551289466,
-0.465217876562729));
#34381=CARTESIAN_POINT('Ctrl Pts',(-0.699252176710741,0.345107104073579,
-0.454783913960249));
#34382=CARTESIAN_POINT('Ctrl Pts',(-0.779379652537759,-0.0248973317232062,
-0.444349951357768));
#34383=CARTESIAN_POINT('Ctrl Pts',(-0.675800017767717,-0.389033232387453,
-0.433915988755288));
#34384=CARTESIAN_POINT('Ctrl Pts',(-0.412927966008004,-0.661470343103483,
-0.423482026152808));
#34385=CARTESIAN_POINT('Ctrl Pts',(-0.0527249109646764,-0.777992675852612,
-0.413048063550326));
#34386=CARTESIAN_POINT('Ctrl Pts',(0.319905901228356,-0.711134821448214,
-0.402614100947846));
#34387=CARTESIAN_POINT('Ctrl Pts',(0.617131885254584,-0.476655804663409,
-0.392180138345365));
#34388=CARTESIAN_POINT('Ctrl Pts',(0.768894082626002,-0.129824533958299,
-0.381746175742884));
#34389=CARTESIAN_POINT('Ctrl Pts',(0.739420716803662,0.247607599809939,
-0.371312213140404));
#34390=CARTESIAN_POINT('Ctrl Pts',(0.535658937155234,0.566676294679626,
-0.360878250537923));
#34391=CARTESIAN_POINT('Ctrl Pts',(0.205637310626139,0.752174059916794,
-0.350444287935443));
#34392=CARTESIAN_POINT('Ctrl Pts',(-0.172854963141732,0.760377328448251,
-0.340010325332963));
#34393=CARTESIAN_POINT('Ctrl Pts',(-0.510603697094476,0.58935251286622,
-0.329576362730482));
#34394=CARTESIAN_POINT('Ctrl Pts',(-0.727998339939048,0.279411769712726,
-0.319142400128001));
#34395=CARTESIAN_POINT('Ctrl Pts',(-0.773796930208484,-0.0963889538944908,
-0.308708437525521));
#34396=CARTESIAN_POINT('Ctrl Pts',(-0.637204310729103,-0.449469895473667,
-0.29827447492304));
#34397=CARTESIAN_POINT('Ctrl Pts',(-0.350416643817245,-0.696606556498865,
-0.287840512320559));
#34398=CARTESIAN_POINT('Ctrl Pts',(0.0189675173356764,-0.779546505705979,
-0.277406549718079));
#34399=CARTESIAN_POINT('Ctrl Pts',(0.383880861799188,-0.678740011636779,
-0.266972587115598));
#34400=CARTESIAN_POINT('Ctrl Pts',(0.65830986777388,-0.417948123900598,
-0.256538624513118));
#34401=CARTESIAN_POINT('Ctrl Pts',(0.777569070626036,-0.0586419196868223,
-0.246104661910636));
#34402=CARTESIAN_POINT('Ctrl Pts',(0.713547892540654,0.314486707157708,
-0.235670699308157));
#34403=CARTESIAN_POINT('Ctrl Pts',(0.481336850230822,0.613487918075931,
-0.225236736705676));
#34404=CARTESIAN_POINT('Ctrl Pts',(0.135670026800076,0.767884146994865,
-0.214802774103195));
#34405=CARTESIAN_POINT('Ctrl Pts',(-0.241975180980523,0.741283085733481,
-0.204368811500715));
#34406=CARTESIAN_POINT('Ctrl Pts',(-0.562585186373481,0.539954196552607,
-0.193934848898234));
#34407=CARTESIAN_POINT('Ctrl Pts',(-0.750587350010884,0.211353885858112,
-0.183500886295754));
#34408=CARTESIAN_POINT('Ctrl Pts',(-0.76167142949834,-0.167066211673776,
-0.173066923693273));
#34409=CARTESIAN_POINT('Ctrl Pts',(-0.593217650425967,-0.506103908795648,
-0.162632961090792));
#34410=CARTESIAN_POINT('Ctrl Pts',(-0.284946229083341,-0.725854698300192,
-0.152198998488312));
#34411=CARTESIAN_POINT('Ctrl Pts',(0.090508090371596,-0.77450183073683,
-0.141765035885831));
#34412=CARTESIAN_POINT('Ctrl Pts',(0.44459231790613,-0.640617059956736,
-0.131331073283351));
#34413=CARTESIAN_POINT('Ctrl Pts',(0.693957024835472,-0.355681462393161,
-0.12089711068087));
#34414=CARTESIAN_POINT('Ctrl Pts',(0.751026167303854,-0.109909948718274,
-0.113941135612549));
#34415=CARTESIAN_POINT('Ctrl Pts',(0.748978993560761,0.0125234617264684,
-0.110463148078389));
#34416=CARTESIAN_POINT('Ctrl Pts',(-0.457725546467602,0.599163409431303,
-1.12801069747057));
#34417=CARTESIAN_POINT('Ctrl Pts',(-0.555667179198619,0.524341772031441,
-1.12453270993641));
#34418=CARTESIAN_POINT('Ctrl Pts',(-0.714084824405276,0.325837708337132,
-1.11757673486809));
#34419=CARTESIAN_POINT('Ctrl Pts',(-0.783362670351873,-0.0489378503027571,
-1.1071427722656));
#34420=CARTESIAN_POINT('Ctrl Pts',(-0.66800317241879,-0.412088937642738,
-1.09670880966313));
#34421=CARTESIAN_POINT('Ctrl Pts',(-0.395185257636931,-0.678150527881453,
-1.08627484706064));
#34422=CARTESIAN_POINT('Ctrl Pts',(-0.0292203366733291,-0.784343583971594,
-1.07584088445816));
#34423=CARTESIAN_POINT('Ctrl Pts',(0.343633040095596,-0.705670692032948,
-1.06540692185568));
#34424=CARTESIAN_POINT('Ctrl Pts',(0.635488397768257,-0.460658889708478,
-1.0549729592532));
#34425=CARTESIAN_POINT('Ctrl Pts',(0.777553410767088,-0.10706835061983,
-1.04453899665072));
#34426=CARTESIAN_POINT('Ctrl Pts',(0.736341651251883,0.271760675877957,
-1.03410503404824));
#34427=CARTESIAN_POINT('Ctrl Pts',(0.521567305771499,0.586532409010022,
-1.02367107144576));
#34428=CARTESIAN_POINT('Ctrl Pts',(0.18385461127603,0.763053319515688,-1.01323710884328));
#34429=CARTESIAN_POINT('Ctrl Pts',(-0.197194327096827,0.759715196564627,
-1.0028031462408));
#34430=CARTESIAN_POINT('Ctrl Pts',(-0.531762717152967,0.577305158239884,
-0.992369183638318));
#34431=CARTESIAN_POINT('Ctrl Pts',(-0.740989631772397,0.258818817356289,
-0.981935221035838));
#34432=CARTESIAN_POINT('Ctrl Pts',(-0.775558326712226,-0.120673526448064,
-0.971501258433358));
#34433=CARTESIAN_POINT('Ctrl Pts',(-0.62732063238631,-0.471721998562323,
-0.961067295830877));
#34434=CARTESIAN_POINT('Ctrl Pts',(-0.331217568484232,-0.711581154688748,
-0.950633333228396));
#34435=CARTESIAN_POINT('Ctrl Pts',(0.0429565901738457,-0.783713946820615,
-0.940199370625916));
#34436=CARTESIAN_POINT('Ctrl Pts',(0.407005476575291,-0.671117992759009,
-0.929765408023435));
#34437=CARTESIAN_POINT('Ctrl Pts',(0.67511934619927,-0.400333219873851,
-0.919331445420955));
#34438=CARTESIAN_POINT('Ctrl Pts',(0.784101239483766,-0.0351861433287503,
-0.908897482818473));
#34439=CARTESIAN_POINT('Ctrl Pts',(0.70826309976199,0.338254637741565,-0.898463520215994));
#34440=CARTESIAN_POINT('Ctrl Pts',(0.465480689448243,0.631965621074234,
-0.888029557613512));
#34441=CARTESIAN_POINT('Ctrl Pts',(0.112980104923758,0.776716366722,-0.877595595011032));
#34442=CARTESIAN_POINT('Ctrl Pts',(-0.266150952393824,0.738387763304695,
-0.867161632408551));
#34443=CARTESIAN_POINT('Ctrl Pts',(-0.582547728300971,0.526014222908733,
-0.856727669806071));
#34444=CARTESIAN_POINT('Ctrl Pts',(-0.761632528456596,0.189654185427614,
-0.846293707203591));
#34445=CARTESIAN_POINT('Ctrl Pts',(-0.761193381991245,-0.191409126391062,
-0.835859744601108));
#34446=CARTESIAN_POINT('Ctrl Pts',(-0.581333799855445,-0.527355507791801,
-0.82542578199863));
#34447=CARTESIAN_POINT('Ctrl Pts',(-0.264448376313448,-0.738999238645273,
-0.814991819396148));
#34448=CARTESIAN_POINT('Ctrl Pts',(0.114770015450622,-0.77645390204848,
-0.804557856793668));
#34449=CARTESIAN_POINT('Ctrl Pts',(0.466936035686987,-0.630891081748588,
-0.794123894191188));
#34450=CARTESIAN_POINT('Ctrl Pts',(0.709040842918429,-0.336621302841119,
-0.783689931588707));
#34451=CARTESIAN_POINT('Ctrl Pts',(0.784018058194348,0.0369932815265814,
-0.773255968986227));
#34452=CARTESIAN_POINT('Ctrl Pts',(0.674194847057107,0.401888201686226,
-0.762822006383746));
#34453=CARTESIAN_POINT('Ctrl Pts',(0.405457572755745,0.672054294791692,
-0.752388043781264));
#34454=CARTESIAN_POINT('Ctrl Pts',(0.0411501370855589,0.783810873024088,
-0.741954081178785));
#34455=CARTESIAN_POINT('Ctrl Pts',(-0.332856772724146,0.710815860335577,
-0.731520118576304));
#34456=CARTESIAN_POINT('Ctrl Pts',(-0.628406212210275,0.470274867400413,
-0.721086155973823));
#34457=CARTESIAN_POINT('Ctrl Pts',(-0.775834400197947,0.118885667439072,
-0.710652193371343));
#34458=CARTESIAN_POINT('Ctrl Pts',(-0.74039112689201,-0.260526001912516,
-0.700218230768861));
#34459=CARTESIAN_POINT('Ctrl Pts',(-0.530430704992227,-0.578529243560246,
-0.689784268166382));
#34460=CARTESIAN_POINT('Ctrl Pts',(-0.195442779655914,-0.760167704084639,
-0.6793503055639));
#34461=CARTESIAN_POINT('Ctrl Pts',(0.185612846088945,-0.762627490862808,
-0.668916342961421));
#34462=CARTESIAN_POINT('Ctrl Pts',(0.52291777917247,-0.585328809028116,
-0.658482380358939));
#34463=CARTESIAN_POINT('Ctrl Pts',(0.736966076059816,-0.27006262457056,
-0.648048417756459));
#34464=CARTESIAN_POINT('Ctrl Pts',(0.777304541031368,0.108859859199587,
-0.637614455153979));
#34465=CARTESIAN_POINT('Ctrl Pts',(0.634425018694941,0.462123050828311,
-0.627180492551498));
#34466=CARTESIAN_POINT('Ctrl Pts',(0.342005555592328,0.70645949522738,-0.616746529949017));
#34467=CARTESIAN_POINT('Ctrl Pts',(-0.0310278319582662,0.784276795587446,
-0.606312567346536));
#34468=CARTESIAN_POINT('Ctrl Pts',(-0.396747667841734,0.677232682698558,
-0.595878604744056));
#34469=CARTESIAN_POINT('Ctrl Pts',(-0.668950348821351,0.410558460227938,
-0.585444642141575));
#34470=CARTESIAN_POINT('Ctrl Pts',(-0.783475144171482,0.0471117492608272,
-0.575010679539094));
#34471=CARTESIAN_POINT('Ctrl Pts',(-0.713327483047265,-0.32743964387715,
-0.564576716936614));
#34472=CARTESIAN_POINT('Ctrl Pts',(-0.475041828592946,-0.624810434884062,
-0.554142754334133));
#34473=CARTESIAN_POINT('Ctrl Pts',(-0.12478434954795,-0.774907532910112,
-0.543708791731654));
#34474=CARTESIAN_POINT('Ctrl Pts',(0.254885973710434,-0.742351640975236,
-0.533274829129171));
#34475=CARTESIAN_POINT('Ctrl Pts',(0.574477276930804,-0.534816488847445,
-0.522840866526692));
#34476=CARTESIAN_POINT('Ctrl Pts',(0.758658885652574,-0.201220062800251,
-0.51240690392421));
#34477=CARTESIAN_POINT('Ctrl Pts',(0.764017463316078,0.179805823601479,
-0.501972941321731));
#34478=CARTESIAN_POINT('Ctrl Pts',(0.589289942793166,0.518449787130605,
-0.49153897871925));
#34479=CARTESIAN_POINT('Ctrl Pts',(0.275661243182654,0.734890262188806,
-0.481105016116769));
#34480=CARTESIAN_POINT('Ctrl Pts',(-0.102943402776662,0.778110194174133,
-0.470671053514289));
#34481=CARTESIAN_POINT('Ctrl Pts',(-0.45728332099061,0.637922238832241,
-0.460237090911808));
#34482=CARTESIAN_POINT('Ctrl Pts',(-0.7038372617931,0.347370015062498,-0.449803128309328));
#34483=CARTESIAN_POINT('Ctrl Pts',(-0.78449014362719,-0.0250605866805392,
-0.439369165706847));
#34484=CARTESIAN_POINT('Ctrl Pts',(-0.680231324073692,-0.391584172562934,
-0.428935203104366));
#34485=CARTESIAN_POINT('Ctrl Pts',(-0.415635586978078,-0.665807687917839,
-0.418501240501886));
#34486=CARTESIAN_POINT('Ctrl Pts',(-0.0530706348834358,-0.783094072360267,
-0.408067277899405));
#34487=CARTESIAN_POINT('Ctrl Pts',(0.32200356473851,-0.715797822537027,
-0.397633315296924));
#34488=CARTESIAN_POINT('Ctrl Pts',(0.621178497185401,-0.479781297142652,
-0.387199352694444));
#34489=CARTESIAN_POINT('Ctrl Pts',(0.773935818505536,-0.130675809869565,
-0.376765390091964));
#34490=CARTESIAN_POINT('Ctrl Pts',(0.744269192090715,0.249231194201058,
-0.366331427489482));
#34491=CARTESIAN_POINT('Ctrl Pts',(0.5391713206469,0.57039206291312,-0.355897464887002));
#34492=CARTESIAN_POINT('Ctrl Pts',(0.206985700515677,0.757106160489391,
-0.345463502284521));
#34493=CARTESIAN_POINT('Ctrl Pts',(-0.173988395026941,0.765363218892891,
-0.335029539682041));
#34494=CARTESIAN_POINT('Ctrl Pts',(-0.513951790203906,0.593216971932302,
-0.324595577079561));
#34495=CARTESIAN_POINT('Ctrl Pts',(-0.73277191725422,0.281243908077434,
-0.314161614477079));
#34496=CARTESIAN_POINT('Ctrl Pts',(-0.778870814680853,-0.0970209884795414,
-0.303727651874599));
#34497=CARTESIAN_POINT('Ctrl Pts',(-0.641382540095329,-0.452417126489892,
-0.293293689272119));
#34498=CARTESIAN_POINT('Ctrl Pts',(-0.352714370131861,-0.701174293940717,
-0.282859726669638));
#34499=CARTESIAN_POINT('Ctrl Pts',(0.0190918897513265,-0.784658090821038,
-0.272425764067158));
#34500=CARTESIAN_POINT('Ctrl Pts',(0.386398017223727,-0.683190595956685,
-0.261991801464677));
#34501=CARTESIAN_POINT('Ctrl Pts',(0.662626488959985,-0.420688662481488,
-0.251557838862196));
#34502=CARTESIAN_POINT('Ctrl Pts',(0.782667689483342,-0.0590264425752619,
-0.241123876259716));
#34503=CARTESIAN_POINT('Ctrl Pts',(0.718226716476135,0.316548837101499,
-0.230689913657235));
#34504=CARTESIAN_POINT('Ctrl Pts',(0.484493036851995,0.617510634526485,
-0.220255951054755));
#34505=CARTESIAN_POINT('Ctrl Pts',(0.136559632479492,0.772919263601255,
-0.209821988452274));
#34506=CARTESIAN_POINT('Ctrl Pts',(-0.243561843146319,0.746143766900965,
-0.199388025849793));
#34507=CARTESIAN_POINT('Ctrl Pts',(-0.566274128183446,0.543494756230508,
-0.188954063247312));
#34508=CARTESIAN_POINT('Ctrl Pts',(-0.755509047325738,0.212739737177783,
-0.178520100644832));
#34509=CARTESIAN_POINT('Ctrl Pts',(-0.766665803559577,-0.168161640964725,
-0.168086138042351));
#34510=CARTESIAN_POINT('Ctrl Pts',(-0.597107457561118,-0.509422584813046,
-0.157652175439871));
#34511=CARTESIAN_POINT('Ctrl Pts',(-0.286814649975479,-0.730614045087353,
-0.14721821283739));
#34512=CARTESIAN_POINT('Ctrl Pts',(0.0911015483498663,-0.779580681377717,
-0.13678425023491));
#34513=CARTESIAN_POINT('Ctrl Pts',(0.447507596061844,-0.644816980204478,
-0.126350287632429));
#34514=CARTESIAN_POINT('Ctrl Pts',(0.698507324942248,-0.358015175128559,
-0.115916325029949));
#34515=CARTESIAN_POINT('Ctrl Pts',(0.755950846588162,-0.110628321320819,
-0.108960349961628));
#34516=CARTESIAN_POINT('Ctrl Pts',(0.753890288033488,0.0126055820648028,
-0.105482362427468));
#34517=CARTESIAN_POINT('Ctrl Pts',(-0.459778808448979,0.601851132366393,
-1.12625));
#34518=CARTESIAN_POINT('Ctrl Pts',(-0.558161082255852,0.526692871143935,
-1.12277201246584));
#34519=CARTESIAN_POINT('Ctrl Pts',(-0.717287384517958,0.327300059154954,
-1.11581603739752));
#34520=CARTESIAN_POINT('Ctrl Pts',(-0.786877139371749,-0.0491576947563845,
-1.10538207479504));
#34521=CARTESIAN_POINT('Ctrl Pts',(-0.670999603978842,-0.41393738145968,
-1.09494811219256));
#34522=CARTESIAN_POINT('Ctrl Pts',(-0.396958121390901,-0.681192740453033,
-1.08451414959008));
#34523=CARTESIAN_POINT('Ctrl Pts',(-0.0293513702614931,-0.787862050964758,
-1.0740801869876));
#34524=CARTESIAN_POINT('Ctrl Pts',(0.345174528791177,-0.70883629909999,
-1.06364622438512));
#34525=CARTESIAN_POINT('Ctrl Pts',(0.638339163802789,-0.462725361017625,
-1.05321226178264));
#34526=CARTESIAN_POINT('Ctrl Pts',(0.781041451767081,-0.107548656621832,
-1.04277829918015));
#34527=CARTESIAN_POINT('Ctrl Pts',(0.73964482858492,0.272979776873333,-1.03234433657767));
#34528=CARTESIAN_POINT('Ctrl Pts',(0.523907016570375,0.589163548674701,
-1.02191037397519));
#34529=CARTESIAN_POINT('Ctrl Pts',(0.184679370276391,0.766476320999641,
-1.01147641137271));
#34530=CARTESIAN_POINT('Ctrl Pts',(-0.198078926680871,0.763123222427557,
-1.00104244877023));
#34531=CARTESIAN_POINT('Ctrl Pts',(-0.534148165188284,0.579894906686739,
-0.990608486167751));
#34532=CARTESIAN_POINT('Ctrl Pts',(-0.744313656594542,0.25997985934869,
-0.980174523565271));
#34533=CARTESIAN_POINT('Ctrl Pts',(-0.779037423985492,-0.121214858921561,
-0.969740560962792));
#34534=CARTESIAN_POINT('Ctrl Pts',(-0.630134746400966,-0.473838108603289,
-0.959306598360309));
#34535=CARTESIAN_POINT('Ctrl Pts',(-0.332703386000083,-0.714773255138962,
-0.94887263575783));
#34536=CARTESIAN_POINT('Ctrl Pts',(0.0431492902551158,-0.78722962966257,
-0.938438673155349));
#34537=CARTESIAN_POINT('Ctrl Pts',(0.408831273062274,-0.67412857846459,
-0.928004710552867));
#34538=CARTESIAN_POINT('Ctrl Pts',(0.678147881681892,-0.402129085108458,
-0.917570747950389));
#34539=CARTESIAN_POINT('Ctrl Pts',(0.787618659686819,-0.0353439857660798,
-0.907136785347906));
#34540=CARTESIAN_POINT('Ctrl Pts',(0.711440315674566,0.339772023043393,
-0.896702822745428));
#34541=CARTESIAN_POINT('Ctrl Pts',(0.467568801414539,0.634800572137751,
-0.886268860142945));
#34542=CARTESIAN_POINT('Ctrl Pts',(0.113486925323206,0.78020065893068,-0.875834897540465));
#34543=CARTESIAN_POINT('Ctrl Pts',(-0.267344885893195,0.741700116231729,
-0.865400934937985));
#34544=CARTESIAN_POINT('Ctrl Pts',(-0.585160994350141,0.528373883831427,
-0.854966972335503));
#34545=CARTESIAN_POINT('Ctrl Pts',(-0.765049155681855,0.19050496008484,
-0.844533009733023));
#34546=CARTESIAN_POINT('Ctrl Pts',(-0.764608039237945,-0.192267773583724,
-0.834099047130543));
#34547=CARTESIAN_POINT('Ctrl Pts',(-0.583941620311302,-0.52972118561936,
-0.823665084528062));
#34548=CARTESIAN_POINT('Ctrl Pts',(-0.265634672182434,-0.742314334605435,
-0.813231121925581));
#34549=CARTESIAN_POINT('Ctrl Pts',(0.115284865256511,-0.779937016860141,
-0.802797159323101));
#34550=CARTESIAN_POINT('Ctrl Pts',(0.469030676228697,-0.63372121250791,
-0.79236319672062));
#34551=CARTESIAN_POINT('Ctrl Pts',(0.712221547729785,-0.338131361123721,
-0.781929234118141));
#34552=CARTESIAN_POINT('Ctrl Pts',(0.787535105251363,0.0371592306530875,
-0.771495271515659));
#34553=CARTESIAN_POINT('Ctrl Pts',(0.677219235306731,0.403691042452731,
-0.761061308913179));
#34554=CARTESIAN_POINT('Ctrl Pts',(0.407276425457032,0.675069080682076,
-0.750627346310697));
#34555=CARTESIAN_POINT('Ctrl Pts',(0.0413347335588409,0.787326990663742,
-0.740193383708218));
#34556=CARTESIAN_POINT('Ctrl Pts',(-0.334349943602904,0.714004527743863,
-0.729759421105736));
#34557=CARTESIAN_POINT('Ctrl Pts',(-0.631225196028523,0.472384485694395,
-0.719325458503257));
#34558=CARTESIAN_POINT('Ctrl Pts',(-0.779314735970096,0.119418979755564,
-0.708891495900775));
#34559=CARTESIAN_POINT('Ctrl Pts',(-0.743712466759963,-0.261694702299867,
-0.698457533298295));
#34560=CARTESIAN_POINT('Ctrl Pts',(-0.532810177927122,-0.581124482983871,
-0.688023570695815));
#34561=CARTESIAN_POINT('Ctrl Pts',(-0.19631952151896,-0.763577760216057,
-0.677589608093334));
#34562=CARTESIAN_POINT('Ctrl Pts',(0.186445491596607,-0.766048581415893,
-0.667155645490853));
#34563=CARTESIAN_POINT('Ctrl Pts',(0.525263549677469,-0.587954550799829,
-0.656721682888373));
#34564=CARTESIAN_POINT('Ctrl Pts',(0.740272051402901,-0.271274105542239,
-0.646287720285891));
#34565=CARTESIAN_POINT('Ctrl Pts',(0.780791471746632,0.109348196481392,
-0.635853757683412));
#34566=CARTESIAN_POINT('Ctrl Pts',(0.637271002434187,0.464196100675705,
-0.625419795080931));
#34567=CARTESIAN_POINT('Ctrl Pts',(0.343539767234785,0.709628620303799,
-0.61498583247845));
#34568=CARTESIAN_POINT('Ctrl Pts',(-0.0311670205189552,0.787795003321279,
-0.604551869875969));
#34569=CARTESIAN_POINT('Ctrl Pts',(-0.398527448553385,0.680270698454323,
-0.594117907273489));
#34570=CARTESIAN_POINT('Ctrl Pts',(-0.671951210639545,0.412400195133385,
-0.583683944671008));
#34571=CARTESIAN_POINT('Ctrl Pts',(-0.78698975575632,0.0473230890856653,
-0.573249982068528));
#34572=CARTESIAN_POINT('Ctrl Pts',(-0.716527417409385,-0.328908513916318,
-0.562816019466047));
#34573=CARTESIAN_POINT('Ctrl Pts',(-0.477172831122479,-0.627613288311012,
-0.552382056863567));
#34574=CARTESIAN_POINT('Ctrl Pts',(-0.125344122916371,-0.778383710824121,
-0.541948094261086));
#34575=CARTESIAN_POINT('Ctrl Pts',(0.256029373348162,-0.74568177556445,
-0.531514131658605));
#34576=CARTESIAN_POINT('Ctrl Pts',(0.577054339531638,-0.537215636084532,
-0.521080169056125));
#34577=CARTESIAN_POINT('Ctrl Pts',(0.762062173336032,-0.202122721128445,
-0.510646206453644));
#34578=CARTESIAN_POINT('Ctrl Pts',(0.767444789182847,0.180612419235498,
-0.500212243851163));
#34579=CARTESIAN_POINT('Ctrl Pts',(0.591933453918155,0.520775514553563,
-0.489778281248683));
#34580=CARTESIAN_POINT('Ctrl Pts',(0.276897839143596,0.738186925584305,
-0.479344318646202));
#34581=CARTESIAN_POINT('Ctrl Pts',(-0.103405199272279,0.781600738989841,
-0.468910356043722));
#34582=CARTESIAN_POINT('Ctrl Pts',(-0.459334660167689,0.640783910842521,
-0.458476393441241));
#34583=CARTESIAN_POINT('Ctrl Pts',(-0.706994623724161,0.348928291273615,
-0.448042430838761));
#34584=CARTESIAN_POINT('Ctrl Pts',(-0.78800930842456,-0.0251730066199923,
-0.43760846823628));
#34585=CARTESIAN_POINT('Ctrl Pts',(-0.683282791513017,-0.393340790216431,
-0.4271745056338));
#34586=CARTESIAN_POINT('Ctrl Pts',(-0.417500097498841,-0.668794451991519,
-0.416740543031319));
#34587=CARTESIAN_POINT('Ctrl Pts',(-0.0533087058287156,-0.786606974485123,
-0.406306580428838));
#34588=CARTESIAN_POINT('Ctrl Pts',(0.323448048928478,-0.719008838659509,
-0.395872617826358));
#34589=CARTESIAN_POINT('Ctrl Pts',(0.623965058008296,-0.481933560577751,
-0.385438655223877));
#34590=CARTESIAN_POINT('Ctrl Pts',(0.777407637380551,-0.131262011893554,
-0.375004692621396));
#34591=CARTESIAN_POINT('Ctrl Pts',(0.747607928672497,0.250349226915972,
-0.364570730018916));
#34592=CARTESIAN_POINT('Ctrl Pts',(0.541590003337538,0.572950799545676,
-0.354136767416435));
#34593=CARTESIAN_POINT('Ctrl Pts',(0.207914223068499,0.760502482762855,
-0.343702804813955));
#34594=CARTESIAN_POINT('Ctrl Pts',(-0.174768894106406,0.768796581719083,
-0.333268842211474));
#34595=CARTESIAN_POINT('Ctrl Pts',(-0.516257339945076,0.595878099420955,
-0.322834879608994));
#34596=CARTESIAN_POINT('Ctrl Pts',(-0.736059077911029,0.282505547458041,
-0.312400917006512));
#34597=CARTESIAN_POINT('Ctrl Pts',(-0.782364771583725,-0.0974562174576635,
-0.301966954404033));
#34598=CARTESIAN_POINT('Ctrl Pts',(-0.644259734761709,-0.454446636287429,
-0.291532991801551));
#34599=CARTESIAN_POINT('Ctrl Pts',(-0.354296620723981,-0.704319709976538,
-0.281099029199071));
#34600=CARTESIAN_POINT('Ctrl Pts',(0.0191775345559673,-0.788178009053099,
-0.270665066596591));
#34601=CARTESIAN_POINT('Ctrl Pts',(0.388131370170813,-0.686255338400113,
-0.26023110399411));
#34602=CARTESIAN_POINT('Ctrl Pts',(0.665598982404191,-0.422575840864817,
-0.249797141391629));
#34603=CARTESIAN_POINT('Ctrl Pts',(0.786178678898116,-0.0592912305593806,
-0.239363178789148));
#34604=CARTESIAN_POINT('Ctrl Pts',(0.721448628413702,0.317968851246866,
-0.228929216186668));
#34605=CARTESIAN_POINT('Ctrl Pts',(0.486666436849571,0.620280742650431,
-0.218495253584187));
#34606=CARTESIAN_POINT('Ctrl Pts',(0.137172228805461,0.776386520196726,
-0.208061290981707));
#34607=CARTESIAN_POINT('Ctrl Pts',(-0.24465444339174,0.749490916798135,
-0.197627328379226));
#34608=CARTESIAN_POINT('Ctrl Pts',(-0.568814392418833,0.545932825443553,
-0.187193365776746));
#34609=CARTESIAN_POINT('Ctrl Pts',(-0.758898204371723,0.213694087832844,
-0.176759403174265));
#34610=CARTESIAN_POINT('Ctrl Pts',(-0.770105011053624,-0.16891603298111,
-0.166325440571784));
#34611=CARTESIAN_POINT('Ctrl Pts',(-0.599786034786057,-0.511707755229724,
-0.155891477969304));
#34612=CARTESIAN_POINT('Ctrl Pts',(-0.288101284597239,-0.733891647041663,
-0.145457515366823));
#34613=CARTESIAN_POINT('Ctrl Pts',(0.0915102336223773,-0.783077583290339,
-0.135023552764343));
#34614=CARTESIAN_POINT('Ctrl Pts',(0.449515061170511,-0.64771005951776,
-0.124589590161862));
#34615=CARTESIAN_POINT('Ctrl Pts',(0.701640821699945,-0.35962018580118,
-0.114155627559382));
#34616=CARTESIAN_POINT('Ctrl Pts',(0.759341912736311,-0.111126206723824,
-0.107199652491061));
#34617=CARTESIAN_POINT('Ctrl Pts',(0.757272083693561,0.0126621280946378,
-0.103721664956901));
#34618=CARTESIAN_POINT('Ctrl Pts',(0.555007866453731,-0.51535192480862,
-0.12));
#34619=CARTESIAN_POINT('Ctrl Pts',(0.591072083605958,-0.472049785910246,
-0.12));
#34620=CARTESIAN_POINT('Ctrl Pts',(0.641266713589829,-0.405214104043369,
-0.12));
#34621=CARTESIAN_POINT('Ctrl Pts',(0.703252213124764,-0.26398462653494,
-0.12));
#34622=CARTESIAN_POINT('Ctrl Pts',(0.719761895146736,-0.212714660677395,
-0.12));
#34623=CARTESIAN_POINT('Ctrl Pts',(0.74280866170717,-0.103336683918317,
-0.12));
#34624=CARTESIAN_POINT('Ctrl Pts',(0.748364886323481,-0.0454765203713978,
-0.12));
#34625=CARTESIAN_POINT('Ctrl Pts',(0.747395528060274,0.0124969850565462,
-0.12));
#34626=CARTESIAN_POINT('',(-0.738674446606903,0.114170753859866,-1.12625));
#34627=CARTESIAN_POINT('Ctrl Pts',(-0.738728321778977,0.114178441930237,
-1.12625));
#34628=CARTESIAN_POINT('Ctrl Pts',(-0.729872306490507,0.171476380149586,
-1.12625));
#34629=CARTESIAN_POINT('Ctrl Pts',(-0.714604763127109,0.227558322531749,
-1.12625));
#34630=CARTESIAN_POINT('Ctrl Pts',(-0.673382241080466,0.331452140304365,
-1.12625));
#34631=CARTESIAN_POINT('Ctrl Pts',(-0.648435827358878,0.379185799077542,
-1.12625));
#34632=CARTESIAN_POINT('Ctrl Pts',(-0.563441537104106,0.507894222797761,
-1.12625));
#34633=CARTESIAN_POINT('Ctrl Pts',(-0.50265383037774,0.565275533421068,
-1.12625));
#34634=CARTESIAN_POINT('Ctrl Pts',(-0.459778808448982,0.60185113236639,
-1.12625));
#34635=CARTESIAN_POINT('Ctrl Pts',(-0.738674444793491,0.11417075360109,
-1.12625));
#34636=CARTESIAN_POINT('Ctrl Pts',(-0.744523251396961,0.0764015856923646,
-1.12516243468899));
#34637=CARTESIAN_POINT('Ctrl Pts',(-0.747504748693495,0.0381902463136716,
-1.12407486937799));
#34638=CARTESIAN_POINT('Ctrl Pts',(-0.747536615034749,-1.54000427280091E-5,
-1.12298730406698));
#34639=CARTESIAN_POINT('Origin',(-9.99409214431492E-17,0.,-1.12625));
#34640=CARTESIAN_POINT('',(-0.82685,-1.01259920587499E-16,-1.12625));
#34641=CARTESIAN_POINT('Origin',(0.,0.,-1.12625));
#34642=CARTESIAN_POINT('Origin',(0.,0.,-1.12625));
#34643=CARTESIAN_POINT('',(0.589301091561372,-0.565833523687256,-1.12625));
#34644=CARTESIAN_POINT('Ctrl Pts',(0.82685,-4.02455846426619E-15,-1.12625));
#34645=CARTESIAN_POINT('Ctrl Pts',(0.82685,-0.0640849384885572,-1.12625));
#34646=CARTESIAN_POINT('Ctrl Pts',(0.819177389464161,-0.127972397977404,
-1.12625));
#34647=CARTESIAN_POINT('Ctrl Pts',(0.789918090291955,-0.247778859616483,
-1.12625));
#34648=CARTESIAN_POINT('Ctrl Pts',(0.769494724754842,-0.303642805552845,
-1.12625));
#34649=CARTESIAN_POINT('Ctrl Pts',(0.695180543122701,-0.45245484006238,
-1.12625));
#34650=CARTESIAN_POINT('Ctrl Pts',(0.636182670612352,-0.521654825860832,
-1.12625));
#34651=CARTESIAN_POINT('Ctrl Pts',(0.589301091561372,-0.565833523687256,
-1.12625));
#34652=CARTESIAN_POINT('',(-0.459778808448984,-0.601851132366389,-1.12625));
#34653=CARTESIAN_POINT('Ctrl Pts',(0.589349009255746,-0.565869316348659,
-1.12625));
#34654=CARTESIAN_POINT('Ctrl Pts',(0.561797955794771,-0.591801457111584,
-1.12625));
#34655=CARTESIAN_POINT('Ctrl Pts',(0.53250376759913,-0.615719001693644,
-1.12625));
#34656=CARTESIAN_POINT('Ctrl Pts',(0.50171824497732,-0.637497823098451,
-1.12625));
#34657=CARTESIAN_POINT('Ctrl Pts',(0.47102306597979,-0.659212732070052,
-1.12625));
#34658=CARTESIAN_POINT('Ctrl Pts',(0.438844183868412,-0.678802004601254,
-1.12625));
#34659=CARTESIAN_POINT('Ctrl Pts',(0.405405868387424,-0.696097894311317,
-1.12625));
#34660=CARTESIAN_POINT('Ctrl Pts',(0.394915382569507,-0.701524073324875,
-1.12625));
#34661=CARTESIAN_POINT('Ctrl Pts',(0.384300816323456,-0.706724162922218,
-1.12625));
#34662=CARTESIAN_POINT('Ctrl Pts',(0.373568843076819,-0.71169193771826,
-1.12625));
#34663=CARTESIAN_POINT('Ctrl Pts',(0.363930578232978,-0.716153440562932,
-1.12625));
#34664=CARTESIAN_POINT('Ctrl Pts',(0.354194037388044,-0.720428823536218,
-1.12625));
#34665=CARTESIAN_POINT('Ctrl Pts',(0.344389136277292,-0.724503440483072,
-1.12625));
#34666=CARTESIAN_POINT('Ctrl Pts',(0.319404665564138,-0.734886222178274,
-1.12625));
#34667=CARTESIAN_POINT('Ctrl Pts',(0.293946819978443,-0.74398129459371,
-1.12625));
#34668=CARTESIAN_POINT('Ctrl Pts',(0.268101859965993,-0.751732914379289,
-1.12625));
#34669=CARTESIAN_POINT('Ctrl Pts',(0.236780787659365,-0.76112697200912,
-1.12625));
#34670=CARTESIAN_POINT('Ctrl Pts',(0.204890853635393,-0.768548833828937,
-1.12625));
#34671=CARTESIAN_POINT('Ctrl Pts',(0.172622384826077,-0.773986220742674,
-1.12625));
#34672=CARTESIAN_POINT('Ctrl Pts',(0.153540924365737,-0.777201535482743,
-1.12625));
#34673=CARTESIAN_POINT('Ctrl Pts',(0.134327020168648,-0.779722340056214,
-1.12625));
#34674=CARTESIAN_POINT('Ctrl Pts',(0.115020357875576,-0.781541004368796,
-1.12625));
#34675=CARTESIAN_POINT('Ctrl Pts',(0.103888024742563,-0.782589656729181,
-1.12625));
#34676=CARTESIAN_POINT('Ctrl Pts',(0.0927190764996314,-0.783404877148015,
-1.12625));
#34677=CARTESIAN_POINT('Ctrl Pts',(0.0815541189285967,-0.783983582560309,
-1.12625));
#34678=CARTESIAN_POINT('Ctrl Pts',(0.0448646731867934,-0.78588528085963,
-1.12625));
#34679=CARTESIAN_POINT('Ctrl Pts',(0.00816270548253231,-0.785244764668211,
-1.12625));
#34680=CARTESIAN_POINT('Ctrl Pts',(-0.0282824614483715,-0.782055278068206,
-1.12625));
#34681=CARTESIAN_POINT('Ctrl Pts',(-0.0590932645533356,-0.779358880934808,
-1.12625));
#34682=CARTESIAN_POINT('Ctrl Pts',(-0.0897210642546043,-0.774839835383014,
-1.12625));
#34683=CARTESIAN_POINT('Ctrl Pts',(-0.119998031533345,-0.768465408942048,
-1.12625));
#34684=CARTESIAN_POINT('Ctrl Pts',(-0.136473000057242,-0.764996816001217,
-1.12625));
#34685=CARTESIAN_POINT('Ctrl Pts',(-0.15284394986517,-0.760978380225078,
-1.12625));
#34686=CARTESIAN_POINT('Ctrl Pts',(-0.169085499191771,-0.756419224292495,
-1.12625));
#34687=CARTESIAN_POINT('Ctrl Pts',(-0.177940972575151,-0.753933409472752,
-1.12625));
#34688=CARTESIAN_POINT('Ctrl Pts',(-0.186757956444784,-0.751286813976276,
-1.12625));
#34689=CARTESIAN_POINT('Ctrl Pts',(-0.195532162363131,-0.748480681723287,
-1.12625));
#34690=CARTESIAN_POINT('Ctrl Pts',(-0.202583374992159,-0.746225590451764,
-1.12625));
#34691=CARTESIAN_POINT('Ctrl Pts',(-0.209606136438257,-0.743867596213384,
-1.12625));
#34692=CARTESIAN_POINT('Ctrl Pts',(-0.216586046839137,-0.741412001951311,
-1.12625));
#34693=CARTESIAN_POINT('Ctrl Pts',(-0.250777745045288,-0.72938305987278,
-1.12625));
#34694=CARTESIAN_POINT('Ctrl Pts',(-0.284021591248731,-0.714991447728378,
-1.12625));
#34695=CARTESIAN_POINT('Ctrl Pts',(-0.316082870432815,-0.6983703238303,
-1.12625));
#34696=CARTESIAN_POINT('Ctrl Pts',(-0.347689999419729,-0.681984639281106,
-1.12625));
#34697=CARTESIAN_POINT('Ctrl Pts',(-0.378148790586058,-0.663431461241488,
-1.12625));
#34698=CARTESIAN_POINT('Ctrl Pts',(-0.40720704752916,-0.642797035900976,
-1.12625));
#34699=CARTESIAN_POINT('Ctrl Pts',(-0.42529729927964,-0.629951050339376,
-1.12625));
#34700=CARTESIAN_POINT('Ctrl Pts',(-0.442844152594049,-0.616297659807387,
-1.12625));
#34701=CARTESIAN_POINT('Ctrl Pts',(-0.459778808448986,-0.601851132366388,
-1.12625));
#34702=CARTESIAN_POINT('Ctrl Pts',(-0.459778808448986,-0.601851132366387,
-1.12625));
#34703=CARTESIAN_POINT('Ctrl Pts',(-0.506938887193883,-0.5616200596157,
-1.12625));
#34704=CARTESIAN_POINT('Ctrl Pts',(-0.580457877279435,-0.492400554929899,
-1.12625));
#34705=CARTESIAN_POINT('Ctrl Pts',(-0.691141067841612,-0.302309651856748,
-1.12625));
#34706=CARTESIAN_POINT('Ctrl Pts',(-0.723888788631575,-0.210189415916573,
-1.12625));
#34707=CARTESIAN_POINT('Ctrl Pts',(-0.738728321778978,-0.114178441930233,
-1.12625));
#34708=CARTESIAN_POINT('Origin',(0.,0.,-1.12625));
#34709=CARTESIAN_POINT('Origin',(0.,0.,-1.33003901172249));
#34710=CARTESIAN_POINT('Ctrl Pts',(-0.748490343485035,-0.115687267835002,
-1.1425283350431));
#34711=CARTESIAN_POINT('Ctrl Pts',(-0.72957939383647,-0.238040085590799,
-1.13905034750894));
#34712=CARTESIAN_POINT('Ctrl Pts',(-0.630653629844317,-0.473183377928881,
-1.13209437244062));
#34713=CARTESIAN_POINT('Ctrl Pts',(-0.333406559150428,-0.714445366112161,
-1.12166040983814));
#34714=CARTESIAN_POINT('Ctrl Pts',(0.0423441932323986,-0.787268438306115,
-1.11122644723566));
#34715=CARTESIAN_POINT('Ctrl Pts',(0.408154628293017,-0.674543622261519,
-1.10079248463318));
#34716=CARTESIAN_POINT('Ctrl Pts',(0.677738701453828,-0.402813068451861,
-1.0903585220307));
#34717=CARTESIAN_POINT('Ctrl Pts',(0.787583785039379,-0.0361404951497401,
-1.07992455942821));
#34718=CARTESIAN_POINT('Ctrl Pts',(0.711782686348953,0.339053175380463,
-1.06949059682573));
#34719=CARTESIAN_POINT('Ctrl Pts',(0.468210400798597,0.634327583870302,
-1.05905663422325));
#34720=CARTESIAN_POINT('Ctrl Pts',(0.114275158775038,0.780085648735316,
-1.04862267162077));
#34721=CARTESIAN_POINT('Ctrl Pts',(-0.266595119432202,0.74196987248233,
-1.03818870901829));
#34722=CARTESIAN_POINT('Ctrl Pts',(-0.584626774041373,0.528964985372604,
-1.02775474641581));
#34723=CARTESIAN_POINT('Ctrl Pts',(-0.764856223313065,0.19127799592914,
-1.01732078381333));
#34724=CARTESIAN_POINT('Ctrl Pts',(-0.764801961726996,-0.191494973175329,
-1.00688682121085));
#34725=CARTESIAN_POINT('Ctrl Pts',(-0.584476642087926,-0.529130798350251,
-0.99645285860837));
#34726=CARTESIAN_POINT('Ctrl Pts',(-0.266384707070968,-0.742045509438616,
-0.98601889600589));
#34727=CARTESIAN_POINT('Ctrl Pts',(0.114496619465385,-0.780053123936526,
-0.975584933403408));
#34728=CARTESIAN_POINT('Ctrl Pts',(0.468390010412392,-0.634194881491942,
-0.965150970800929));
#34729=CARTESIAN_POINT('Ctrl Pts',(0.711879475926064,-0.338850945209237,
-0.954717008198448));
#34730=CARTESIAN_POINT('Ctrl Pts',(0.787572255433587,0.0363633449241354,
-0.944283045595968));
#34731=CARTESIAN_POINT('Ctrl Pts',(0.677626851623736,0.403006452460033,
-0.933849082993486));
#34732=CARTESIAN_POINT('Ctrl Pts',(0.407958428506616,0.674657150909495,
-0.923415120391007));
#34733=CARTESIAN_POINT('Ctrl Pts',(0.042130369016677,0.787284816735879,
-0.912981157788525));
#34734=CARTESIAN_POINT('Ctrl Pts',(-0.333628214598003,0.714342050500304,
-0.902547195186045));
#34735=CARTESIAN_POINT('Ctrl Pts',(-0.630747491734475,0.473022147824027,
-0.892113232583564));
#34736=CARTESIAN_POINT('Ctrl Pts',(-0.779193655806613,0.120206478312629,
-0.881679269981084));
#34737=CARTESIAN_POINT('Ctrl Pts',(-0.743976550446063,-0.260942988134434,
-0.871245307378604));
#34738=CARTESIAN_POINT('Ctrl Pts',(-0.533397178462468,-0.58058573930206,
-0.860811344776122));
#34739=CARTESIAN_POINT('Ctrl Pts',(-0.197091077355777,-0.763378973969726,
-0.850377382173643));
#34740=CARTESIAN_POINT('Ctrl Pts',(0.185671243420201,-0.766236608391142,
-0.83994341957116));
#34741=CARTESIAN_POINT('Ctrl Pts',(0.524669106735824,-0.588485071271487,
-0.829509456968682));
#34742=CARTESIAN_POINT('Ctrl Pts',(0.739997529484913,-0.272022070847804,
-0.819075494366199));
#34743=CARTESIAN_POINT('Ctrl Pts',(0.780901578249222,0.108559088795519,
-0.80864153176372));
#34744=CARTESIAN_POINT('Ctrl Pts',(0.637739784219531,0.46355185070908,-0.798207569161239));
#34745=CARTESIAN_POINT('Ctrl Pts',(0.344256728029392,0.709281083829744,
-0.787773606558758));
#34746=CARTESIAN_POINT('Ctrl Pts',(-0.0303708751141343,0.787826097953732,
-0.777339643956278));
#34747=CARTESIAN_POINT('Ctrl Pts',(-0.397839777494349,0.680673094896106,
-0.766905681353797));
#34748=CARTESIAN_POINT('Ctrl Pts',(-0.671534104459313,0.413079044760479,
-0.756471718751317));
#34749=CARTESIAN_POINT('Ctrl Pts',(-0.786941530302541,0.0481183806594935,
-0.746037756148835));
#34750=CARTESIAN_POINT('Ctrl Pts',(-0.716859439874856,-0.32818423809578,
-0.735603793546356));
#34751=CARTESIAN_POINT('Ctrl Pts',(-0.477806840690935,-0.627130746863161,
-0.725169830943874));
#34752=CARTESIAN_POINT('Ctrl Pts',(-0.126130677572575,-0.778256643304304,
-0.714735868341395));
#34753=CARTESIAN_POINT('Ctrl Pts',(0.25527567193062,-0.745940132981574,
-0.704301905738912));
#34754=CARTESIAN_POINT('Ctrl Pts',(0.576511145861978,-0.537798521166717,
-0.693867943136434));
#34755=CARTESIAN_POINT('Ctrl Pts',(0.761857523268443,-0.202892742382455,
-0.683433980533952));
#34756=CARTESIAN_POINT('Ctrl Pts',(0.767626920662054,0.179836763057753,
-0.673000017931472));
#34757=CARTESIAN_POINT('Ctrl Pts',(0.5924594368424,0.520177052904666,-0.662566055328991));
#34758=CARTESIAN_POINT('Ctrl Pts',(0.277643694393179,0.737906721500696,
-0.652132092726511));
#34759=CARTESIAN_POINT('Ctrl Pts',(-0.102615276791043,0.781704839208058,
-0.64169813012403));
#34760=CARTESIAN_POINT('Ctrl Pts',(-0.458686862609216,0.641247777962555,
-0.631264167521549));
#34761=CARTESIAN_POINT('Ctrl Pts',(-0.706641643062577,0.349642587454705,
-0.620830204919069));
#34762=CARTESIAN_POINT('Ctrl Pts',(-0.78803434551991,-0.0243766477023704,
-0.610396242316588));
#34763=CARTESIAN_POINT('Ctrl Pts',(-0.683679944886674,-0.392650077845343,
-0.599962279714107));
#34764=CARTESIAN_POINT('Ctrl Pts',(-0.418175754367012,-0.668372193565666,
-0.589528317111627));
#34765=CARTESIAN_POINT('Ctrl Pts',(-0.0541036075165375,-0.786552700285172,
-0.579094354509147));
#34766=CARTESIAN_POINT('Ctrl Pts',(0.322721268222062,-0.719335341624019,
-0.568660391906665));
#34767=CARTESIAN_POINT('Ctrl Pts',(0.623477707326195,-0.482563880889846,
-0.558226429304185));
#34768=CARTESIAN_POINT('Ctrl Pts',(0.777274589863052,-0.132047577128186,
-0.547792466701704));
#34769=CARTESIAN_POINT('Ctrl Pts',(0.747860544863849,0.24959358186489,-0.537358504099224));
#34770=CARTESIAN_POINT('Ctrl Pts',(0.542168739239194,0.572403187328635,
-0.526924541496743));
#34771=CARTESIAN_POINT('Ctrl Pts',(0.208682665163581,0.760291980710322,
-0.516490578894263));
#34772=CARTESIAN_POINT('Ctrl Pts',(-0.17399187479518,0.768972807176858,
-0.506056616291782));
#34773=CARTESIAN_POINT('Ctrl Pts',(-0.515654894268523,0.596399514326692,
-0.495622653689302));
#34774=CARTESIAN_POINT('Ctrl Pts',(-0.735773207791699,0.283249249545548,
-0.485188691086821));
#34775=CARTESIAN_POINT('Ctrl Pts',(-0.782462859663334,-0.0966655260145846,
-0.47475472848434));
#34776=CARTESIAN_POINT('Ctrl Pts',(-0.64471866003509,-0.453795328396784,
-0.46432076588186));
#34777=CARTESIAN_POINT('Ctrl Pts',(-0.355008211612258,-0.703961306010569,
-0.453886803279379));
#34778=CARTESIAN_POINT('Ctrl Pts',(0.0183810095128271,-0.788196986267641,
-0.443452840676899));
#34779=CARTESIAN_POINT('Ctrl Pts',(0.38743765390661,-0.686647227481269,
-0.433018878074418));
#34780=CARTESIAN_POINT('Ctrl Pts',(0.665171601199011,-0.423248262406725,
-0.422584915471937));
#34781=CARTESIAN_POINT('Ctrl Pts',(0.786118349198421,-0.0600857031737155,
-0.412150952869457));
#34782=CARTESIAN_POINT('Ctrl Pts',(0.721769612451196,0.317239621129978,
-0.401716990266976));
#34783=CARTESIAN_POINT('Ctrl Pts',(0.48729299311423,0.619788584544703,-0.391283027664495));
#34784=CARTESIAN_POINT('Ctrl Pts',(0.137956834542062,0.776247552318673,
-0.380849065062015));
#34785=CARTESIAN_POINT('Ctrl Pts',(-0.24389704678188,0.749737674945354,
-0.370415102459534));
#34786=CARTESIAN_POINT('Ctrl Pts',(-0.568262101448461,0.54650757977013,
-0.359981139857054));
#34787=CARTESIAN_POINT('Ctrl Pts',(-0.758682436896782,0.214460510585722,
-0.349547177254573));
#34788=CARTESIAN_POINT('Ctrl Pts',(-0.770274190049179,-0.168136916847512,
-0.339113214652093));
#34789=CARTESIAN_POINT('Ctrl Pts',(-0.600305075684733,-0.511102892647913,
-0.328679252049612));
#34790=CARTESIAN_POINT('Ctrl Pts',(-0.288838411909729,-0.73359711162755,
-0.318245289447131));
#34791=CARTESIAN_POINT('Ctrl Pts',(0.0907101808452941,-0.783175596150043,
-0.307811326844651));
#34792=CARTESIAN_POINT('Ctrl Pts',(0.448877531081785,-0.648152228766222,
-0.29737736424217));
#34793=CARTESIAN_POINT('Ctrl Pts',(0.70124022796002,-0.360353291538616,
-0.286943401639689));
#34794=CARTESIAN_POINT('Ctrl Pts',(0.78831401046138,0.0123843106225018,
-0.276509439037209));
#34795=CARTESIAN_POINT('Ctrl Pts',(0.689574771586232,0.382202801273025,
-0.266075476434728));
#34796=CARTESIAN_POINT('Ctrl Pts',(0.42829627406239,0.661932524534907,-0.255641513832248));
#34797=CARTESIAN_POINT('Ctrl Pts',(0.0660643238823282,0.785638478676651,
-0.245207551229767));
#34798=CARTESIAN_POINT('Ctrl Pts',(-0.311739618905983,0.724162157724785,
-0.234773588627286));
#34799=CARTESIAN_POINT('Ctrl Pts',(-0.616063582497866,0.491993812660696,
-0.224339626024806));
#34800=CARTESIAN_POINT('Ctrl Pts',(-0.775175608854641,0.143858286910066,
-0.213905663422325));
#34801=CARTESIAN_POINT('Ctrl Pts',(-0.751571377703373,-0.238186748774504,
-0.203471700819845));
#34802=CARTESIAN_POINT('Ctrl Pts',(-0.550814864235531,-0.564087434409687,
-0.193037738217364));
#34803=CARTESIAN_POINT('Ctrl Pts',(-0.220225801435375,-0.757030349608765,
-0.182603775614884));
#34804=CARTESIAN_POINT('Ctrl Pts',(0.162271947040125,-0.771528308468155,
-0.172169813012403));
#34805=CARTESIAN_POINT('Ctrl Pts',(0.50652186418947,-0.604181181458613,
-0.161735850409922));
#34806=CARTESIAN_POINT('Ctrl Pts',(0.731377474710374,-0.294400431622865,
-0.151301887807442));
#34807=CARTESIAN_POINT('Ctrl Pts',(0.783845102655791,0.0847288019872719,
-0.140867925204961));
#34808=CARTESIAN_POINT('Ctrl Pts',(0.651544586453759,0.443977659175325,
-0.130433962602481));
#34809=CARTESIAN_POINT('Ctrl Pts',(0.460967102820801,0.613562143858194,
-0.12347798753416));
#34810=CARTESIAN_POINT('Ctrl Pts',(0.35128376055981,0.670985139773177,-0.12));
#34811=CARTESIAN_POINT('Ctrl Pts',(-0.745983409600527,-0.115299794123061,
-1.14120781194017));
#34812=CARTESIAN_POINT('Ctrl Pts',(-0.727135791628741,-0.237242859367695,
-1.13772982440601));
#34813=CARTESIAN_POINT('Ctrl Pts',(-0.628541377473353,-0.471598508427931,
-1.13077384933769));
#34814=CARTESIAN_POINT('Ctrl Pts',(-0.332289872157584,-0.712052475912534,
-1.12033988673521));
#34815=CARTESIAN_POINT('Ctrl Pts',(0.0422023676689075,-0.784631620439639,
-1.10990592413273));
#34816=CARTESIAN_POINT('Ctrl Pts',(0.406787590016807,-0.672284365610761,
-1.09947196153025));
#34817=CARTESIAN_POINT('Ctrl Pts',(0.675468739687113,-0.401463918278453,
-1.08903799892777));
#34818=CARTESIAN_POINT('Ctrl Pts',(0.784945917892683,-0.036019450074174,
-1.07860403632529));
#34819=CARTESIAN_POINT('Ctrl Pts',(0.709398700781977,0.337917579445235,
-1.06817007372281));
#34820=CARTESIAN_POINT('Ctrl Pts',(0.466642216044095,0.632203019823103,
-1.05773611112033));
#34821=CARTESIAN_POINT('Ctrl Pts',(0.113892415079302,0.777472895144444,
-1.04730214851785));
#34822=CARTESIAN_POINT('Ctrl Pts',(-0.265702207996828,0.739484780514238,
-1.03686818591537));
#34823=CARTESIAN_POINT('Ctrl Pts',(-0.582668673968479,0.527193314268239,
-1.02643422331289));
#34824=CARTESIAN_POINT('Ctrl Pts',(-0.762294477768732,0.190637345373093,
-1.01600026071041));
#34825=CARTESIAN_POINT('Ctrl Pts',(-0.76224039792685,-0.190853595901271,
-1.00556629810792));
#34826=CARTESIAN_POINT('Ctrl Pts',(-0.58251904484713,-0.527358571859844,
-0.995132335505447));
#34827=CARTESIAN_POINT('Ctrl Pts',(-0.265492500386351,-0.739560164195111,
-0.984698372902963));
#34828=CARTESIAN_POINT('Ctrl Pts',(0.114113134053,-0.777440479167041,-0.974264410300485));
#34829=CARTESIAN_POINT('Ctrl Pts',(0.466821224039013,-0.632070762133705,
-0.963830447698002));
#34830=CARTESIAN_POINT('Ctrl Pts',(0.709495166277289,-0.337716026159997,
-0.953396485095523));
#34831=CARTESIAN_POINT('Ctrl Pts',(0.784934426712147,0.036241552574442,
-0.942962522493043));
#34832=CARTESIAN_POINT('Ctrl Pts',(0.675357264853418,0.401656656313797,
-0.932528559890561));
#34833=CARTESIAN_POINT('Ctrl Pts',(0.406592046625541,0.672397510606692,
-0.922094597288082));
#34834=CARTESIAN_POINT('Ctrl Pts',(0.0419892610781143,0.784647950737612,
-0.911660634685599));
#34835=CARTESIAN_POINT('Ctrl Pts',(-0.332510788126124,0.711949492909918,
-0.901226672083121));
#34836=CARTESIAN_POINT('Ctrl Pts',(-0.628634918776022,0.47143784695666,
-0.890792709480638));
#34837=CARTESIAN_POINT('Ctrl Pts',(-0.776583889666874,0.119803868775785,
-0.880358746878159));
#34838=CARTESIAN_POINT('Ctrl Pts',(-0.741484737537109,-0.260069007488211,
-0.869924784275677));
#34839=CARTESIAN_POINT('Ctrl Pts',(-0.531610662510997,-0.578641173926874,
-0.859490821673197));
#34840=CARTESIAN_POINT('Ctrl Pts',(-0.196430956965558,-0.760822176204229,
-0.849056859070717));
#34841=CARTESIAN_POINT('Ctrl Pts',(0.185049371667793,-0.763670239503633,
-0.838622896468236));
#34842=CARTESIAN_POINT('Ctrl Pts',(0.522911823858683,-0.586514048533684,
-0.828188933865755));
#34843=CARTESIAN_POINT('Ctrl Pts',(0.737519043576373,-0.271110982847447,
-0.817754971263275));
#34844=CARTESIAN_POINT('Ctrl Pts',(0.778286091736729,0.108195490052141,
-0.807321008660794));
#34845=CARTESIAN_POINT('Ctrl Pts',(0.63560379186074,0.46199926886376,-0.796887046058315));
#34846=CARTESIAN_POINT('Ctrl Pts',(0.343103703302493,0.70690547701834,-0.786453083455833));
#34847=CARTESIAN_POINT('Ctrl Pts',(-0.0302691534421004,0.785187419033389,
-0.776019120853353));
#34848=CARTESIAN_POINT('Ctrl Pts',(-0.396507286177706,0.678393305293029,
-0.765585158250871));
#34849=CARTESIAN_POINT('Ctrl Pts',(-0.669284924227368,0.411695512315087,
-0.755151195648392));
#34850=CARTESIAN_POINT('Ctrl Pts',(-0.784305814079195,0.0479572169749487,
-0.74471723304591));
#34851=CARTESIAN_POINT('Ctrl Pts',(-0.714458450750784,-0.327085045224027,
-0.734283270443431));
#34852=CARTESIAN_POINT('Ctrl Pts',(-0.47620651437298,-0.625030287527851,
-0.723849307840949));
#34853=CARTESIAN_POINT('Ctrl Pts',(-0.125708226017614,-0.775650015515966,
-0.713415345238469));
#34854=CARTESIAN_POINT('Ctrl Pts',(0.254420672919862,-0.743441743413307,
-0.702981382635988));
#34855=CARTESIAN_POINT('Ctrl Pts',(0.574580227589684,-0.535997263725664,
-0.692547420033508));
#34856=CARTESIAN_POINT('Ctrl Pts',(0.75930582132283,-0.202213190380046,
-0.682113457431026));
#34857=CARTESIAN_POINT('Ctrl Pts',(0.765055895178765,0.17923443282648,-0.671679494828547));
#34858=CARTESIAN_POINT('Ctrl Pts',(0.59047510269656,0.518434815337377,-0.661245532226065));
#34859=CARTESIAN_POINT('Ctrl Pts',(0.276713777796529,0.73543523836976,-0.650811569623586));
#34860=CARTESIAN_POINT('Ctrl Pts',(-0.102271585755068,0.77908666232041,
-0.640377607021104));
#34861=CARTESIAN_POINT('Ctrl Pts',(-0.457150575148634,0.639100036222566,
-0.629943644418625));
#34862=CARTESIAN_POINT('Ctrl Pts',(-0.70427487657359,0.348471523780162,
-0.619509681816143));
#34863=CARTESIAN_POINT('Ctrl Pts',(-0.785394969112564,-0.0242950025948932,
-0.609075719213664));
#34864=CARTESIAN_POINT('Ctrl Pts',(-0.681390084391421,-0.391334968475175,
-0.598641756611182));
#34865=CARTESIAN_POINT('Ctrl Pts',(-0.416775151428224,-0.666133603573932,
-0.588207794008702));
#34866=CARTESIAN_POINT('Ctrl Pts',(-0.0539223974131412,-0.783918286376605,
-0.577773831406221));
#34867=CARTESIAN_POINT('Ctrl Pts',(0.321640372565246,-0.716926059921455,
-0.567339868803741));
#34868=CARTESIAN_POINT('Ctrl Pts',(0.62138948317635,-0.480947621738835,
-0.55690590620126));
#34869=CARTESIAN_POINT('Ctrl Pts',(0.774671251282472,-0.131605308004129,
-0.546471943598779));
#34870=CARTESIAN_POINT('Ctrl Pts',(0.745355723228448,0.248757613971936,
-0.536037980996299));
#34871=CARTESIAN_POINT('Ctrl Pts',(0.540352844554801,0.57048602790949,-0.525604018393818));
#34872=CARTESIAN_POINT('Ctrl Pts',(0.207983720877477,0.757745522262172,
-0.515170055791338));
#34873=CARTESIAN_POINT('Ctrl Pts',(-0.173409120944393,0.766397273893708,
-0.504736093188856));
#34874=CARTESIAN_POINT('Ctrl Pts',(-0.513927802841605,0.594401983614464,
-0.494302130586377));
#34875=CARTESIAN_POINT('Ctrl Pts',(-0.733308870473353,0.282300558170737,
-0.483868167983895));
#34876=CARTESIAN_POINT('Ctrl Pts',(-0.779842143925295,-0.0963417625768395,
-0.473434205381416));
#34877=CARTESIAN_POINT('Ctrl Pts',(-0.642559293212633,-0.452275424232272,
-0.463000242778934));
#34878=CARTESIAN_POINT('Ctrl Pts',(-0.353819176764386,-0.701603516818599,
-0.452566280176454));
#34879=CARTESIAN_POINT('Ctrl Pts',(0.0183194456950479,-0.785557065124962,
-0.442132317573973));
#34880=CARTESIAN_POINT('Ctrl Pts',(0.386140002593756,-0.68434742861757,
-0.431698354971493));
#34881=CARTESIAN_POINT('Ctrl Pts',(0.662943731003984,-0.421830670033247,
-0.421264392369012));
#34882=CARTESIAN_POINT('Ctrl Pts',(0.7834853900691,-0.0598844571388489,
-0.410830429766532));
#34883=CARTESIAN_POINT('Ctrl Pts',(0.719352177605274,0.316177085244017,
-0.400396467164051));
#34884=CARTESIAN_POINT('Ctrl Pts',(0.485660894669788,0.617712716434524,
-0.38996250456157));
#34885=CARTESIAN_POINT('Ctrl Pts',(0.13749477344486,0.773647653611852,-0.37952854195909));
#34886=CARTESIAN_POINT('Ctrl Pts',(-0.243080158387662,0.747226566207262,
-0.369094579356609));
#34887=CARTESIAN_POINT('Ctrl Pts',(-0.566358811836438,0.544677152935719,
-0.358660616754129));
#34888=CARTESIAN_POINT('Ctrl Pts',(-0.756141369320212,0.213742214466813,
-0.348226654151648));
#34889=CARTESIAN_POINT('Ctrl Pts',(-0.767694298022977,-0.167573773103754,
-0.337792691549167));
#34890=CARTESIAN_POINT('Ctrl Pts',(-0.598294464011491,-0.509391047315,-0.327358728946686));
#34891=CARTESIAN_POINT('Ctrl Pts',(-0.28787100066151,-0.731140062743844,
-0.316924766344206));
#34892=CARTESIAN_POINT('Ctrl Pts',(0.0904063637433995,-0.780552493232092,
-0.306490803741726));
#34893=CARTESIAN_POINT('Ctrl Pts',(0.447374098176336,-0.645981361835213,
-0.296056841139245));
#34894=CARTESIAN_POINT('Ctrl Pts',(0.698891552520447,-0.359146354327081,
-0.285622878536764));
#34895=CARTESIAN_POINT('Ctrl Pts',(0.785673697365901,0.0123428316480947,
-0.275188915934284));
#34896=CARTESIAN_POINT('Ctrl Pts',(0.687265167454291,0.380922683136212,
-0.264754953331803));
#34897=CARTESIAN_POINT('Ctrl Pts',(0.42686177429362,0.65971550303675,-0.254320990729322));
#34898=CARTESIAN_POINT('Ctrl Pts',(0.0658430535679694,0.783007126777559,
-0.243887028126842));
#34899=CARTESIAN_POINT('Ctrl Pts',(-0.310695504294148,0.721736709503349,
-0.233453065524361));
#34900=CARTESIAN_POINT('Ctrl Pts',(-0.614000190546954,0.490345969652942,
-0.223019102921881));
#34901=CARTESIAN_POINT('Ctrl Pts',(-0.772579300526886,0.143376460042316,
-0.2125851403194));
#34902=CARTESIAN_POINT('Ctrl Pts',(-0.749054127115351,-0.237388986095505,
-0.20215117771692));
#34903=CARTESIAN_POINT('Ctrl Pts',(-0.548970011334125,-0.562198126842394,
-0.191717215114439));
#34904=CARTESIAN_POINT('Ctrl Pts',(-0.219488194761954,-0.754494815860368,
-0.181283252511959));
#34905=CARTESIAN_POINT('Ctrl Pts',(0.161728445419113,-0.768944215087351,
-0.170849289909478));
#34906=CARTESIAN_POINT('Ctrl Pts',(0.504825365157434,-0.602157589282083,
-0.160415327306997));
#34907=CARTESIAN_POINT('Ctrl Pts',(0.728927854200643,-0.29341438785622,
-0.149981364704517));
#34908=CARTESIAN_POINT('Ctrl Pts',(0.781219769114282,0.0844450113192067,
-0.139547402102036));
#34909=CARTESIAN_POINT('Ctrl Pts',(0.649362332362858,0.442490652619712,
-0.129113439499555));
#34910=CARTESIAN_POINT('Ctrl Pts',(0.459423217828217,0.611507106016669,
-0.122157464431235));
#34911=CARTESIAN_POINT('Ctrl Pts',(0.350107198737617,0.668737795639028,
-0.118679476897075));
#34912=CARTESIAN_POINT('Ctrl Pts',(-0.740853004920359,-0.114506834660721,
-1.13671995863906));
#34913=CARTESIAN_POINT('Ctrl Pts',(-0.722134886980705,-0.235612041726607,
-1.1332419711049));
#34914=CARTESIAN_POINT('Ctrl Pts',(-0.624218812318237,-0.468354692822251,
-1.12628599603658));
#34915=CARTESIAN_POINT('Ctrl Pts',(-0.330004563367695,-0.707155702503664,
-1.1158520334341));
#34916=CARTESIAN_POINT('Ctrl Pts',(0.0419121041683271,-0.779235354142126,
-1.10541807083161));
#34917=CARTESIAN_POINT('Ctrl Pts',(0.40399000002701,-0.667660918672005,
-1.09498410822914));
#34918=CARTESIAN_POINT('Ctrl Pts',(0.670823328245096,-0.398702898627244,
-1.08455014562665));
#34919=CARTESIAN_POINT('Ctrl Pts',(0.779547608102049,-0.0357717483197776,
-1.07411618302417));
#34920=CARTESIAN_POINT('Ctrl Pts',(0.704519947383164,0.335593624574011,
-1.06368222042169));
#34921=CARTESIAN_POINT('Ctrl Pts',(0.463432975704643,0.627855162501341,
-1.05324825781921));
#34922=CARTESIAN_POINT('Ctrl Pts',(0.113109141693867,0.772125978326591,
-1.04281429521673));
#34923=CARTESIAN_POINT('Ctrl Pts',(-0.26387489246471,0.734399116602389,
-1.03238033261425));
#34924=CARTESIAN_POINT('Ctrl Pts',(-0.578661483474972,0.523567645181706,
-1.02194637001177));
#34925=CARTESIAN_POINT('Ctrl Pts',(-0.757051945540773,0.189326273808813,
-1.01151240740929));
#34926=CARTESIAN_POINT('Ctrl Pts',(-0.756998237707173,-0.18954103724319,
-1.00107844480681));
#34927=CARTESIAN_POINT('Ctrl Pts',(-0.578512883273854,-0.523731765804213,
-0.99064448220433));
#34928=CARTESIAN_POINT('Ctrl Pts',(-0.263666627302358,-0.734473982814123,
-0.980210519601847));
#34929=CARTESIAN_POINT('Ctrl Pts',(0.113328343147265,-0.772093783330432,
-0.969776556999367));
#34930=CARTESIAN_POINT('Ctrl Pts',(0.463610751763097,-0.627723818257463,
-0.959342594396887));
#34931=CARTESIAN_POINT('Ctrl Pts',(0.704615751113342,-0.335393449806213,
-0.948908631794406));
#34932=CARTESIAN_POINT('Ctrl Pts',(0.779536192689487,0.0359923083399053,
-0.938474669191926));
#34933=CARTESIAN_POINT('Ctrl Pts',(0.670712626473464,0.398894340692951,
-0.928040706589444));
#34934=CARTESIAN_POINT('Ctrl Pts',(0.403795788817699,0.66777322736188,-0.917606743986965));
#34935=CARTESIAN_POINT('Ctrl Pts',(0.0417004880928141,0.779251686898004,
-0.907172781384483));
#34936=CARTESIAN_POINT('Ctrl Pts',(-0.33022400978122,0.707053198590567,
-0.896738818782004));
#34937=CARTESIAN_POINT('Ctrl Pts',(-0.624311604253702,0.468195624755374,
-0.886304856179521));
#34938=CARTESIAN_POINT('Ctrl Pts',(-0.771243084840896,0.118979940943888,
-0.875870893577043));
#34939=CARTESIAN_POINT('Ctrl Pts',(-0.736385320310804,-0.258280433415597,
-0.865436930974559));
#34940=CARTESIAN_POINT('Ctrl Pts',(-0.527954613461226,-0.574661681671945,
-0.855002968372082));
#34941=CARTESIAN_POINT('Ctrl Pts',(-0.195080041221753,-0.755589769500391,
-0.844569005769599));
#34942=CARTESIAN_POINT('Ctrl Pts',(0.183776730565653,-0.758418245797768,
-0.83413504316712));
#34943=CARTESIAN_POINT('Ctrl Pts',(0.519315599381725,-0.582480412113205,
-0.823701080564639));
#34944=CARTESIAN_POINT('Ctrl Pts',(0.73244689963983,-0.269246469734522,
-0.813267117962159));
#34945=CARTESIAN_POINT('Ctrl Pts',(0.772933580346709,0.107451396589594,
-0.802833155359677));
#34946=CARTESIAN_POINT('Ctrl Pts',(0.631232550267715,0.458821958649651,
-0.792399192757197));
#34947=CARTESIAN_POINT('Ctrl Pts',(0.340744074241428,0.702043871938179,
-0.781965230154717));
#34948=CARTESIAN_POINT('Ctrl Pts',(-0.0300609832200121,0.779787445105681,
-0.771531267552235));
#34949=CARTESIAN_POINT('Ctrl Pts',(-0.393780384350698,0.673727787134545,
-0.761097304949757));
#34950=CARTESIAN_POINT('Ctrl Pts',(-0.664682047190082,0.408864156413597,
-0.750663342347273));
#34951=CARTESIAN_POINT('Ctrl Pts',(-0.778911903218281,0.047627400532361,
-0.740229379744795));
#34952=CARTESIAN_POINT('Ctrl Pts',(-0.709544901561173,-0.324835581371782,
-0.729795417142313));
#34953=CARTESIAN_POINT('Ctrl Pts',(-0.472931496588075,-0.620731763156647,
-0.719361454539833));
#34954=CARTESIAN_POINT('Ctrl Pts',(-0.124843692115849,-0.770315633228017,
-0.708927491937352));
#34955=CARTESIAN_POINT('Ctrl Pts',(0.252670944170861,-0.738328867259302,
-0.698493529334872));
#34956=CARTESIAN_POINT('Ctrl Pts',(0.570628663704237,-0.532311046678269,
-0.688059566732391));
#34957=CARTESIAN_POINT('Ctrl Pts',(0.754083843055084,-0.20082250844931,
-0.677625604129911));
#34958=CARTESIAN_POINT('Ctrl Pts',(0.759794371895204,0.178001782836491,
-0.667191641527429));
#34959=CARTESIAN_POINT('Ctrl Pts',(0.586414224895629,0.51486938061673,-0.65675767892495));
#34960=CARTESIAN_POINT('Ctrl Pts',(0.274810732549857,0.730377425398683,
-0.646323716322469));
#34961=CARTESIAN_POINT('Ctrl Pts',(-0.101568232793424,0.773728645161738,
-0.635889753719988));
#34962=CARTESIAN_POINT('Ctrl Pts',(-0.454006610883545,0.634704749888194,
-0.625455791117507));
#34963=CARTESIAN_POINT('Ctrl Pts',(-0.699431362936911,0.346074978576626,
-0.615021828515027));
#34964=CARTESIAN_POINT('Ctrl Pts',(-0.779993567799511,-0.0241279184345948,
-0.604587865912546));
#34965=CARTESIAN_POINT('Ctrl Pts',(-0.676703956466903,-0.388643638258286,
-0.594153903310066));
#34966=CARTESIAN_POINT('Ctrl Pts',(-0.41390886129561,-0.661552399132199,
-0.583719940707585));
#34967=CARTESIAN_POINT('Ctrl Pts',(-0.053551556601009,-0.778527040662177,
-0.573285978105104));
#34968=CARTESIAN_POINT('Ctrl Pts',(0.319428353391418,-0.711995540229181,
-0.562852015502625));
#34969=CARTESIAN_POINT('Ctrl Pts',(0.617115997729736,-0.477639997909126,
-0.552418052900142));
#34970=CARTESIAN_POINT('Ctrl Pts',(0.769343600255384,-0.130700218066691,
-0.541984090297663));
#34971=CARTESIAN_POINT('Ctrl Pts',(0.740229684050112,0.247046831810627,
-0.531550127695182));
#34972=CARTESIAN_POINT('Ctrl Pts',(0.536636672846459,0.566562621086918,
-0.521116165092702));
#34973=CARTESIAN_POINT('Ctrl Pts',(0.206553353244347,0.752534274648081,
-0.51068220249022));
#34974=CARTESIAN_POINT('Ctrl Pts',(-0.172216533405129,0.761126525538637,
-0.500248239887741));
#34975=CARTESIAN_POINT('Ctrl Pts',(-0.510393364223772,0.59031409945294,
-0.489814277285259));
#34976=CARTESIAN_POINT('Ctrl Pts',(-0.728265681184372,0.280359090927444,
-0.479380314682779));
#34977=CARTESIAN_POINT('Ctrl Pts',(-0.77447893108866,-0.0956791908220543,
-0.468946352080298));
#34978=CARTESIAN_POINT('Ctrl Pts',(-0.638140216510379,-0.449164987870463,
-0.458512389477818));
#34979=CARTESIAN_POINT('Ctrl Pts',(-0.351385854116396,-0.696778374939642,
-0.448078426875337));
#34980=CARTESIAN_POINT('Ctrl Pts',(0.0181934572663925,-0.780154549028075,
-0.437644464272857));
#34981=CARTESIAN_POINT('Ctrl Pts',(0.383484399745436,-0.679640962132693,
-0.427210501670376));
#34982=CARTESIAN_POINT('Ctrl Pts',(0.658384464291117,-0.418929611553615,
-0.416776539067896));
#34983=CARTESIAN_POINT('Ctrl Pts',(0.778097121514928,-0.0594726134192682,
-0.406342576465414));
#34984=CARTESIAN_POINT('Ctrl Pts',(0.714404972759968,0.314002638767335,
-0.395908613862934));
#34985=CARTESIAN_POINT('Ctrl Pts',(0.482320856221212,0.613464517236842,
-0.385474651260454));
#34986=CARTESIAN_POINT('Ctrl Pts',(0.136549179853027,0.768327042178898,
-0.375040688657973));
#34987=CARTESIAN_POINT('Ctrl Pts',(-0.241408421824046,0.74208766066977,
-0.364606726055492));
#34988=CARTESIAN_POINT('Ctrl Pts',(-0.562463789140705,0.540931241636695,
-0.354172763453012));
#34989=CARTESIAN_POINT('Ctrl Pts',(-0.750941153956061,0.21227224391263,
-0.343738800850531));
#34990=CARTESIAN_POINT('Ctrl Pts',(-0.762414629636959,-0.166421317035261,
-0.333304838248051));
#34991=CARTESIAN_POINT('Ctrl Pts',(-0.59417981007126,-0.505887809352505,
-0.32287087564557));
#34992=CARTESIAN_POINT('Ctrl Pts',(-0.2858912237842,-0.726111789007469,
-0.312436913043089));
#34993=CARTESIAN_POINT('Ctrl Pts',(0.0897846115448619,-0.77518439510846,
-0.302002950440609));
#34994=CARTESIAN_POINT('Ctrl Pts',(0.444297369724562,-0.641538750516217,
-0.291568987838128));
#34995=CARTESIAN_POINT('Ctrl Pts',(0.694085061664183,-0.356676395059487,
-0.281135025235648));
#34996=CARTESIAN_POINT('Ctrl Pts',(0.780270379123696,0.0122579462393452,
-0.270701062633167));
#34997=CARTESIAN_POINT('Ctrl Pts',(0.682538634845947,0.378302961353538,
-0.260267100030687));
#34998=CARTESIAN_POINT('Ctrl Pts',(0.423926115256723,0.655178437904007,
-0.249833137428206));
#34999=CARTESIAN_POINT('Ctrl Pts',(0.0653902309856967,0.777622147249573,
-0.239399174825725));
#35000=CARTESIAN_POINT('Ctrl Pts',(-0.308558756771405,0.716773105772152,
-0.228965212223245));
#35001=CARTESIAN_POINT('Ctrl Pts',(-0.60977752264731,0.486973709982111,
-0.218531249620764));
#35002=CARTESIAN_POINT('Ctrl Pts',(-0.767266038211421,0.142390417335117,
-0.208097287018284));
#35003=CARTESIAN_POINT('Ctrl Pts',(-0.743902649484968,-0.235756391513122,
-0.197663324415803));
#35004=CARTESIAN_POINT('Ctrl Pts',(-0.545194583421681,-0.558331714416402,
-0.187229361813323));
#35005=CARTESIAN_POINT('Ctrl Pts',(-0.217978694187387,-0.749305932283897,
-0.176795399210842));
#35006=CARTESIAN_POINT('Ctrl Pts',(0.160616163563403,-0.763655935021635,
-0.166361436608361));
#35007=CARTESIAN_POINT('Ctrl Pts',(0.501353577761108,-0.59801639819482,
-0.155927474005881));
#35008=CARTESIAN_POINT('Ctrl Pts',(0.723914693935939,-0.291396426753068,
-0.1454935114034));
#35009=CARTESIAN_POINT('Ctrl Pts',(0.775847282725173,0.0838641360470627,
-0.135059548800919));
#35010=CARTESIAN_POINT('Ctrl Pts',(0.644896041046783,0.439447767297551,
-0.124625586198439));
#35011=CARTESIAN_POINT('Ctrl Pts',(0.45626430167519,0.607301174227473,-0.117669611130118));
#35012=CARTESIAN_POINT('Ctrl Pts',(0.347699381636261,0.66413863770549,-0.114191623595958));
#35013=CARTESIAN_POINT('Ctrl Pts',(-0.738728321778978,-0.114178441930233,
-1.13006310830201));
#35014=CARTESIAN_POINT('Ctrl Pts',(-0.720064366806754,-0.234933217536769,
-1.12658512076785));
#35015=CARTESIAN_POINT('Ctrl Pts',(-0.622428042508284,-0.467013310191975,
-1.11962914569953));
#35016=CARTESIAN_POINT('Ctrl Pts',(-0.329058258071164,-0.705126571760288,
-1.10919518309705));
#35017=CARTESIAN_POINT('Ctrl Pts',(0.0417919924060089,-0.777000845426073,
-1.09876122049457));
#35018=CARTESIAN_POINT('Ctrl Pts',(0.402831247473459,-0.66574573944522,
-1.08832725789209));
#35019=CARTESIAN_POINT('Ctrl Pts',(0.668899333621666,-0.39755947669164,
-1.0778932952896));
#35020=CARTESIAN_POINT('Ctrl Pts',(0.777311738081329,-0.0356690904367907,
-1.06745933268712));
#35021=CARTESIAN_POINT('Ctrl Pts',(0.702499287124512,0.334631062607015,
-1.05702537008464));
#35022=CARTESIAN_POINT('Ctrl Pts',(0.462103778469495,0.626054396882013,
-1.04659140748216));
#35023=CARTESIAN_POINT('Ctrl Pts',(0.112784729733038,0.769911399718677,
-1.03615744487968));
#35024=CARTESIAN_POINT('Ctrl Pts',(-0.263118061333202,0.73229275590801,
-1.0257234822772));
#35025=CARTESIAN_POINT('Ctrl Pts',(-0.577001796823257,0.522065974186607,
-1.01528951967472));
#35026=CARTESIAN_POINT('Ctrl Pts',(-0.754880609472423,0.188783259239166,
-1.00485555707224));
#35027=CARTESIAN_POINT('Ctrl Pts',(-0.754827055346662,-0.188997406198555,
-0.994421594469758));
#35028=CARTESIAN_POINT('Ctrl Pts',(-0.576853623322529,-0.522229625831565,
-0.98398763186728));
#35029=CARTESIAN_POINT('Ctrl Pts',(-0.262910392619021,-0.732367403574915,
-0.973553669264797));
#35030=CARTESIAN_POINT('Ctrl Pts',(0.113003300781567,-0.769879304770086,
-0.963119706662317));
#35031=CARTESIAN_POINT('Ctrl Pts',(0.462281047969412,-0.625923414086446,
-0.952685744059838));
#35032=CARTESIAN_POINT('Ctrl Pts',(0.702594809534997,-0.334431492061369,
-0.942251781457356));
#35033=CARTESIAN_POINT('Ctrl Pts',(0.777300368274831,0.0358890770986708,
-0.931817818854876));
#35034=CARTESIAN_POINT('Ctrl Pts',(0.668788924044225,0.397750253078562,
-0.921383856252395));
#35035=CARTESIAN_POINT('Ctrl Pts',(0.402637643125386,0.665857955560156,
-0.910949893649915));
#35036=CARTESIAN_POINT('Ctrl Pts',(0.0415808849614458,0.777016678487022,
-0.900515931047433));
#35037=CARTESIAN_POINT('Ctrl Pts',(-0.329276878767882,0.705025266057697,
-0.890081968444954));
#35038=CARTESIAN_POINT('Ctrl Pts',(-0.622520986779629,0.466852770864623,
-0.879648005842472));
#35039=CARTESIAN_POINT('Ctrl Pts',(-0.76903104627692,0.118638688979371,
-0.869214043239993));
#35040=CARTESIAN_POINT('Ctrl Pts',(-0.734273258940723,-0.25753964715726,
-0.858780080637511));
#35041=CARTESIAN_POINT('Ctrl Pts',(-0.526440362004133,-0.573013467475887,
-0.848346118035031));
#35042=CARTESIAN_POINT('Ctrl Pts',(-0.194520522980727,-0.753422626946348,
-0.837912155432551));
#35043=CARTESIAN_POINT('Ctrl Pts',(0.183249631881523,-0.756242990757862,
-0.82747819283007));
#35044=CARTESIAN_POINT('Ctrl Pts',(0.517826125887222,-0.5808097726486,-0.81704423022759));
#35045=CARTESIAN_POINT('Ctrl Pts',(0.730346134239288,-0.268474231271757,
-0.806610267625109));
#35046=CARTESIAN_POINT('Ctrl Pts',(0.770716693193102,0.107143210185493,
-0.796176305022628));
#35047=CARTESIAN_POINT('Ctrl Pts',(0.629422082502815,0.457505989811206,
-0.785742342420148));
#35048=CARTESIAN_POINT('Ctrl Pts',(0.339766770136572,0.700030306891271,
-0.775308379817667));
#35049=CARTESIAN_POINT('Ctrl Pts',(-0.0299747639002413,0.777550900060215,
-0.764874417215186));
#35050=CARTESIAN_POINT('Ctrl Pts',(-0.392650964310469,0.671795436782195,
-0.754440454612705));
#35051=CARTESIAN_POINT('Ctrl Pts',(-0.662775641349895,0.407691473897311,
-0.744006492010225));
#35052=CARTESIAN_POINT('Ctrl Pts',(-0.77667786935568,0.0474907981449312,
-0.733572529407744));
#35053=CARTESIAN_POINT('Ctrl Pts',(-0.707509822458421,-0.323903905163518,
-0.723138566805264));
#35054=CARTESIAN_POINT('Ctrl Pts',(-0.471575059520285,-0.618951413193123,
-0.712704604202783));
#35055=CARTESIAN_POINT('Ctrl Pts',(-0.124485622050972,-0.768106254731665,
-0.702270641600303));
#35056=CARTESIAN_POINT('Ctrl Pts',(0.251946246752525,-0.736211231510794,
-0.691836678997822));
#35057=CARTESIAN_POINT('Ctrl Pts',(0.568992016796649,-0.530784300330188,
-0.681402716395341));
#35058=CARTESIAN_POINT('Ctrl Pts',(0.751921019719524,-0.200246519967949,
-0.670968753792861));
#35059=CARTESIAN_POINT('Ctrl Pts',(0.757615169923306,0.177491247551542,
-0.66053479119038));
#35060=CARTESIAN_POINT('Ctrl Pts',(0.584732302677578,0.513392659531377,
-0.650100828587899));
#35061=CARTESIAN_POINT('Ctrl Pts',(0.274022534963215,0.728282595554539,
-0.639666865985419));
#35062=CARTESIAN_POINT('Ctrl Pts',(-0.101276920168097,0.771509477645342,
-0.629232903382938));
#35063=CARTESIAN_POINT('Ctrl Pts',(-0.452704453170499,0.632884323344261,
-0.618798940780458));
#35064=CARTESIAN_POINT('Ctrl Pts',(-0.697425290949937,0.345082384654329,
-0.608364978177976));
#35065=CARTESIAN_POINT('Ctrl Pts',(-0.777756431563853,-0.0240587160169735,
-0.597931015575498));
#35066=CARTESIAN_POINT('Ctrl Pts',(-0.674763070023318,-0.38752895116111,
-0.587497052973015));
#35067=CARTESIAN_POINT('Ctrl Pts',(-0.412721709823994,-0.659654969582799,
-0.577063090370536));
#35068=CARTESIAN_POINT('Ctrl Pts',(-0.0533979628629402,-0.776294110641973,
-0.566629127768054));
#35069=CARTESIAN_POINT('Ctrl Pts',(0.318512185908032,-0.709953432334411,
-0.556195165165574));
#35070=CARTESIAN_POINT('Ctrl Pts',(0.615346018313083,-0.476270056167252,
-0.545761202563093));
#35071=CARTESIAN_POINT('Ctrl Pts',(0.767137009692518,-0.130325350624296,
-0.535327239960613));
#35072=CARTESIAN_POINT('Ctrl Pts',(0.738106596479569,0.246338265173459,
-0.524893277358132));
#35073=CARTESIAN_POINT('Ctrl Pts',(0.535097519966526,0.564937636187391,
-0.514459314755652));
#35074=CARTESIAN_POINT('Ctrl Pts',(0.205960927857503,0.750375895702546,
-0.504025352153171));
#35075=CARTESIAN_POINT('Ctrl Pts',(-0.171722591066159,0.758943502754224,
-0.49359138955069));
#35076=CARTESIAN_POINT('Ctrl Pts',(-0.508929481011548,0.588620991821254,
-0.48315742694821));
#35077=CARTESIAN_POINT('Ctrl Pts',(-0.726176908133127,0.279554979833196,
-0.47272346434573));
#35078=CARTESIAN_POINT('Ctrl Pts',(-0.772257611641912,-0.0954047688349727,
-0.462289501743249));
#35079=CARTESIAN_POINT('Ctrl Pts',(-0.636309936543053,-0.447876716644087,
-0.451855539140769));
#35080=CARTESIAN_POINT('Ctrl Pts',(-0.350378027822189,-0.694779912112316,
-0.441421576538287));
#35081=CARTESIAN_POINT('Ctrl Pts',(0.0181412757559533,-0.777916951074585,
-0.430987613935807));
#35082=CARTESIAN_POINT('Ctrl Pts',(0.382384510102879,-0.677691651925025,
-0.420553651333326));
#35083=CARTESIAN_POINT('Ctrl Pts',(0.656496120844634,-0.417728059832058,
-0.410119688730846));
#35084=CARTESIAN_POINT('Ctrl Pts',(0.775865424566033,-0.059302037219655,
-0.399685726128365));
#35085=CARTESIAN_POINT('Ctrl Pts',(0.712355954258472,0.313102033031217,
-0.389251763525884));
#35086=CARTESIAN_POINT('Ctrl Pts',(0.480937489089399,0.611705010803167,
-0.378817800923404));
#35087=CARTESIAN_POINT('Ctrl Pts',(0.136157536728385,0.76612336725398,-0.368383838320924));
#35088=CARTESIAN_POINT('Ctrl Pts',(-0.240716026976006,0.739959244149261,
-0.357949875718442));
#35089=CARTESIAN_POINT('Ctrl Pts',(-0.560850560293331,0.539379771301723,
-0.347515913115962));
#35090=CARTESIAN_POINT('Ctrl Pts',(-0.748787344315938,0.211663415907114,
-0.337081950513481));
#35091=CARTESIAN_POINT('Ctrl Pts',(-0.760227912378577,-0.165943996230135,
-0.326647987911001));
#35092=CARTESIAN_POINT('Ctrl Pts',(-0.592475615017121,-0.504436848731709,
-0.316214025308521));
#35093=CARTESIAN_POINT('Ctrl Pts',(-0.285071245711697,-0.724029193640397,
-0.30578006270604));
#35094=CARTESIAN_POINT('Ctrl Pts',(0.0895270960624317,-0.772961052277889,
-0.295346100103559));
#35095=CARTESIAN_POINT('Ctrl Pts',(0.443023059573026,-0.639698723071951,
-0.284912137501079));
#35096=CARTESIAN_POINT('Ctrl Pts',(0.692094323595697,-0.355653394680012,
-0.274478174898598));
#35097=CARTESIAN_POINT('Ctrl Pts',(0.77803244906981,0.0122227885764535,
-0.264044212296118));
#35098=CARTESIAN_POINT('Ctrl Pts',(0.680581013455972,0.377217932977406,
-0.253610249693636));
#35099=CARTESIAN_POINT('Ctrl Pts',(0.422710233282305,0.653299289538504,
-0.243176287091156));
#35100=CARTESIAN_POINT('Ctrl Pts',(0.0652026812946639,0.775391813136047,
-0.232742324488675));
#35101=CARTESIAN_POINT('Ctrl Pts',(-0.307673763129735,0.714717294055676,
-0.222308361886195));
#35102=CARTESIAN_POINT('Ctrl Pts',(-0.608028594518627,0.485576999870044,
-0.211874399283715));
#35103=CARTESIAN_POINT('Ctrl Pts',(-0.765065399588571,0.141982016572898,
-0.201440436681234));
#35104=CARTESIAN_POINT('Ctrl Pts',(-0.741769040716881,-0.235080199432113,
-0.191006474078753));
#35105=CARTESIAN_POINT('Ctrl Pts',(-0.543630858812939,-0.556730352880329,
-0.180572511476273));
#35106=CARTESIAN_POINT('Ctrl Pts',(-0.217353551159869,-0.747156781385138,
-0.170138548873792));
#35107=CARTESIAN_POINT('Ctrl Pts',(0.16015559496067,-0.761465719142782,
-0.159704586271311));
#35108=CARTESIAN_POINT('Ctrl Pts',(0.499915420847107,-0.596301077920999,
-0.149270623668831));
#35109=CARTESIAN_POINT('Ctrl Pts',(0.721838796965714,-0.290560898293607,
-0.13883666106635));
#35110=CARTESIAN_POINT('Ctrl Pts',(0.773621246330564,0.0836240792666152,
-0.12840269846387));
#35111=CARTESIAN_POINT('Ctrl Pts',(0.643048073335996,0.438186347774578,
-0.117968735861389));
#35112=CARTESIAN_POINT('Ctrl Pts',(0.454952994195837,0.605560964824544,
-0.111012760793069));
#35113=CARTESIAN_POINT('Ctrl Pts',(0.346702218893416,0.662233962746084,
-0.107534773258908));
#35114=CARTESIAN_POINT('Ctrl Pts',(-0.738728321778978,-0.114178441930233,
-1.12625));
#35115=CARTESIAN_POINT('Ctrl Pts',(-0.720064014057805,-0.23493549980332,
-1.12277201246584));
#35116=CARTESIAN_POINT('Ctrl Pts',(-0.622428467720143,-0.467011987146764,
-1.11581603739752));
#35117=CARTESIAN_POINT('Ctrl Pts',(-0.329058176975965,-0.705127368582219,
-1.10538207479504));
#35118=CARTESIAN_POINT('Ctrl Pts',(0.0417919283474094,-0.777000661774149,
-1.09494811219256));
#35119=CARTESIAN_POINT('Ctrl Pts',(0.402831360764579,-0.665746034504356,
-1.08451414959008));
#35120=CARTESIAN_POINT('Ctrl Pts',(0.668899442574653,-0.397559467050135,
-1.0740801869876));
#35121=CARTESIAN_POINT('Ctrl Pts',(0.777311895666571,-0.0356691406410416,
-1.06364622438512));
#35122=CARTESIAN_POINT('Ctrl Pts',(0.702499416237836,0.334631148448012,
-1.05321226178264));
#35123=CARTESIAN_POINT('Ctrl Pts',(0.46210386898375,0.626054505003765,-1.04277829918015));
#35124=CARTESIAN_POINT('Ctrl Pts',(0.112784749994036,0.769911552166375,
-1.03234433657768));
#35125=CARTESIAN_POINT('Ctrl Pts',(-0.26311811085717,0.732292892594134,
-1.02191037397519));
#35126=CARTESIAN_POINT('Ctrl Pts',(-0.577001907123836,0.522066075167687,
-1.01147641137271));
#35127=CARTESIAN_POINT('Ctrl Pts',(-0.75488075319647,0.188783294475201,
-1.00104244877023));
#35128=CARTESIAN_POINT('Ctrl Pts',(-0.754827199305277,-0.188997441843081,
-0.990608486167751));
#35129=CARTESIAN_POINT('Ctrl Pts',(-0.576853733233578,-0.522229725565815,
-0.980174523565273));
#35130=CARTESIAN_POINT('Ctrl Pts',(-0.262910442753167,-0.732367543071951,
-0.969740560962789));
#35131=CARTESIAN_POINT('Ctrl Pts',(0.113003322331734,-0.769879451565163,
-0.959306598360312));
#35132=CARTESIAN_POINT('Ctrl Pts',(0.462281136078415,-0.62592353336717,
-0.948872635757828));
#35133=CARTESIAN_POINT('Ctrl Pts',(0.702594943458043,-0.334431555819591,
-0.938438673155349));
#35134=CARTESIAN_POINT('Ctrl Pts',(0.777300516433143,0.0358890839459625,
-0.928004710552868));
#35135=CARTESIAN_POINT('Ctrl Pts',(0.668789051521523,0.397750328889649,
-0.917570747950388));
#35136=CARTESIAN_POINT('Ctrl Pts',(0.402637719871008,0.665858082479754,
-0.907136785347906));
#35137=CARTESIAN_POINT('Ctrl Pts',(0.0415808928872853,0.777016826591823,
-0.896702822745427));
#35138=CARTESIAN_POINT('Ctrl Pts',(-0.329276941530812,0.705025400441648,
-0.886268860142945));
#35139=CARTESIAN_POINT('Ctrl Pts',(-0.622521105437113,0.466852859850312,
-0.875834897540466));
#35140=CARTESIAN_POINT('Ctrl Pts',(-0.769031192860478,0.118638711592977,
-0.865400934937984));
#35141=CARTESIAN_POINT('Ctrl Pts',(-0.73427339889913,-0.257539696246457,
-0.854966972335505));
#35142=CARTESIAN_POINT('Ctrl Pts',(-0.526440462347927,-0.573013576696855,
-0.844533009733022));
#35143=CARTESIAN_POINT('Ctrl Pts',(-0.194520560057907,-0.753422770554806,
-0.834099047130545));
#35144=CARTESIAN_POINT('Ctrl Pts',(0.183249666810382,-0.75624313490388,
-0.823665084528061));
#35145=CARTESIAN_POINT('Ctrl Pts',(0.517826224589069,-0.580809883355642,
-0.813231121925582));
#35146=CARTESIAN_POINT('Ctrl Pts',(0.730346273449163,-0.268474282445113,
-0.802797159323101));
#35147=CARTESIAN_POINT('Ctrl Pts',(0.770716840097934,0.107143230607854,
-0.79236319672062));
#35148=CARTESIAN_POINT('Ctrl Pts',(0.629422202475751,0.457506077015547,
-0.781929234118141));
#35149=CARTESIAN_POINT('Ctrl Pts',(0.339766834898865,0.700030440322704,
-0.771495271515659));
#35150=CARTESIAN_POINT('Ctrl Pts',(-0.0299747696136733,0.777551048267703,
-0.76106130891318));
#35151=CARTESIAN_POINT('Ctrl Pts',(-0.392651039152918,0.671795564831834,
-0.750627346310697));
#35152=CARTESIAN_POINT('Ctrl Pts',(-0.662775767680288,0.407691551606601,
-0.740193383708218));
#35153=CARTESIAN_POINT('Ctrl Pts',(-0.776678017396761,0.0474908071970611,
-0.729759421105736));
#35154=CARTESIAN_POINT('Ctrl Pts',(-0.707509957315512,-0.32390396690222,
-0.719325458503256));
#35155=CARTESIAN_POINT('Ctrl Pts',(-0.471575149406303,-0.618951531170265,
-0.708891495900776));
#35156=CARTESIAN_POINT('Ctrl Pts',(-0.124485645778937,-0.768106401138927,
-0.698457533298295));
#35157=CARTESIAN_POINT('Ctrl Pts',(0.251946294775516,-0.736211371838605,
-0.688023570695814));
#35158=CARTESIAN_POINT('Ctrl Pts',(0.568992125251126,-0.530784401501965,
-0.677589608093334));
#35159=CARTESIAN_POINT('Ctrl Pts',(0.751921163041749,-0.200246558136555,
-0.667155645490853));
#35160=CARTESIAN_POINT('Ctrl Pts',(0.757615314330881,0.177491281382809,
-0.656721682888373));
#35161=CARTESIAN_POINT('Ctrl Pts',(0.584732414132281,0.513392757388168,
-0.646287720285892));
#35162=CARTESIAN_POINT('Ctrl Pts',(0.274022587194125,0.728282734371089,
-0.635853757683411));
#35163=CARTESIAN_POINT('Ctrl Pts',(-0.101276939472296,0.771509624701284,
-0.625419795080931));
#35164=CARTESIAN_POINT('Ctrl Pts',(-0.452704539459628,0.632884443977129,
-0.61498583247845));
#35165=CARTESIAN_POINT('Ctrl Pts',(-0.697425423884835,0.34508245042982,
-0.60455186987597));
#35166=CARTESIAN_POINT('Ctrl Pts',(-0.777756579810516,-0.0240587206027588,
-0.594117907273489));
#35167=CARTESIAN_POINT('Ctrl Pts',(-0.674763198638613,-0.387529025027261,
-0.583683944671008));
#35168=CARTESIAN_POINT('Ctrl Pts',(-0.412721788492088,-0.659655095318368,
-0.573249982068528));
#35169=CARTESIAN_POINT('Ctrl Pts',(-0.0533979730410232,-0.776294258609905,
-0.562816019466047));
#35170=CARTESIAN_POINT('Ctrl Pts',(0.318512246619028,-0.709953567657274,
-0.552382056863567));
#35171=CARTESIAN_POINT('Ctrl Pts',(0.615346135603009,-0.476270146948173,
-0.541948094261086));
#35172=CARTESIAN_POINT('Ctrl Pts',(0.767137155915032,-0.130325375465362,
-0.531514131658606));
#35173=CARTESIAN_POINT('Ctrl Pts',(0.738106737168653,0.246338312127524,
-0.521080169056125));
#35174=CARTESIAN_POINT('Ctrl Pts',(0.535097621960438,0.56493774386907,-0.510646206453644));
#35175=CARTESIAN_POINT('Ctrl Pts',(0.20596096711532,0.750376038730258,-0.500212243851164));
#35176=CARTESIAN_POINT('Ctrl Pts',(-0.171722623797873,0.758943647414989,
-0.489778281248683));
#35177=CARTESIAN_POINT('Ctrl Pts',(-0.50892957801762,0.588621104017174,
-0.479344318646202));
#35178=CARTESIAN_POINT('Ctrl Pts',(-0.726177046548315,0.279555033118634,
-0.468910356043722));
#35179=CARTESIAN_POINT('Ctrl Pts',(-0.772257758840454,-0.0954047870198923,
-0.458476393441241));
#35180=CARTESIAN_POINT('Ctrl Pts',(-0.636310057828871,-0.44787680201301,
-0.448042430838761));
#35181=CARTESIAN_POINT('Ctrl Pts',(-0.350378094607072,-0.694780044542982,
-0.43760846823628));
#35182=CARTESIAN_POINT('Ctrl Pts',(0.0181412792138254,-0.777917099351843,
-0.4271745056338));
#35183=CARTESIAN_POINT('Ctrl Pts',(0.382384582988461,-0.677691781098534,
-0.416740543031318));
#35184=CARTESIAN_POINT('Ctrl Pts',(0.656496245978095,-0.417728139454399,
-0.406306580428839));
#35185=CARTESIAN_POINT('Ctrl Pts',(0.775865572452267,-0.0593020485231105,
-0.395872617826357));
#35186=CARTESIAN_POINT('Ctrl Pts',(0.71235609003925,0.313102092711011,-0.385438655223877));
#35187=CARTESIAN_POINT('Ctrl Pts',(0.480937580760022,0.611705127399056,
-0.375004692621396));
#35188=CARTESIAN_POINT('Ctrl Pts',(0.136157562681014,0.766123513283346,
-0.364570730018916));
#35189=CARTESIAN_POINT('Ctrl Pts',(-0.240716072858233,0.739959385191357,
-0.354136767416435));
#35190=CARTESIAN_POINT('Ctrl Pts',(-0.560850667196364,0.539379874112098,
-0.343702804813955));
#35191=CARTESIAN_POINT('Ctrl Pts',(-0.748787487040106,0.211663456251418,
-0.333268842211474));
#35192=CARTESIAN_POINT('Ctrl Pts',(-0.760228057285642,-0.165944027859509,
-0.322834879608993));
#35193=CARTESIAN_POINT('Ctrl Pts',(-0.592475727944849,-0.504436944883207,
-0.312400917006513));
#35194=CARTESIAN_POINT('Ctrl Pts',(-0.285071300054314,-0.724029331642755,
-0.301966954404032));
#35195=CARTESIAN_POINT('Ctrl Pts',(0.0895271131383019,-0.772961199617318,
-0.291532991801552));
#35196=CARTESIAN_POINT('Ctrl Pts',(0.443023143994601,-0.639698844990308,
-0.281099029199071));
#35197=CARTESIAN_POINT('Ctrl Pts',(0.692094455558156,-0.355653462496774,
-0.27066506659659));
#35198=CARTESIAN_POINT('Ctrl Pts',(0.778032597283115,0.0122227909580681,
-0.26023110399411));
#35199=CARTESIAN_POINT('Ctrl Pts',(0.680581143349384,0.377218004776158,
-0.249797141391629));
#35200=CARTESIAN_POINT('Ctrl Pts',(0.422710313521399,0.653299414263413,
-0.239363178789149));
#35201=CARTESIAN_POINT('Ctrl Pts',(0.0652026943778876,0.775391960536891,
-0.228929216186668));
#35202=CARTESIAN_POINT('Ctrl Pts',(-0.307673823063876,0.714717431064052,
-0.218495253584187));
#35203=CARTESIAN_POINT('Ctrl Pts',(-0.608028707877235,0.485577090895019,
-0.208061290981707));
#35204=CARTESIAN_POINT('Ctrl Pts',(-0.765065550407644,0.1419820466464,-0.197627328379226));
#35205=CARTESIAN_POINT('Ctrl Pts',(-0.741769172281951,-0.235080250164509,
-0.187193365776746));
#35206=CARTESIAN_POINT('Ctrl Pts',(-0.543630981761309,-0.556730447339977,
-0.176759403174265));
#35207=CARTESIAN_POINT('Ctrl Pts',(-0.217353554555294,-0.747156946739445,
-0.166325440571784));
#35208=CARTESIAN_POINT('Ctrl Pts',(0.160155550638919,-0.761465819139253,
-0.155891477969304));
#35209=CARTESIAN_POINT('Ctrl Pts',(0.499915663487151,-0.59630128045638,
-0.145457515366823));
#35210=CARTESIAN_POINT('Ctrl Pts',(0.721838643854921,-0.290560778341041,
-0.135023552764343));
#35211=CARTESIAN_POINT('Ctrl Pts',(0.773621974230802,0.0836237451066752,
-0.124589590161862));
#35212=CARTESIAN_POINT('Ctrl Pts',(0.643046958594177,0.438187177596506,
-0.114155627559381));
#35213=CARTESIAN_POINT('Ctrl Pts',(0.454955040136648,0.605559893704277,
-0.107199652491061));
#35214=CARTESIAN_POINT('Ctrl Pts',(0.346702218893416,0.662233962746084,
-0.103721664956901));
#35215=CARTESIAN_POINT('',(0.351283760559811,0.670985139773177,-0.12));
#35216=CARTESIAN_POINT('Ctrl Pts',(0.708746600204741,0.237559480337495,
-0.12));
#35217=CARTESIAN_POINT('Ctrl Pts',(0.677871308579869,0.329674339059907,
-0.12));
#35218=CARTESIAN_POINT('Ctrl Pts',(0.630004482514663,0.414923577124779,
-0.12));
#35219=CARTESIAN_POINT('Ctrl Pts',(0.488745407170187,0.583538685988183,
-0.12));
#35220=CARTESIAN_POINT('Ctrl Pts',(0.404572366318542,0.639316291073142,
-0.12));
#35221=CARTESIAN_POINT('Ctrl Pts',(0.35128376055981,0.670985139773177,-0.12));
#35222=CARTESIAN_POINT('Ctrl Pts',(-0.459745842892902,-0.601806928197395,
-1.12625));
#35223=CARTESIAN_POINT('Ctrl Pts',(-0.416468302643127,-0.63488822608401,
-1.12472013661271));
#35224=CARTESIAN_POINT('Ctrl Pts',(-0.263250172568346,-0.728042154867832,
-1.11971228569126));
#35225=CARTESIAN_POINT('Ctrl Pts',(0.0423441932323986,-0.787268438306115,
-1.11122644723566));
#35226=CARTESIAN_POINT('Ctrl Pts',(0.408154628293017,-0.674543622261519,
-1.10079248463318));
#35227=CARTESIAN_POINT('Ctrl Pts',(0.677738701453828,-0.402813068451861,
-1.0903585220307));
#35228=CARTESIAN_POINT('Ctrl Pts',(0.787583785039379,-0.0361404951497401,
-1.07992455942821));
#35229=CARTESIAN_POINT('Ctrl Pts',(0.711782686348953,0.339053175380463,
-1.06949059682573));
#35230=CARTESIAN_POINT('Ctrl Pts',(0.468210400798597,0.634327583870302,
-1.05905663422325));
#35231=CARTESIAN_POINT('Ctrl Pts',(0.114275158775038,0.780085648735316,
-1.04862267162077));
#35232=CARTESIAN_POINT('Ctrl Pts',(-0.266595119432202,0.74196987248233,
-1.03818870901829));
#35233=CARTESIAN_POINT('Ctrl Pts',(-0.584626774041373,0.528964985372604,
-1.02775474641581));
#35234=CARTESIAN_POINT('Ctrl Pts',(-0.764856223313065,0.19127799592914,
-1.01732078381333));
#35235=CARTESIAN_POINT('Ctrl Pts',(-0.764801961726996,-0.191494973175329,
-1.00688682121085));
#35236=CARTESIAN_POINT('Ctrl Pts',(-0.584476642087926,-0.529130798350251,
-0.99645285860837));
#35237=CARTESIAN_POINT('Ctrl Pts',(-0.266384707070968,-0.742045509438616,
-0.98601889600589));
#35238=CARTESIAN_POINT('Ctrl Pts',(0.114496619465385,-0.780053123936526,
-0.975584933403408));
#35239=CARTESIAN_POINT('Ctrl Pts',(0.468390010412392,-0.634194881491942,
-0.965150970800929));
#35240=CARTESIAN_POINT('Ctrl Pts',(0.711879475926064,-0.338850945209237,
-0.954717008198448));
#35241=CARTESIAN_POINT('Ctrl Pts',(0.787572255433587,0.0363633449241354,
-0.944283045595968));
#35242=CARTESIAN_POINT('Ctrl Pts',(0.677626851623736,0.403006452460033,
-0.933849082993486));
#35243=CARTESIAN_POINT('Ctrl Pts',(0.407958428506616,0.674657150909495,
-0.923415120391007));
#35244=CARTESIAN_POINT('Ctrl Pts',(0.042130369016677,0.787284816735879,
-0.912981157788525));
#35245=CARTESIAN_POINT('Ctrl Pts',(-0.333628214598003,0.714342050500304,
-0.902547195186045));
#35246=CARTESIAN_POINT('Ctrl Pts',(-0.630747491734475,0.473022147824027,
-0.892113232583564));
#35247=CARTESIAN_POINT('Ctrl Pts',(-0.779193655806613,0.120206478312629,
-0.881679269981084));
#35248=CARTESIAN_POINT('Ctrl Pts',(-0.743976550446063,-0.260942988134434,
-0.871245307378604));
#35249=CARTESIAN_POINT('Ctrl Pts',(-0.533397178462468,-0.58058573930206,
-0.860811344776122));
#35250=CARTESIAN_POINT('Ctrl Pts',(-0.197091077355777,-0.763378973969726,
-0.850377382173643));
#35251=CARTESIAN_POINT('Ctrl Pts',(0.185671243420201,-0.766236608391142,
-0.83994341957116));
#35252=CARTESIAN_POINT('Ctrl Pts',(0.524669106735824,-0.588485071271487,
-0.829509456968682));
#35253=CARTESIAN_POINT('Ctrl Pts',(0.739997529484913,-0.272022070847804,
-0.819075494366199));
#35254=CARTESIAN_POINT('Ctrl Pts',(0.780901578249222,0.108559088795519,
-0.80864153176372));
#35255=CARTESIAN_POINT('Ctrl Pts',(0.637739784219531,0.46355185070908,-0.798207569161239));
#35256=CARTESIAN_POINT('Ctrl Pts',(0.344256728029392,0.709281083829744,
-0.787773606558758));
#35257=CARTESIAN_POINT('Ctrl Pts',(-0.0303708751141343,0.787826097953732,
-0.777339643956278));
#35258=CARTESIAN_POINT('Ctrl Pts',(-0.397839777494349,0.680673094896106,
-0.766905681353797));
#35259=CARTESIAN_POINT('Ctrl Pts',(-0.671534104459313,0.413079044760479,
-0.756471718751317));
#35260=CARTESIAN_POINT('Ctrl Pts',(-0.786941530302541,0.0481183806594935,
-0.746037756148835));
#35261=CARTESIAN_POINT('Ctrl Pts',(-0.716859439874856,-0.32818423809578,
-0.735603793546356));
#35262=CARTESIAN_POINT('Ctrl Pts',(-0.477806840690935,-0.627130746863161,
-0.725169830943874));
#35263=CARTESIAN_POINT('Ctrl Pts',(-0.126130677572575,-0.778256643304304,
-0.714735868341395));
#35264=CARTESIAN_POINT('Ctrl Pts',(0.25527567193062,-0.745940132981574,
-0.704301905738912));
#35265=CARTESIAN_POINT('Ctrl Pts',(0.576511145861978,-0.537798521166717,
-0.693867943136434));
#35266=CARTESIAN_POINT('Ctrl Pts',(0.761857523268443,-0.202892742382455,
-0.683433980533952));
#35267=CARTESIAN_POINT('Ctrl Pts',(0.767626920662054,0.179836763057753,
-0.673000017931472));
#35268=CARTESIAN_POINT('Ctrl Pts',(0.5924594368424,0.520177052904666,-0.662566055328991));
#35269=CARTESIAN_POINT('Ctrl Pts',(0.277643694393179,0.737906721500696,
-0.652132092726511));
#35270=CARTESIAN_POINT('Ctrl Pts',(-0.102615276791043,0.781704839208058,
-0.64169813012403));
#35271=CARTESIAN_POINT('Ctrl Pts',(-0.458686862609216,0.641247777962555,
-0.631264167521549));
#35272=CARTESIAN_POINT('Ctrl Pts',(-0.706641643062577,0.349642587454705,
-0.620830204919069));
#35273=CARTESIAN_POINT('Ctrl Pts',(-0.78803434551991,-0.0243766477023704,
-0.610396242316588));
#35274=CARTESIAN_POINT('Ctrl Pts',(-0.683679944886674,-0.392650077845343,
-0.599962279714107));
#35275=CARTESIAN_POINT('Ctrl Pts',(-0.418175754367012,-0.668372193565666,
-0.589528317111627));
#35276=CARTESIAN_POINT('Ctrl Pts',(-0.0541036075165375,-0.786552700285172,
-0.579094354509147));
#35277=CARTESIAN_POINT('Ctrl Pts',(0.322721268222062,-0.719335341624019,
-0.568660391906665));
#35278=CARTESIAN_POINT('Ctrl Pts',(0.623477707326195,-0.482563880889846,
-0.558226429304185));
#35279=CARTESIAN_POINT('Ctrl Pts',(0.777274589863052,-0.132047577128186,
-0.547792466701704));
#35280=CARTESIAN_POINT('Ctrl Pts',(0.747860544863849,0.24959358186489,-0.537358504099224));
#35281=CARTESIAN_POINT('Ctrl Pts',(0.542168739239194,0.572403187328635,
-0.526924541496743));
#35282=CARTESIAN_POINT('Ctrl Pts',(0.208682665163581,0.760291980710322,
-0.516490578894263));
#35283=CARTESIAN_POINT('Ctrl Pts',(-0.17399187479518,0.768972807176858,
-0.506056616291782));
#35284=CARTESIAN_POINT('Ctrl Pts',(-0.515654894268523,0.596399514326692,
-0.495622653689302));
#35285=CARTESIAN_POINT('Ctrl Pts',(-0.735773207791699,0.283249249545548,
-0.485188691086821));
#35286=CARTESIAN_POINT('Ctrl Pts',(-0.782462859663334,-0.0966655260145846,
-0.47475472848434));
#35287=CARTESIAN_POINT('Ctrl Pts',(-0.64471866003509,-0.453795328396784,
-0.46432076588186));
#35288=CARTESIAN_POINT('Ctrl Pts',(-0.355008211612258,-0.703961306010569,
-0.453886803279379));
#35289=CARTESIAN_POINT('Ctrl Pts',(0.0183810095128271,-0.788196986267641,
-0.443452840676899));
#35290=CARTESIAN_POINT('Ctrl Pts',(0.38743765390661,-0.686647227481269,
-0.433018878074418));
#35291=CARTESIAN_POINT('Ctrl Pts',(0.665171601199011,-0.423248262406725,
-0.422584915471937));
#35292=CARTESIAN_POINT('Ctrl Pts',(0.786118349198421,-0.0600857031737155,
-0.412150952869457));
#35293=CARTESIAN_POINT('Ctrl Pts',(0.721769612451196,0.317239621129978,
-0.401716990266976));
#35294=CARTESIAN_POINT('Ctrl Pts',(0.48729299311423,0.619788584544703,-0.391283027664495));
#35295=CARTESIAN_POINT('Ctrl Pts',(0.137956834542062,0.776247552318673,
-0.380849065062015));
#35296=CARTESIAN_POINT('Ctrl Pts',(-0.24389704678188,0.749737674945354,
-0.370415102459534));
#35297=CARTESIAN_POINT('Ctrl Pts',(-0.568262101448461,0.54650757977013,
-0.359981139857054));
#35298=CARTESIAN_POINT('Ctrl Pts',(-0.758682436896782,0.214460510585722,
-0.349547177254573));
#35299=CARTESIAN_POINT('Ctrl Pts',(-0.770274190049179,-0.168136916847512,
-0.339113214652093));
#35300=CARTESIAN_POINT('Ctrl Pts',(-0.600305075684733,-0.511102892647913,
-0.328679252049612));
#35301=CARTESIAN_POINT('Ctrl Pts',(-0.288838411909729,-0.73359711162755,
-0.318245289447131));
#35302=CARTESIAN_POINT('Ctrl Pts',(0.0907101808452941,-0.783175596150043,
-0.307811326844651));
#35303=CARTESIAN_POINT('Ctrl Pts',(0.448877531081785,-0.648152228766222,
-0.29737736424217));
#35304=CARTESIAN_POINT('Ctrl Pts',(0.70124022796002,-0.360353291538616,
-0.286943401639689));
#35305=CARTESIAN_POINT('Ctrl Pts',(0.78831401046138,0.0123843106225018,
-0.276509439037209));
#35306=CARTESIAN_POINT('Ctrl Pts',(0.689574771586232,0.382202801273025,
-0.266075476434728));
#35307=CARTESIAN_POINT('Ctrl Pts',(0.42829627406239,0.661932524534907,-0.255641513832248));
#35308=CARTESIAN_POINT('Ctrl Pts',(0.0660643238823282,0.785638478676651,
-0.245207551229767));
#35309=CARTESIAN_POINT('Ctrl Pts',(-0.311739618905983,0.724162157724785,
-0.234773588627286));
#35310=CARTESIAN_POINT('Ctrl Pts',(-0.616063582497866,0.491993812660696,
-0.224339626024806));
#35311=CARTESIAN_POINT('Ctrl Pts',(-0.775175608854641,0.143858286910066,
-0.213905663422325));
#35312=CARTESIAN_POINT('Ctrl Pts',(-0.751571377703373,-0.238186748774504,
-0.203471700819845));
#35313=CARTESIAN_POINT('Ctrl Pts',(-0.550814864235531,-0.564087434409687,
-0.193037738217364));
#35314=CARTESIAN_POINT('Ctrl Pts',(-0.220225801435375,-0.757030349608765,
-0.182603775614884));
#35315=CARTESIAN_POINT('Ctrl Pts',(0.162271947040125,-0.771528308468155,
-0.172169813012403));
#35316=CARTESIAN_POINT('Ctrl Pts',(0.50652186418947,-0.604181181458613,
-0.161735850409922));
#35317=CARTESIAN_POINT('Ctrl Pts',(0.731377474710374,-0.294400431622865,
-0.151301887807442));
#35318=CARTESIAN_POINT('Ctrl Pts',(0.783845102655791,0.0847288019872719,
-0.140867925204961));
#35319=CARTESIAN_POINT('Ctrl Pts',(0.651544586453759,0.443977659175325,
-0.130433962602481));
#35320=CARTESIAN_POINT('Ctrl Pts',(0.460967102820801,0.613562143858194,
-0.12347798753416));
#35321=CARTESIAN_POINT('Ctrl Pts',(0.35128376055981,0.670985139773177,-0.12));
#35322=CARTESIAN_POINT('Ctrl Pts',(-0.495956409719265,-0.649207665313755,
-1.15727273924394));
#35323=CARTESIAN_POINT('Ctrl Pts',(-0.388302693694881,-0.731448762184642,
-1.15374460067508));
#35324=CARTESIAN_POINT('Ctrl Pts',(-0.13140455693268,-0.841265750467438,
-1.14668832353737));
#35325=CARTESIAN_POINT('Ctrl Pts',(0.286034174319602,-0.801958781222045,
-1.1361039078308));
#35326=CARTESIAN_POINT('Ctrl Pts',(0.634034477218437,-0.568280999134343,
-1.12551949212423));
#35327=CARTESIAN_POINT('Ctrl Pts',(0.828384689818385,-0.196826841568886,
-1.11493507641766));
#35328=CARTESIAN_POINT('Ctrl Pts',(0.821897829369206,0.222332451391628,
-1.10435066071109));
#35329=CARTESIAN_POINT('Ctrl Pts',(0.616183750099589,0.587599496275833,
-1.09376624500451));
#35330=CARTESIAN_POINT('Ctrl Pts',(0.261091496307317,0.810421806269904,
-1.08318182929794));
#35331=CARTESIAN_POINT('Ctrl Pts',(-0.157289815040412,0.836787381022574,
-1.07259741359137));
#35332=CARTESIAN_POINT('Ctrl Pts',(-0.537543482173721,0.660303137862947,
-1.0620129978848));
#35333=CARTESIAN_POINT('Ctrl Pts',(-0.7874880639875,0.323752245535046,-1.05142858217823));
#35334=CARTESIAN_POINT('Ctrl Pts',(-0.846534688677586,-0.0912809764781306,
-1.04084416647166));
#35335=CARTESIAN_POINT('Ctrl Pts',(-0.700368959446377,-0.484186307032688,
-1.03025975076509));
#35336=CARTESIAN_POINT('Ctrl Pts',(-0.38442387329105,-0.759717979177561,
-1.01967533505852));
#35337=CARTESIAN_POINT('Ctrl Pts',(0.0247111232736773,-0.851083110906004,
-1.00909091935195));
#35338=CARTESIAN_POINT('Ctrl Pts',(0.42785576069194,-0.736133514901142,
-0.998506503645377));
#35339=CARTESIAN_POINT('Ctrl Pts',(0.727282047487868,-0.442734604895683,
-0.987922087938807));
#35340=CARTESIAN_POINT('Ctrl Pts',(0.850404740342968,-0.0420104871635215,
-0.977337672232236));
#35341=CARTESIAN_POINT('Ctrl Pts',(0.767377146099821,0.368897575755567,
-0.966753256525664));
#35342=CARTESIAN_POINT('Ctrl Pts',(0.498326337204486,0.690379581274127,
-0.956168840819095));
#35343=CARTESIAN_POINT('Ctrl Pts',(0.108474086749781,0.844503687104731,
-0.945584425112522));
#35344=CARTESIAN_POINT('Ctrl Pts',(-0.307673836701548,0.793908001690772,
-0.935000009405953));
#35345=CARTESIAN_POINT('Ctrl Pts',(-0.649237214524841,0.550857644208324,
-0.924415593699381));
#35346=CARTESIAN_POINT('Ctrl Pts',(-0.833416191506255,0.174271502818131,
-0.913831177992811));
#35347=CARTESIAN_POINT('Ctrl Pts',(-0.815563145108209,-0.244560547230945,
-0.90324676228624));
#35348=CARTESIAN_POINT('Ctrl Pts',(-0.600005909618337,-0.604107617370174,
-0.892662346579669));
#35349=CARTESIAN_POINT('Ctrl Pts',(-0.238998646675454,-0.817210347352623,
-0.882077930873097));
#35350=CARTESIAN_POINT('Ctrl Pts',(0.17994531181254,-0.832209582792671,
-0.871493515166529));
#35351=CARTESIAN_POINT('Ctrl Pts',(0.555267949047113,-0.64546929415458,
-0.860909099459956));
#35352=CARTESIAN_POINT('Ctrl Pts',(0.795985681346874,-0.302258002417496,
-0.850324683753387));
#35353=CARTESIAN_POINT('Ctrl Pts',(0.843745082180559,0.114224958881187,
-0.839740268046815));
#35354=CARTESIAN_POINT('Ctrl Pts',(0.686968588642089,0.503018153901045,
-0.829155852340245));
#35355=CARTESIAN_POINT('Ctrl Pts',(0.363661068552687,0.769872542797965,
-0.818571436633673));
#35356=CARTESIAN_POINT('Ctrl Pts',(-0.047803103913807,0.850098799076459,
-0.807987020927103));
#35357=CARTESIAN_POINT('Ctrl Pts',(-0.447679119223231,0.724248928992339,
-0.797402605220532));
#35358=CARTESIAN_POINT('Ctrl Pts',(-0.739031303134287,0.422830743823914,
-0.786818189513961));
#35359=CARTESIAN_POINT('Ctrl Pts',(-0.85123171271497,0.0189123294010521,
-0.776233773807391));
#35360=CARTESIAN_POINT('Ctrl Pts',(-0.757081361438328,-0.389590704583327,
-0.765649358100819));
#35361=CARTESIAN_POINT('Ctrl Pts',(-0.479403643135562,-0.703651370980965,
-0.755064942394249));
#35362=CARTESIAN_POINT('Ctrl Pts',(-0.0855116143916565,-0.847136865411472,
-0.744480526687678));
#35363=CARTESIAN_POINT('Ctrl Pts',(0.329109654614668,-0.785264248628737,
-0.733896110981106));
#35364=CARTESIAN_POINT('Ctrl Pts',(0.663950028923553,-0.533032329251663,
-0.723311695274536));
#35365=CARTESIAN_POINT('Ctrl Pts',(0.837839405292465,-0.151585737700515,
-0.712727279567964));
#35366=CARTESIAN_POINT('Ctrl Pts',(0.808624507964925,0.266607408099481,
-0.702142863861395));
#35367=CARTESIAN_POINT('Ctrl Pts',(0.583387446549703,0.620171099087388,
-0.691558448154823));
#35368=CARTESIAN_POINT('Ctrl Pts',(0.216728911202081,0.82339643185054,-0.680974032448252));
#35369=CARTESIAN_POINT('Ctrl Pts',(-0.202467816811898,0.82701867457178,
-0.670389616741683));
#35370=CARTESIAN_POINT('Ctrl Pts',(-0.572583445726543,0.6301597437277,-0.659805201035111));
#35371=CARTESIAN_POINT('Ctrl Pts',(-0.803896645273107,0.280541064113054,
-0.64922078532854));
#35372=CARTESIAN_POINT('Ctrl Pts',(-0.840333782374013,-0.137084788127738,
-0.63863636962197));
#35373=CARTESIAN_POINT('Ctrl Pts',(-0.67306197304253,-0.521479324018831,
-0.628051953915399));
#35374=CARTESIAN_POINT('Ctrl Pts',(-0.342630299990165,-0.779459801698388,
-0.617467538208828));
#35375=CARTESIAN_POINT('Ctrl Pts',(0.0708598658787424,-0.848488057866867,
-0.606883122502257));
#35376=CARTESIAN_POINT('Ctrl Pts',(0.467172585207631,-0.7118306544154,-0.596298706795686));
#35377=CARTESIAN_POINT('Ctrl Pts',(0.750235977744155,-0.402615303525977,
-0.585714291089116));
#35378=CARTESIAN_POINT('Ctrl Pts',(0.851431422320551,0.00419976430822168,
-0.575129875382545));
#35379=CARTESIAN_POINT('Ctrl Pts',(0.746227693570422,0.409996749113464,
-0.564545459675974));
#35380=CARTESIAN_POINT('Ctrl Pts',(0.460127682361612,0.716404648826047,
-0.553961043969404));
#35381=CARTESIAN_POINT('Ctrl Pts',(0.0624861297268952,0.849145799334128,
-0.543376628262831));
#35382=CARTESIAN_POINT('Ctrl Pts',(-0.350302955852819,0.776041844268606,
-0.532792212556262));
#35383=CARTESIAN_POINT('Ctrl Pts',(-0.67817358692588,0.514814229534427,
-0.522207796849691));
#35384=CARTESIAN_POINT('Ctrl Pts',(-0.841645225850065,0.12878827096765,
-0.511623381143119));
#35385=CARTESIAN_POINT('Ctrl Pts',(-0.80109000565714,-0.288457809343551,
-0.501038965436549));
#35386=CARTESIAN_POINT('Ctrl Pts',(-0.566339092665934,-0.635777584579208,
-0.490454549729978));
#35387=CARTESIAN_POINT('Ctrl Pts',(-0.194299470937418,-0.82897576594764,
-0.479870134023407));
#35388=CARTESIAN_POINT('Ctrl Pts',(0.224841125840774,-0.821218346766367,
-0.469285718316837));
#35389=CARTESIAN_POINT('Ctrl Pts',(0.589477012918694,-0.614385836568145,
-0.458701302610266));
#35390=CARTESIAN_POINT('Ctrl Pts',(0.811215227944597,-0.258617398652365,
-0.448116886903695));
#35391=CARTESIAN_POINT('Ctrl Pts',(0.8363032512486,0.159843601330507,-0.437532471197124));
#35392=CARTESIAN_POINT('Ctrl Pts',(0.658659386600812,0.539556222628657,
-0.426948055490553));
#35393=CARTESIAN_POINT('Ctrl Pts',(0.321347051500517,0.788472686544893,
-0.416363639783983));
#35394=CARTESIAN_POINT('Ctrl Pts',(-0.0938644121072648,0.846252076555809,
-0.405779224077412));
#35395=CARTESIAN_POINT('Ctrl Pts',(-0.48632179762979,0.698887840846459,
-0.395194808370841));
#35396=CARTESIAN_POINT('Ctrl Pts',(-0.760887812970069,0.382103181111099,
-0.38461039266427));
#35397=CARTESIAN_POINT('Ctrl Pts',(-0.851003722888249,-0.0273087632644408,
-0.374025976957699));
#35398=CARTESIAN_POINT('Ctrl Pts',(-0.734824139984663,-0.43010067223277,
-0.363441561251128));
#35399=CARTESIAN_POINT('Ctrl Pts',(-0.440512659294738,-0.728630017160833,
-0.352857145544558));
#35400=CARTESIAN_POINT('Ctrl Pts',(-0.0394145998886176,-0.850529008473494,
-0.342272729837987));
#35401=CARTESIAN_POINT('Ctrl Pts',(0.371238123405903,-0.766247584505002,
-0.331688314131416));
#35402=CARTESIAN_POINT('Ctrl Pts',(0.691897407156195,-0.496216769731146,
-0.321103898424845));
#35403=CARTESIAN_POINT('Ctrl Pts',(0.844830849187047,-0.105895901792902,
-0.310519482718274));
#35404=CARTESIAN_POINT('Ctrl Pts',(0.792965189320117,0.310095649688961,
-0.299935067011704));
#35405=CARTESIAN_POINT('Ctrl Pts',(0.548873412549209,0.650915573609104,
-0.289350651305133));
#35406=CARTESIAN_POINT('Ctrl Pts',(0.171726850179941,0.833944238330876,
-0.278766235598562));
#35407=CARTESIAN_POINT('Ctrl Pts',(-0.247048745074761,0.814812873511381,
-0.268181819891991));
#35408=CARTESIAN_POINT('Ctrl Pts',(-0.605936216145871,0.598159196372131,
-0.257597404185421));
#35409=CARTESIAN_POINT('Ctrl Pts',(-0.817936008537478,0.236503161103038,
-0.247012988478849));
#35410=CARTESIAN_POINT('Ctrl Pts',(-0.831656513568513,-0.182484627408237,
-0.236428572772279));
#35411=CARTESIAN_POINT('Ctrl Pts',(-0.643771334910445,-0.557235529878874,
-0.225844157065708));
#35412=CARTESIAN_POINT('Ctrl Pts',(-0.29982721760122,-0.796904554312883,
-0.215259741359137));
#35413=CARTESIAN_POINT('Ctrl Pts',(0.116800205661488,-0.843392505842622,
-0.204675325652567));
#35414=CARTESIAN_POINT('Ctrl Pts',(0.50511183077167,-0.685430019722115,
-0.194090909945995));
#35415=CARTESIAN_POINT('Ctrl Pts',(0.770980560490097,-0.361309503413322,
-0.183506494239425));
#35416=CARTESIAN_POINT('Ctrl Pts',(0.849945784476039,0.0503976618012751,
-0.172922078532854));
#35417=CARTESIAN_POINT('Ctrl Pts',(0.722885284777081,0.449887613677287,
-0.162337662826283));
#35418=CARTESIAN_POINT('Ctrl Pts',(0.42056085792794,0.740318564577236,-0.151753247119712));
#35419=CARTESIAN_POINT('Ctrl Pts',(0.0163382438424028,0.85128520335196,
-0.141168831413141));
#35420=CARTESIAN_POINT('Ctrl Pts',(-0.391950752487246,0.755890089971351,
-0.130584415706571));
#35421=CARTESIAN_POINT('Ctrl Pts',(-0.600629835243707,0.5701228592569,-0.123528138568857));
#35422=CARTESIAN_POINT('Ctrl Pts',(-0.676565692095422,0.457932546695692,
-0.12));
#35423=CARTESIAN_POINT('Ctrl Pts',(-0.483897209295839,-0.633422154331299,
-1.14693182616263));
#35424=CARTESIAN_POINT('Ctrl Pts',(-0.378861097787544,-0.71366355556206,
-1.14340368759377));
#35425=CARTESIAN_POINT('Ctrl Pts',(-0.128209449746748,-0.820810339275165,
-1.13634741045605));
#35426=CARTESIAN_POINT('Ctrl Pts',(0.279079241651182,-0.782459120597521,
-1.12576299474949));
#35427=CARTESIAN_POINT('Ctrl Pts',(0.618617902926218,-0.554463223355893,
-1.11517857904291));
#35428=CARTESIAN_POINT('Ctrl Pts',(0.808242482143577,-0.192040988851441,
-1.10459416333634));
#35429=CARTESIAN_POINT('Ctrl Pts',(0.80191334997201,0.216926428726288,-1.09400974762977));
#35430=CARTESIAN_POINT('Ctrl Pts',(0.601201216968671,0.57331199044784,-1.0834253319232));
#35431=CARTESIAN_POINT('Ctrl Pts',(0.254743045876755,0.790716366844582,
-1.07284091621663));
#35432=CARTESIAN_POINT('Ctrl Pts',(-0.15346530674298,0.816440861566847,
-1.06225650051006));
#35433=CARTESIAN_POINT('Ctrl Pts',(-0.524473090379596,0.644247840010836,
-1.05167208480349));
#35434=CARTESIAN_POINT('Ctrl Pts',(-0.768340259445449,0.315880196419577,
-1.04108766909692));
#35435=CARTESIAN_POINT('Ctrl Pts',(-0.825951163036847,-0.0890614757949581,
-1.03050325339035));
#35436=CARTESIAN_POINT('Ctrl Pts',(-0.683339459500824,-0.47241329713835,
-1.01991883768378));
#35437=CARTESIAN_POINT('Ctrl Pts',(-0.375076591060762,-0.741245405385504,
-1.0093344219772));
#35438=CARTESIAN_POINT('Ctrl Pts',(0.0241102712987759,-0.830388990192415,
-0.998750006270636));
#35439=CARTESIAN_POINT('Ctrl Pts',(0.417452430339941,-0.718234398324306,
-0.988165590564063));
#35440=CARTESIAN_POINT('Ctrl Pts',(0.709598154703862,-0.431969494837229,
-0.977581174857493));
#35441=CARTESIAN_POINT('Ctrl Pts',(0.829727114237416,-0.0409890004468207,
-0.966996759150922));
#35442=CARTESIAN_POINT('Ctrl Pts',(0.748718339350226,0.359927816086022,
-0.956412343444352));
#35443=CARTESIAN_POINT('Ctrl Pts',(0.486209511897153,0.673592973468133,
-0.945827927737781));
#35444=CARTESIAN_POINT('Ctrl Pts',(0.105836534885889,0.823969545350454,
-0.93524351203121));
#35445=CARTESIAN_POINT('Ctrl Pts',(-0.300192734755657,0.774604096100419,
-0.924659096324639));
#35446=CARTESIAN_POINT('Ctrl Pts',(-0.633450985052106,0.537463518018798,
-0.914074680618068));
#35447=CARTESIAN_POINT('Ctrl Pts',(-0.813151642661748,0.170034084086582,
-0.903490264911497));
#35448=CARTESIAN_POINT('Ctrl Pts',(-0.795732693818374,-0.238614047504507,
-0.892905849204926));
#35449=CARTESIAN_POINT('Ctrl Pts',(-0.585416741341586,-0.589418715901377,
-0.882321433498356));
#35450=CARTESIAN_POINT('Ctrl Pts',(-0.233187384788913,-0.797339844272723,
-0.871737017791784));
#35451=CARTESIAN_POINT('Ctrl Pts',(0.175569934182818,-0.811974372688474,
-0.861152602085215));
#35452=CARTESIAN_POINT('Ctrl Pts',(0.541766586114726,-0.629774681820032,
-0.850568186378643));
#35453=CARTESIAN_POINT('Ctrl Pts',(0.776631256890554,-0.294908586704127,
-0.839983770672073));
#35454=CARTESIAN_POINT('Ctrl Pts',(0.823229385936095,0.111447574325788,
-0.829399354965501));
#35455=CARTESIAN_POINT('Ctrl Pts',(0.670264919261704,0.490787246878494,
-0.818814939258932));
#35456=CARTESIAN_POINT('Ctrl Pts',(0.354818634770338,0.75115306037541,-0.808230523552359));
#35457=CARTESIAN_POINT('Ctrl Pts',(-0.0466407694834795,0.829428611945336,
-0.79764610784579));
#35458=CARTESIAN_POINT('Ctrl Pts',(-0.436793783096309,0.70663878660883,
-0.787061692139218));
#35459=CARTESIAN_POINT('Ctrl Pts',(-0.721061726717829,0.412549596962952,
-0.776477276432648));
#35460=CARTESIAN_POINT('Ctrl Pts',(-0.830533978742309,0.0184524753367595,
-0.765892860726077));
#35461=CARTESIAN_POINT('Ctrl Pts',(-0.738672897114632,-0.380117790638464,
-0.755308445019506));
#35462=CARTESIAN_POINT('Ctrl Pts',(-0.467746923909844,-0.686542059064458,
-0.744724029312935));
#35463=CARTESIAN_POINT('Ctrl Pts',(-0.0834323959840071,-0.826538697818774,
-0.734139613606364));
#35464=CARTESIAN_POINT('Ctrl Pts',(0.321107339877917,-0.766170516248254,
-0.723555197899794));
#35465=CARTESIAN_POINT('Ctrl Pts',(0.647806056765878,-0.520071626325674,
-0.712970782193223));
#35466=CARTESIAN_POINT('Ctrl Pts',(0.817467305823512,-0.147899924277319,
-0.702386366486651));
#35467=CARTESIAN_POINT('Ctrl Pts',(0.788962769921528,0.260124838047687,
-0.691801950780082));
#35468=CARTESIAN_POINT('Ctrl Pts',(0.569202356883383,0.605091613402457,
-0.68121753507351));
#35469=CARTESIAN_POINT('Ctrl Pts',(0.211459138846046,0.803375513872608,
-0.67063311936694));
#35470=CARTESIAN_POINT('Ctrl Pts',(-0.197544803550289,0.806909681613664,
-0.660048703660368));
#35471=CARTESIAN_POINT('Ctrl Pts',(-0.558661055782917,0.61483738373907,
-0.649464287953798));
#35472=CARTESIAN_POINT('Ctrl Pts',(-0.784349865404781,0.273719696644377,
-0.638879872247227));
#35473=CARTESIAN_POINT('Ctrl Pts',(-0.819901032024117,-0.133751565887559,
-0.628295456540657));
#35474=CARTESIAN_POINT('Ctrl Pts',(-0.656696443590252,-0.508799532888447,
-0.617711040834085));
#35475=CARTESIAN_POINT('Ctrl Pts',(-0.334299230207119,-0.760507204682845,
-0.607126625127515));
#35476=CARTESIAN_POINT('Ctrl Pts',(0.0691369053365199,-0.827857035974254,
-0.596542209420944));
#35477=CARTESIAN_POINT('Ctrl Pts',(0.455813264656582,-0.69452246288705,
-0.585957793714373));
#35478=CARTESIAN_POINT('Ctrl Pts',(0.731993959205463,-0.392825695924158,
-0.575373378007802));
#35479=CARTESIAN_POINT('Ctrl Pts',(0.830728832400646,0.0040976468669884,
-0.564788962301232));
#35480=CARTESIAN_POINT('Ctrl Pts',(0.728083136625648,0.400027661359743,
-0.55420454659466));
#35481=CARTESIAN_POINT('Ctrl Pts',(0.448939658911917,0.69898524043619,-0.543620130888091));
#35482=CARTESIAN_POINT('Ctrl Pts',(0.060966776922306,0.828498784430789,
-0.533035715181518));
#35483=CARTESIAN_POINT('Ctrl Pts',(-0.341785325128097,0.757172355028014,
-0.522451299474948));
#35484=CARTESIAN_POINT('Ctrl Pts',(-0.661683768372588,0.502296500449523,
-0.511866883768377));
#35485=CARTESIAN_POINT('Ctrl Pts',(-0.821180587698315,0.125656778882156,
-0.501282468061807));
#35486=CARTESIAN_POINT('Ctrl Pts',(-0.781611469346073,-0.281443945890219,
-0.490698052355235));
#35487=CARTESIAN_POINT('Ctrl Pts',(-0.552568534422829,-0.620318626560091,
-0.480113636648665));
#35488=CARTESIAN_POINT('Ctrl Pts',(-0.189575071340432,-0.808819186232531,
-0.469529220942094));
#35489=CARTESIAN_POINT('Ctrl Pts',(0.219374104653414,-0.8012503890165,-0.458944805235523));
#35490=CARTESIAN_POINT('Ctrl Pts',(0.575143855196601,-0.599447019778413,
-0.448360389528952));
#35491=CARTESIAN_POINT('Ctrl Pts',(0.791490496438744,-0.252329106007655,
-0.437775973822382));
#35492=CARTESIAN_POINT('Ctrl Pts',(0.815968503428166,0.155956997614794,
-0.42719155811581));
#35493=CARTESIAN_POINT('Ctrl Pts',(0.64264405662799,0.526436890967901,-0.416607142409241));
#35494=CARTESIAN_POINT('Ctrl Pts',(0.313533484776547,0.769300940865017,
-0.406022726702668));
#35495=CARTESIAN_POINT('Ctrl Pts',(-0.0915820950809177,0.825675422640392,
-0.395438310996099));
#35496=CARTESIAN_POINT('Ctrl Pts',(-0.474496863194084,0.681894354360349,
-0.384853895289527));
#35497=CARTESIAN_POINT('Ctrl Pts',(-0.742386794621416,0.372812326606253,
-0.374269479582957));
#35498=CARTESIAN_POINT('Ctrl Pts',(-0.830311532497566,-0.0266447495667293,
-0.363685063876386));
#35499=CARTESIAN_POINT('Ctrl Pts',(-0.716956860912571,-0.419642756764674,
-0.353100648169815));
#35500=CARTESIAN_POINT('Ctrl Pts',(-0.429801575934612,-0.710913348438998,
-0.342516232463245));
#35501=CARTESIAN_POINT('Ctrl Pts',(-0.0384562322773691,-0.829848360783256,
-0.331931816756673));
#35502=CARTESIAN_POINT('Ctrl Pts',(0.36221145322434,-0.747616243091868,
-0.321347401050103));
#35503=CARTESIAN_POINT('Ctrl Pts',(0.675073893351689,-0.484151238643362,
-0.310762985343532));
#35504=CARTESIAN_POINT('Ctrl Pts',(0.824288752473332,-0.103321038601875,
-0.300178569636961));
#35505=CARTESIAN_POINT('Ctrl Pts',(0.773684208251188,0.30255566126105,-0.28959415393039));
#35506=CARTESIAN_POINT('Ctrl Pts',(0.535527533033774,0.635088534766467,
-0.27900973822382));
#35507=CARTESIAN_POINT('Ctrl Pts',(0.167551304781554,0.813666850006192,
-0.268425322517249));
#35508=CARTESIAN_POINT('Ctrl Pts',(-0.2410417447158,0.795000665106163,-0.257840906810678));
#35509=CARTESIAN_POINT('Ctrl Pts',(-0.591202852222919,0.583614931003628,
-0.247256491104107));
#35510=CARTESIAN_POINT('Ctrl Pts',(-0.798047860976135,0.230752577050439,
-0.236672075397536));
#35511=CARTESIAN_POINT('Ctrl Pts',(-0.811434751365163,-0.17804750621576,
-0.226087659690966));
#35512=CARTESIAN_POINT('Ctrl Pts',(-0.62811800852449,-0.543686325137944,
-0.215503243984394));
#35513=CARTESIAN_POINT('Ctrl Pts',(-0.292536906520256,-0.777527787422745,
-0.204918828277824));
#35514=CARTESIAN_POINT('Ctrl Pts',(0.113960203875109,-0.822885382506262,
-0.194334412571253));
#35515=CARTESIAN_POINT('Ctrl Pts',(0.492830015910225,-0.668763760708061,
-0.183749996864682));
#35516=CARTESIAN_POINT('Ctrl Pts',(0.752234136571959,-0.352524248033688,
-0.173165581158111));
#35517=CARTESIAN_POINT('Ctrl Pts',(0.829279317901195,0.0491722405896055,
-0.162581165451541));
#35518=CARTESIAN_POINT('Ctrl Pts',(0.705308299458539,0.438948577917225,
-0.15199674974497));
#35519=CARTESIAN_POINT('Ctrl Pts',(0.410334903435544,0.72231768834605,-0.141412334038399));
#35520=CARTESIAN_POINT('Ctrl Pts',(0.0159409787739384,0.830586168752268,
-0.130827918331828));
#35521=CARTESIAN_POINT('Ctrl Pts',(-0.3824204538809,0.737510591462186,-0.120243502625258));
#35522=CARTESIAN_POINT('Ctrl Pts',(-0.586025496189812,0.556260298574102,
-0.113187225487544));
#35523=CARTESIAN_POINT('Ctrl Pts',(-0.660114969570814,0.446797898059657,
-0.109659086918687));
#35524=CARTESIAN_POINT('Ctrl Pts',(-0.471838008872413,-0.617636643348843,
-1.13659091308131));
#35525=CARTESIAN_POINT('Ctrl Pts',(-0.369419501880207,-0.695878348939477,
-1.13306277451246));
#35526=CARTESIAN_POINT('Ctrl Pts',(-0.125014342560816,-0.800354928082894,
-1.12600649737474));
#35527=CARTESIAN_POINT('Ctrl Pts',(0.272124308982761,-0.762959459972996,
-1.11542208166817));
#35528=CARTESIAN_POINT('Ctrl Pts',(0.603201328633999,-0.540645447577443,
-1.1048376659616));
#35529=CARTESIAN_POINT('Ctrl Pts',(0.78810027446877,-0.187255136133995,
-1.09425325025503));
#35530=CARTESIAN_POINT('Ctrl Pts',(0.781928870574814,0.211520406060948,
-1.08366883454846));
#35531=CARTESIAN_POINT('Ctrl Pts',(0.586218683837755,0.559024484619848,
-1.07308441884189));
#35532=CARTESIAN_POINT('Ctrl Pts',(0.248394595446193,0.771010927419258,
-1.06250000313532));
#35533=CARTESIAN_POINT('Ctrl Pts',(-0.149640798445549,0.796094342111122,
-1.05191558742875));
#35534=CARTESIAN_POINT('Ctrl Pts',(-0.511402698585469,0.628192542158725,
-1.04133117172218));
#35535=CARTESIAN_POINT('Ctrl Pts',(-0.749192454903402,0.308008147304108,
-1.0307467560156));
#35536=CARTESIAN_POINT('Ctrl Pts',(-0.805367637396107,-0.0868419751117861,
-1.02016234030904));
#35537=CARTESIAN_POINT('Ctrl Pts',(-0.666309959555272,-0.460640287244011,
-1.00957792460246));
#35538=CARTESIAN_POINT('Ctrl Pts',(-0.365729308830473,-0.722772831593449,
-0.998993508895892));
#35539=CARTESIAN_POINT('Ctrl Pts',(0.0235094193238739,-0.809694869478827,
-0.988409093189322));
#35540=CARTESIAN_POINT('Ctrl Pts',(0.407049099987941,-0.70033528174747,
-0.97782467748275));
#35541=CARTESIAN_POINT('Ctrl Pts',(0.691914261919856,-0.421204384778775,
-0.96724026177618));
#35542=CARTESIAN_POINT('Ctrl Pts',(0.809049488131863,-0.0399675137301197,
-0.956655846069608));
#35543=CARTESIAN_POINT('Ctrl Pts',(0.730059532600631,0.350958056416477,
-0.946071430363039));
#35544=CARTESIAN_POINT('Ctrl Pts',(0.474092686589819,0.656806365662141,
-0.935487014656468));
#35545=CARTESIAN_POINT('Ctrl Pts',(0.103198983021998,0.803435403596175,
-0.924902598949896));
#35546=CARTESIAN_POINT('Ctrl Pts',(-0.292711632809765,0.755300190510068,
-0.914318183243327));
#35547=CARTESIAN_POINT('Ctrl Pts',(-0.617664755579371,0.52406939182927,
-0.903733767536755));
#35548=CARTESIAN_POINT('Ctrl Pts',(-0.792887093817242,0.165796665355035,
-0.893149351830185));
#35549=CARTESIAN_POINT('Ctrl Pts',(-0.775902242528537,-0.23266754777807,
-0.882564936123613));
#35550=CARTESIAN_POINT('Ctrl Pts',(-0.570827573064835,-0.574729814432578,
-0.871980520417042));
#35551=CARTESIAN_POINT('Ctrl Pts',(-0.227376122902373,-0.777469341192823,
-0.861396104710471));
#35552=CARTESIAN_POINT('Ctrl Pts',(0.171194556553096,-0.791739162584277,
-0.850811689003902));
#35553=CARTESIAN_POINT('Ctrl Pts',(0.528265223182337,-0.614080069485486,
-0.840227273297329));
#35554=CARTESIAN_POINT('Ctrl Pts',(0.757276832434235,-0.287559170990757,
-0.82964285759076));
#35555=CARTESIAN_POINT('Ctrl Pts',(0.802713689691629,0.108670189770389,
-0.819058441884188));
#35556=CARTESIAN_POINT('Ctrl Pts',(0.653561249881321,0.478556339855944,
-0.808474026177618));
#35557=CARTESIAN_POINT('Ctrl Pts',(0.345976200987988,0.732433577952855,
-0.797889610471047));
#35558=CARTESIAN_POINT('Ctrl Pts',(-0.0454784350531523,0.808758424814214,
-0.787305194764475));
#35559=CARTESIAN_POINT('Ctrl Pts',(-0.425908446969387,0.689028644225321,
-0.776720779057906));
#35560=CARTESIAN_POINT('Ctrl Pts',(-0.703092150301373,0.402268450101991,
-0.766136363351333));
#35561=CARTESIAN_POINT('Ctrl Pts',(-0.809836244769646,0.0179926212724667,
-0.755551947644765));
#35562=CARTESIAN_POINT('Ctrl Pts',(-0.720264432790936,-0.3706448766936,
-0.744967531938193));
#35563=CARTESIAN_POINT('Ctrl Pts',(-0.456090204684126,-0.669432747147951,
-0.734383116231622));
#35564=CARTESIAN_POINT('Ctrl Pts',(-0.081353177576358,-0.805940530226077,
-0.723798700525052));
#35565=CARTESIAN_POINT('Ctrl Pts',(0.313105025141166,-0.74707678386777,
-0.71321428481848));
#35566=CARTESIAN_POINT('Ctrl Pts',(0.631662084608202,-0.507110923399685,
-0.70262986911191));
#35567=CARTESIAN_POINT('Ctrl Pts',(0.797095206354559,-0.144214110854122,
-0.692045453405339));
#35568=CARTESIAN_POINT('Ctrl Pts',(0.769301031878132,0.253642267995893,
-0.681461037698768));
#35569=CARTESIAN_POINT('Ctrl Pts',(0.555017267217064,0.590012127717527,
-0.670876621992197));
#35570=CARTESIAN_POINT('Ctrl Pts',(0.20618936649001,0.783354595894675,-0.660292206285626));
#35571=CARTESIAN_POINT('Ctrl Pts',(-0.19262179028868,0.786800688655548,
-0.649707790579056));
#35572=CARTESIAN_POINT('Ctrl Pts',(-0.544738665839292,0.599515023750439,
-0.639123374872485));
#35573=CARTESIAN_POINT('Ctrl Pts',(-0.764803085536454,0.266898329175701,
-0.628538959165914));
#35574=CARTESIAN_POINT('Ctrl Pts',(-0.799468281674222,-0.130418343647382,
-0.617954543459343));
#35575=CARTESIAN_POINT('Ctrl Pts',(-0.640330914137975,-0.496119741758063,
-0.607370127752772));
#35576=CARTESIAN_POINT('Ctrl Pts',(-0.325968160424072,-0.741554607667303,
-0.596785712046202));
#35577=CARTESIAN_POINT('Ctrl Pts',(0.0674139447942971,-0.80722601408164,
-0.58620129633963));
#35578=CARTESIAN_POINT('Ctrl Pts',(0.444453944105533,-0.6772142713587,-0.575616880633061));
#35579=CARTESIAN_POINT('Ctrl Pts',(0.713751940666771,-0.383036088322339,
-0.565032464926489));
#35580=CARTESIAN_POINT('Ctrl Pts',(0.810026242480743,0.00399552942575511,
-0.554448049219918));
#35581=CARTESIAN_POINT('Ctrl Pts',(0.709938579680874,0.390058573606021,
-0.543863633513348));
#35582=CARTESIAN_POINT('Ctrl Pts',(0.437751635462224,0.681565832046333,
-0.533279217806777));
#35583=CARTESIAN_POINT('Ctrl Pts',(0.059447424117716,0.807851769527449,
-0.522694802100205));
#35584=CARTESIAN_POINT('Ctrl Pts',(-0.333267694403375,0.738302865787421,
-0.512110386393635));
#35585=CARTESIAN_POINT('Ctrl Pts',(-0.645193949819297,0.489778771364619,
-0.501525970687064));
#35586=CARTESIAN_POINT('Ctrl Pts',(-0.800715949546566,0.122525286796663,
-0.490941554980493));
#35587=CARTESIAN_POINT('Ctrl Pts',(-0.762132933035007,-0.274430082436886,
-0.480357139273922));
#35588=CARTESIAN_POINT('Ctrl Pts',(-0.538797976179725,-0.604859668540974,
-0.469772723567352));
#35589=CARTESIAN_POINT('Ctrl Pts',(-0.184850671743447,-0.788662606517422,
-0.459188307860781));
#35590=CARTESIAN_POINT('Ctrl Pts',(0.213907083466054,-0.781282431266632,
-0.44860389215421));
#35591=CARTESIAN_POINT('Ctrl Pts',(0.560810697474509,-0.58450820298868,
-0.438019476447639));
#35592=CARTESIAN_POINT('Ctrl Pts',(0.771765764932892,-0.246040813362946,
-0.427435060741069));
#35593=CARTESIAN_POINT('Ctrl Pts',(0.79563375560773,0.152070393899081,-0.416850645034497));
#35594=CARTESIAN_POINT('Ctrl Pts',(0.626628726655168,0.513317559307143,
-0.406266229327927));
#35595=CARTESIAN_POINT('Ctrl Pts',(0.305719918052578,0.750129195185142,
-0.395681813621356));
#35596=CARTESIAN_POINT('Ctrl Pts',(-0.089299778054571,0.805098768724973,
-0.385097397914786));
#35597=CARTESIAN_POINT('Ctrl Pts',(-0.462671928758378,0.664900867874241,
-0.374512982208214));
#35598=CARTESIAN_POINT('Ctrl Pts',(-0.723885776272764,0.363521472101407,
-0.363928566501644));
#35599=CARTESIAN_POINT('Ctrl Pts',(-0.809619342106881,-0.0259807358690177,
-0.353344150795073));
#35600=CARTESIAN_POINT('Ctrl Pts',(-0.69908958184048,-0.409184841296576,
-0.342759735088502));
#35601=CARTESIAN_POINT('Ctrl Pts',(-0.419090492574486,-0.693196679717163,
-0.332175319381931));
#35602=CARTESIAN_POINT('Ctrl Pts',(-0.0374978646661203,-0.809167713093018,
-0.32159090367536));
#35603=CARTESIAN_POINT('Ctrl Pts',(0.353184783042777,-0.728984901678733,
-0.311006487968789));
#35604=CARTESIAN_POINT('Ctrl Pts',(0.658250379547182,-0.472085707555579,
-0.300422072262219));
#35605=CARTESIAN_POINT('Ctrl Pts',(0.803746655759618,-0.100746175410848,
-0.289837656555648));
#35606=CARTESIAN_POINT('Ctrl Pts',(0.754403227182257,0.29501567283314,-0.279253240849078));
#35607=CARTESIAN_POINT('Ctrl Pts',(0.52218165351834,0.619261495923831,-0.268668825142506));
#35608=CARTESIAN_POINT('Ctrl Pts',(0.163375759383167,0.793389461681509,
-0.258084409435936));
#35609=CARTESIAN_POINT('Ctrl Pts',(-0.23503474435684,0.775188456700946,
-0.247499993729365));
#35610=CARTESIAN_POINT('Ctrl Pts',(-0.576469488299965,0.569070665635125,
-0.236915578022794));
#35611=CARTESIAN_POINT('Ctrl Pts',(-0.778159713414792,0.225001992997841,
-0.226331162316223));
#35612=CARTESIAN_POINT('Ctrl Pts',(-0.791212989161812,-0.173610385023284,
-0.215746746609652));
#35613=CARTESIAN_POINT('Ctrl Pts',(-0.612464682138537,-0.530137120397013,
-0.205162330903081));
#35614=CARTESIAN_POINT('Ctrl Pts',(-0.285246595439292,-0.758151020532607,
-0.194577915196511));
#35615=CARTESIAN_POINT('Ctrl Pts',(0.111120202088729,-0.8023782591699,-0.18399349948994));
#35616=CARTESIAN_POINT('Ctrl Pts',(0.48054820104878,-0.652097501694006,
-0.173409083783369));
#35617=CARTESIAN_POINT('Ctrl Pts',(0.73348771265382,-0.343738992654054,
-0.162824668076798));
#35618=CARTESIAN_POINT('Ctrl Pts',(0.808612851326352,0.047946819377936,
-0.152240252370227));
#35619=CARTESIAN_POINT('Ctrl Pts',(0.687731314139997,0.428009542157163,
-0.141655836663656));
#35620=CARTESIAN_POINT('Ctrl Pts',(0.400108948943148,0.704316812114863,
-0.131071420957086));
#35621=CARTESIAN_POINT('Ctrl Pts',(0.0155437137054738,0.809887134152576,
-0.120487005250515));
#35622=CARTESIAN_POINT('Ctrl Pts',(-0.372890155274553,0.71913109295302,
-0.109902589543944));
#35623=CARTESIAN_POINT('Ctrl Pts',(-0.571421157135916,0.542397737891304,
-0.10284631240623));
#35624=CARTESIAN_POINT('Ctrl Pts',(-0.643664247046206,0.435663249423622,
-0.0993181738373734));
#35625=CARTESIAN_POINT('Ctrl Pts',(-0.459778808448986,-0.601851132366388,
-1.12625));
#35626=CARTESIAN_POINT('Ctrl Pts',(-0.35997790597287,-0.678093142316895,
-1.12272186143114));
#35627=CARTESIAN_POINT('Ctrl Pts',(-0.121819235374885,-0.779899516890621,
-1.11566558429343));
#35628=CARTESIAN_POINT('Ctrl Pts',(0.265169376314341,-0.743459799348471,
-1.10508116858686));
#35629=CARTESIAN_POINT('Ctrl Pts',(0.58778475434178,-0.526827671798993,
-1.09449675288029));
#35630=CARTESIAN_POINT('Ctrl Pts',(0.767958066793962,-0.18246928341655,
-1.08391233717372));
#35631=CARTESIAN_POINT('Ctrl Pts',(0.761944391177617,0.206114383395608,
-1.07332792146715));
#35632=CARTESIAN_POINT('Ctrl Pts',(0.571236150706839,0.544736978791855,
-1.06274350576057));
#35633=CARTESIAN_POINT('Ctrl Pts',(0.242046145015631,0.751305487993936,
-1.052159090054));
#35634=CARTESIAN_POINT('Ctrl Pts',(-0.145816290148117,0.775747822655396,
-1.04157467434743));
#35635=CARTESIAN_POINT('Ctrl Pts',(-0.498332306791342,0.612137244306613,
-1.03099025864086));
#35636=CARTESIAN_POINT('Ctrl Pts',(-0.730044650361353,0.300136098188639,
-1.02040584293429));
#35637=CARTESIAN_POINT('Ctrl Pts',(-0.784784111755367,-0.0846224744286134,
-1.00982142722772));
#35638=CARTESIAN_POINT('Ctrl Pts',(-0.649280459609721,-0.448867277349673,
-0.999237011521151));
#35639=CARTESIAN_POINT('Ctrl Pts',(-0.356382026600184,-0.704300257801392,
-0.988652595814578));
#35640=CARTESIAN_POINT('Ctrl Pts',(0.0229085673489721,-0.789000748765239,
-0.97806818010801));
#35641=CARTESIAN_POINT('Ctrl Pts',(0.396645769635941,-0.682436165170634,
-0.967483764401436));
#35642=CARTESIAN_POINT('Ctrl Pts',(0.674230369135852,-0.410439274720321,
-0.956899348694867));
#35643=CARTESIAN_POINT('Ctrl Pts',(0.788371862026309,-0.0389460270134185,
-0.946314932988296));
#35644=CARTESIAN_POINT('Ctrl Pts',(0.711400725851037,0.341988296746932,
-0.935730517281725));
#35645=CARTESIAN_POINT('Ctrl Pts',(0.461975861282485,0.640019757856149,
-0.925146101575155));
#35646=CARTESIAN_POINT('Ctrl Pts',(0.100561431158107,0.782901261841897,
-0.914561685868583));
#35647=CARTESIAN_POINT('Ctrl Pts',(-0.285230530863874,0.735996284919715,
-0.903977270162013));
#35648=CARTESIAN_POINT('Ctrl Pts',(-0.601878526106637,0.510675265639743,
-0.893392854455441));
#35649=CARTESIAN_POINT('Ctrl Pts',(-0.772622544972736,0.161559246623487,
-0.882808438748871));
#35650=CARTESIAN_POINT('Ctrl Pts',(-0.756071791238701,-0.226721048051633,
-0.8722240230423));
#35651=CARTESIAN_POINT('Ctrl Pts',(-0.556238404788084,-0.56004091296378,
-0.861639607335729));
#35652=CARTESIAN_POINT('Ctrl Pts',(-0.221564861015832,-0.757598838112923,
-0.851055191629159));
#35653=CARTESIAN_POINT('Ctrl Pts',(0.166819178923374,-0.77150395248008,
-0.840470775922587));
#35654=CARTESIAN_POINT('Ctrl Pts',(0.51476386024995,-0.598385457150939,
-0.829886360216018));
#35655=CARTESIAN_POINT('Ctrl Pts',(0.737922407977915,-0.280209755277387,
-0.819301944509446));
#35656=CARTESIAN_POINT('Ctrl Pts',(0.782197993447165,0.105892805214989,
-0.808717528802876));
#35657=CARTESIAN_POINT('Ctrl Pts',(0.636857580500936,0.466325432833394,
-0.798133113096304));
#35658=CARTESIAN_POINT('Ctrl Pts',(0.337133767205639,0.7137140955303,-0.787548697389735));
#35659=CARTESIAN_POINT('Ctrl Pts',(-0.0443161006228245,0.788088237683093,
-0.776964281683162));
#35660=CARTESIAN_POINT('Ctrl Pts',(-0.415023110842466,0.67141850184181,
-0.766379865976593));
#35661=CARTESIAN_POINT('Ctrl Pts',(-0.685122573884915,0.39198730324103,
-0.75579545027002));
#35662=CARTESIAN_POINT('Ctrl Pts',(-0.789138510796985,0.0175327672081737,
-0.745211034563451));
#35663=CARTESIAN_POINT('Ctrl Pts',(-0.701855968467241,-0.361171962748737,
-0.734626618856879));
#35664=CARTESIAN_POINT('Ctrl Pts',(-0.444433485458408,-0.652323435231444,
-0.724042203150309));
#35665=CARTESIAN_POINT('Ctrl Pts',(-0.0792739591687083,-0.78534236263338,
-0.713457787443737));
#35666=CARTESIAN_POINT('Ctrl Pts',(0.305102710404415,-0.727983051487286,
-0.702873371737167));
#35667=CARTESIAN_POINT('Ctrl Pts',(0.615518112450527,-0.494150220473696,
-0.692288956030596));
#35668=CARTESIAN_POINT('Ctrl Pts',(0.776723106885605,-0.140528297430925,
-0.681704540324026));
#35669=CARTESIAN_POINT('Ctrl Pts',(0.749639293834737,0.247159697944099,
-0.671120124617454));
#35670=CARTESIAN_POINT('Ctrl Pts',(0.540832177550744,0.574932642032597,
-0.660535708910884));
#35671=CARTESIAN_POINT('Ctrl Pts',(0.200919594133975,0.763333677916742,
-0.649951293204313));
#35672=CARTESIAN_POINT('Ctrl Pts',(-0.187698777027071,0.766691695697432,
-0.639366877497742));
#35673=CARTESIAN_POINT('Ctrl Pts',(-0.530816275895666,0.584192663761808,
-0.628782461791172));
#35674=CARTESIAN_POINT('Ctrl Pts',(-0.745256305668128,0.260076961707024,
-0.618198046084601));
#35675=CARTESIAN_POINT('Ctrl Pts',(-0.779035531324328,-0.127085121407204,
-0.607613630378029));
#35676=CARTESIAN_POINT('Ctrl Pts',(-0.623965384685697,-0.483439950627678,
-0.597029214671459));
#35677=CARTESIAN_POINT('Ctrl Pts',(-0.317637090641027,-0.72260201065176,
-0.586444798964888));
#35678=CARTESIAN_POINT('Ctrl Pts',(0.0656909842520752,-0.786594992189027,
-0.575860383258318));
#35679=CARTESIAN_POINT('Ctrl Pts',(0.433094623554483,-0.659906079830351,
-0.565275967551746));
#35680=CARTESIAN_POINT('Ctrl Pts',(0.695509922128081,-0.37324648072052,
-0.554691551845176));
#35681=CARTESIAN_POINT('Ctrl Pts',(0.789323652560836,0.00389341198452167,
-0.544107136138605));
#35682=CARTESIAN_POINT('Ctrl Pts',(0.691794022736101,0.380089485852299,
-0.533522720432034));
#35683=CARTESIAN_POINT('Ctrl Pts',(0.426563612012528,0.664146423656475,
-0.522938304725463));
#35684=CARTESIAN_POINT('Ctrl Pts',(0.0579280713131272,0.787204754624109,
-0.512353889018893));
#35685=CARTESIAN_POINT('Ctrl Pts',(-0.324750063678654,0.719433376546829,
-0.501769473312321));
#35686=CARTESIAN_POINT('Ctrl Pts',(-0.628704131266004,0.477261042279714,
-0.491185057605751));
#35687=CARTESIAN_POINT('Ctrl Pts',(-0.780251311394817,0.11939379471117,
-0.48060064189918));
#35688=CARTESIAN_POINT('Ctrl Pts',(-0.742654396723939,-0.267416218983553,
-0.470016226192609));
#35689=CARTESIAN_POINT('Ctrl Pts',(-0.525027417936622,-0.589400710521857,
-0.459431810486039));
#35690=CARTESIAN_POINT('Ctrl Pts',(-0.180126272146461,-0.768506026802313,
-0.448847394779467));
#35691=CARTESIAN_POINT('Ctrl Pts',(0.208440062278693,-0.761314473516765,
-0.438262979072897));
#35692=CARTESIAN_POINT('Ctrl Pts',(0.546477539752417,-0.569569386198947,
-0.427678563366326));
#35693=CARTESIAN_POINT('Ctrl Pts',(0.752041033427039,-0.239752520718236,
-0.417094147659755));
#35694=CARTESIAN_POINT('Ctrl Pts',(0.775299007787296,0.148183790183368,
-0.406509731953184));
#35695=CARTESIAN_POINT('Ctrl Pts',(0.610613396682346,0.500198227646385,
-0.395925316246614));
#35696=CARTESIAN_POINT('Ctrl Pts',(0.297906351328608,0.730957449505267,
-0.385340900540042));
#35697=CARTESIAN_POINT('Ctrl Pts',(-0.087017461028224,0.784522114809553,
-0.374756484833472));
#35698=CARTESIAN_POINT('Ctrl Pts',(-0.450846994322672,0.647907381388134,
-0.364172069126901));
#35699=CARTESIAN_POINT('Ctrl Pts',(-0.705384757924111,0.35423061759656,
-0.353587653420331));
#35700=CARTESIAN_POINT('Ctrl Pts',(-0.788927151716197,-0.0253167221713055,
-0.343003237713759));
#35701=CARTESIAN_POINT('Ctrl Pts',(-0.681222302768388,-0.398726925828479,
-0.332418822007189));
#35702=CARTESIAN_POINT('Ctrl Pts',(-0.40837940921436,-0.675480010995328,
-0.321834406300618));
#35703=CARTESIAN_POINT('Ctrl Pts',(-0.0365394970548715,-0.788487065402779,
-0.311249990594047));
#35704=CARTESIAN_POINT('Ctrl Pts',(0.344158112861213,-0.710353560265599,
-0.300665574887476));
#35705=CARTESIAN_POINT('Ctrl Pts',(0.641426865742676,-0.460020176467796,
-0.290081159180906));
#35706=CARTESIAN_POINT('Ctrl Pts',(0.783204559045904,-0.0981713122198202,
-0.279496743474334));
#35707=CARTESIAN_POINT('Ctrl Pts',(0.735122246113328,0.287475684405229,
-0.268912327767764));
#35708=CARTESIAN_POINT('Ctrl Pts',(0.508835774002905,0.603434457081194,
-0.258327912061193));
#35709=CARTESIAN_POINT('Ctrl Pts',(0.15920021398478,0.773112073356826,-0.247743496354623));
#35710=CARTESIAN_POINT('Ctrl Pts',(-0.22902774399788,0.755376248295729,
-0.237159080648051));
#35711=CARTESIAN_POINT('Ctrl Pts',(-0.561736124377012,0.554526400266621,
-0.226574664941481));
#35712=CARTESIAN_POINT('Ctrl Pts',(-0.75827156585345,0.219251408945243,
-0.215990249234909));
#35713=CARTESIAN_POINT('Ctrl Pts',(-0.770991226958462,-0.169173263830808,
-0.205405833528339));
#35714=CARTESIAN_POINT('Ctrl Pts',(-0.596811355752582,-0.516587915656082,
-0.194821417821768));
#35715=CARTESIAN_POINT('Ctrl Pts',(-0.277956284358327,-0.738774253642469,
-0.184237002115197));
#35716=CARTESIAN_POINT('Ctrl Pts',(0.108280200302349,-0.78187113583354,
-0.173652586408627));
#35717=CARTESIAN_POINT('Ctrl Pts',(0.468266386187336,-0.635431242679951,
-0.163068170702056));
#35718=CARTESIAN_POINT('Ctrl Pts',(0.71474128873568,-0.33495373727442,-0.152483754995485));
#35719=CARTESIAN_POINT('Ctrl Pts',(0.787946384751509,0.046721398166267,
-0.141899339288914));
#35720=CARTESIAN_POINT('Ctrl Pts',(0.670154328821455,0.417070506397101,
-0.131314923582343));
#35721=CARTESIAN_POINT('Ctrl Pts',(0.389882994450752,0.686315935883678,
-0.120730507875773));
#35722=CARTESIAN_POINT('Ctrl Pts',(0.0151464486370091,0.789188099552883,
-0.110146092169201));
#35723=CARTESIAN_POINT('Ctrl Pts',(-0.363359856668207,0.700751594443855,
-0.0995616764626311));
#35724=CARTESIAN_POINT('Ctrl Pts',(-0.55681681808202,0.528535177208507,
-0.0925053993249171));
#35725=CARTESIAN_POINT('Ctrl Pts',(-0.627213524521598,0.424528600787587,
-0.0889772607560602));
#35726=CARTESIAN_POINT('',(-0.676565692095423,0.457932546695692,-0.12));
#35727=CARTESIAN_POINT('Ctrl Pts',(0.351315334519666,0.671030718912565,
-0.12));
#35728=CARTESIAN_POINT('Ctrl Pts',(0.320499669985565,0.689321131271856,
-0.12));
#35729=CARTESIAN_POINT('Ctrl Pts',(0.288470314380151,0.705335580149119,
-0.12));
#35730=CARTESIAN_POINT('Ctrl Pts',(0.255512129576424,0.719045430115912,
-0.12));
#35731=CARTESIAN_POINT('Ctrl Pts',(0.22214779681421,0.732924228330563,-0.12));
#35732=CARTESIAN_POINT('Ctrl Pts',(0.187830516460429,0.744441808855943,
-0.12));
#35733=CARTESIAN_POINT('Ctrl Pts',(0.1528242686584,0.753525280825841,-0.12));
#35734=CARTESIAN_POINT('Ctrl Pts',(0.126989719984013,0.760228866998969,
-0.12));
#35735=CARTESIAN_POINT('Ctrl Pts',(0.100779187652097,0.765605880524251,
-0.12));
#35736=CARTESIAN_POINT('Ctrl Pts',(0.0742933277395626,0.76960959177323,
-0.12));
#35737=CARTESIAN_POINT('Ctrl Pts',(0.0666757152815714,0.770761101325464,
-0.12));
#35738=CARTESIAN_POINT('Ctrl Pts',(0.0590433060649341,0.771797653690197,
-0.12));
#35739=CARTESIAN_POINT('Ctrl Pts',(0.0514033585110513,0.772718183814392,
-0.12));
#35740=CARTESIAN_POINT('Ctrl Pts',(0.0392486607751243,0.774182691958918,
-0.12));
#35741=CARTESIAN_POINT('Ctrl Pts',(0.0270711318454161,0.775354140672433,
-0.12));
#35742=CARTESIAN_POINT('Ctrl Pts',(0.0148810082990363,0.776230637396706,
-0.12));
#35743=CARTESIAN_POINT('Ctrl Pts',(-0.0215690645837374,0.778851477895959,
-0.12));
#35744=CARTESIAN_POINT('Ctrl Pts',(-0.0581308241833953,0.778839173851118,
-0.12));
#35745=CARTESIAN_POINT('Ctrl Pts',(-0.0945366085257304,0.776289317214896,
-0.119999999999999));
#35746=CARTESIAN_POINT('Ctrl Pts',(-0.121214846927138,0.774420776694223,
-0.119999999999999));
#35747=CARTESIAN_POINT('Ctrl Pts',(-0.147809835066355,0.771188449071313,
-0.12));
#35748=CARTESIAN_POINT('Ctrl Pts',(-0.174217694473203,0.766612275855432,
-0.12));
#35749=CARTESIAN_POINT('Ctrl Pts',(-0.190197279886907,0.763843200572029,
-0.12));
#35750=CARTESIAN_POINT('Ctrl Pts',(-0.206108346383167,0.760581783987635,
-0.12));
#35751=CARTESIAN_POINT('Ctrl Pts',(-0.221927418745588,0.756829859540378,
-0.12));
#35752=CARTESIAN_POINT('Ctrl Pts',(-0.229467360158877,0.755041556795989,
-0.12));
#35753=CARTESIAN_POINT('Ctrl Pts',(-0.236985877671306,0.753141777075834,
-0.12));
#35754=CARTESIAN_POINT('Ctrl Pts',(-0.244467321374769,0.751134526250689,
-0.12));
#35755=CARTESIAN_POINT('Ctrl Pts',(-0.280535878868674,0.7414574312058,-0.12));
#35756=CARTESIAN_POINT('Ctrl Pts',(-0.315822129998283,0.729268499598691,
-0.12));
#35757=CARTESIAN_POINT('Ctrl Pts',(-0.350052129487708,0.714644278109736,
-0.12));
#35758=CARTESIAN_POINT('Ctrl Pts',(-0.355634194416505,0.712259429874209,
-0.12));
#35759=CARTESIAN_POINT('Ctrl Pts',(-0.361188160016036,0.709809706699139,
-0.12));
#35760=CARTESIAN_POINT('Ctrl Pts',(-0.366712818974203,0.707295310693253,
-0.12));
#35761=CARTESIAN_POINT('Ctrl Pts',(-0.397138122868593,0.693448073575234,
-0.12));
#35762=CARTESIAN_POINT('Ctrl Pts',(-0.426675742611669,0.677641907045338,
-0.12));
#35763=CARTESIAN_POINT('Ctrl Pts',(-0.455180005223245,0.66000787905436,
-0.12));
#35764=CARTESIAN_POINT('Ctrl Pts',(-0.461866014446751,0.65587161089679,
-0.12));
#35765=CARTESIAN_POINT('Ctrl Pts',(-0.468495101116925,0.651634643173702,
-0.12));
#35766=CARTESIAN_POINT('Ctrl Pts',(-0.475065246040253,0.647298434119057,
-0.12));
#35767=CARTESIAN_POINT('Ctrl Pts',(-0.481997163117426,0.642723460211044,
-0.12));
#35768=CARTESIAN_POINT('Ctrl Pts',(-0.488856348552518,0.638042668308952,
-0.12));
#35769=CARTESIAN_POINT('Ctrl Pts',(-0.495637685263811,0.633260662354593,
-0.12));
#35770=CARTESIAN_POINT('Ctrl Pts',(-0.526421712127851,0.611552641350735,
-0.12));
#35771=CARTESIAN_POINT('Ctrl Pts',(-0.555624158844379,0.587748863949367,
-0.12));
#35772=CARTESIAN_POINT('Ctrl Pts',(-0.583051806437047,0.562054023979174,
-0.12));
#35773=CARTESIAN_POINT('Ctrl Pts',(-0.610463295407308,0.536374321771544,
-0.12));
#35774=CARTESIAN_POINT('Ctrl Pts',(-0.636103059505849,0.50880506281788,
-0.12));
#35775=CARTESIAN_POINT('Ctrl Pts',(-0.659749387717314,0.479508356594237,
-0.12));
#35776=CARTESIAN_POINT('Ctrl Pts',(-0.665472951279087,0.472417126246673,
-0.12));
#35777=CARTESIAN_POINT('Ctrl Pts',(-0.671079552778587,0.465224522959082,
-0.12));
#35778=CARTESIAN_POINT('Ctrl Pts',(-0.676565692095422,0.457932546695692,
-0.12));
#35779=CARTESIAN_POINT('Ctrl Pts',(0.589349009255749,-0.565869316348656,
-1.12625));
#35780=CARTESIAN_POINT('Ctrl Pts',(0.595826955511021,-0.559130415243379,
-1.12600649737474));
#35781=CARTESIAN_POINT('Ctrl Pts',(0.694346705276116,-0.453008535243727,
-1.12223485618063));
#35782=CARTESIAN_POINT('Ctrl Pts',(0.828384689818385,-0.196826841568886,
-1.11493507641766));
#35783=CARTESIAN_POINT('Ctrl Pts',(0.821897829369206,0.222332451391628,
-1.10435066071109));
#35784=CARTESIAN_POINT('Ctrl Pts',(0.616183750099589,0.587599496275833,
-1.09376624500451));
#35785=CARTESIAN_POINT('Ctrl Pts',(0.261091496307317,0.810421806269904,
-1.08318182929794));
#35786=CARTESIAN_POINT('Ctrl Pts',(-0.157289815040412,0.836787381022574,
-1.07259741359137));
#35787=CARTESIAN_POINT('Ctrl Pts',(-0.537543482173721,0.660303137862947,
-1.0620129978848));
#35788=CARTESIAN_POINT('Ctrl Pts',(-0.7874880639875,0.323752245535046,-1.05142858217823));
#35789=CARTESIAN_POINT('Ctrl Pts',(-0.846534688677586,-0.0912809764781306,
-1.04084416647166));
#35790=CARTESIAN_POINT('Ctrl Pts',(-0.700368959446377,-0.484186307032688,
-1.03025975076509));
#35791=CARTESIAN_POINT('Ctrl Pts',(-0.38442387329105,-0.759717979177561,
-1.01967533505852));
#35792=CARTESIAN_POINT('Ctrl Pts',(0.0247111232736773,-0.851083110906004,
-1.00909091935195));
#35793=CARTESIAN_POINT('Ctrl Pts',(0.42785576069194,-0.736133514901142,
-0.998506503645377));
#35794=CARTESIAN_POINT('Ctrl Pts',(0.727282047487868,-0.442734604895683,
-0.987922087938807));
#35795=CARTESIAN_POINT('Ctrl Pts',(0.850404740342968,-0.0420104871635215,
-0.977337672232236));
#35796=CARTESIAN_POINT('Ctrl Pts',(0.767377146099821,0.368897575755567,
-0.966753256525664));
#35797=CARTESIAN_POINT('Ctrl Pts',(0.498326337204486,0.690379581274127,
-0.956168840819095));
#35798=CARTESIAN_POINT('Ctrl Pts',(0.108474086749781,0.844503687104731,
-0.945584425112522));
#35799=CARTESIAN_POINT('Ctrl Pts',(-0.307673836701548,0.793908001690772,
-0.935000009405953));
#35800=CARTESIAN_POINT('Ctrl Pts',(-0.649237214524841,0.550857644208324,
-0.924415593699381));
#35801=CARTESIAN_POINT('Ctrl Pts',(-0.833416191506255,0.174271502818131,
-0.913831177992811));
#35802=CARTESIAN_POINT('Ctrl Pts',(-0.815563145108209,-0.244560547230945,
-0.90324676228624));
#35803=CARTESIAN_POINT('Ctrl Pts',(-0.600005909618337,-0.604107617370174,
-0.892662346579669));
#35804=CARTESIAN_POINT('Ctrl Pts',(-0.238998646675454,-0.817210347352623,
-0.882077930873097));
#35805=CARTESIAN_POINT('Ctrl Pts',(0.17994531181254,-0.832209582792671,
-0.871493515166529));
#35806=CARTESIAN_POINT('Ctrl Pts',(0.555267949047113,-0.64546929415458,
-0.860909099459956));
#35807=CARTESIAN_POINT('Ctrl Pts',(0.795985681346874,-0.302258002417496,
-0.850324683753387));
#35808=CARTESIAN_POINT('Ctrl Pts',(0.843745082180559,0.114224958881187,
-0.839740268046815));
#35809=CARTESIAN_POINT('Ctrl Pts',(0.686968588642089,0.503018153901045,
-0.829155852340245));
#35810=CARTESIAN_POINT('Ctrl Pts',(0.363661068552687,0.769872542797965,
-0.818571436633673));
#35811=CARTESIAN_POINT('Ctrl Pts',(-0.047803103913807,0.850098799076459,
-0.807987020927103));
#35812=CARTESIAN_POINT('Ctrl Pts',(-0.447679119223231,0.724248928992339,
-0.797402605220532));
#35813=CARTESIAN_POINT('Ctrl Pts',(-0.739031303134287,0.422830743823914,
-0.786818189513961));
#35814=CARTESIAN_POINT('Ctrl Pts',(-0.85123171271497,0.0189123294010521,
-0.776233773807391));
#35815=CARTESIAN_POINT('Ctrl Pts',(-0.757081361438328,-0.389590704583327,
-0.765649358100819));
#35816=CARTESIAN_POINT('Ctrl Pts',(-0.479403643135562,-0.703651370980965,
-0.755064942394249));
#35817=CARTESIAN_POINT('Ctrl Pts',(-0.0855116143916565,-0.847136865411472,
-0.744480526687678));
#35818=CARTESIAN_POINT('Ctrl Pts',(0.329109654614668,-0.785264248628737,
-0.733896110981106));
#35819=CARTESIAN_POINT('Ctrl Pts',(0.663950028923553,-0.533032329251663,
-0.723311695274536));
#35820=CARTESIAN_POINT('Ctrl Pts',(0.837839405292465,-0.151585737700515,
-0.712727279567964));
#35821=CARTESIAN_POINT('Ctrl Pts',(0.808624507964925,0.266607408099481,
-0.702142863861395));
#35822=CARTESIAN_POINT('Ctrl Pts',(0.583387446549703,0.620171099087388,
-0.691558448154823));
#35823=CARTESIAN_POINT('Ctrl Pts',(0.216728911202081,0.82339643185054,-0.680974032448252));
#35824=CARTESIAN_POINT('Ctrl Pts',(-0.202467816811898,0.82701867457178,
-0.670389616741683));
#35825=CARTESIAN_POINT('Ctrl Pts',(-0.572583445726543,0.6301597437277,-0.659805201035111));
#35826=CARTESIAN_POINT('Ctrl Pts',(-0.803896645273107,0.280541064113054,
-0.64922078532854));
#35827=CARTESIAN_POINT('Ctrl Pts',(-0.840333782374013,-0.137084788127738,
-0.63863636962197));
#35828=CARTESIAN_POINT('Ctrl Pts',(-0.67306197304253,-0.521479324018831,
-0.628051953915399));
#35829=CARTESIAN_POINT('Ctrl Pts',(-0.342630299990165,-0.779459801698388,
-0.617467538208828));
#35830=CARTESIAN_POINT('Ctrl Pts',(0.0708598658787424,-0.848488057866867,
-0.606883122502257));
#35831=CARTESIAN_POINT('Ctrl Pts',(0.467172585207631,-0.7118306544154,-0.596298706795686));
#35832=CARTESIAN_POINT('Ctrl Pts',(0.750235977744155,-0.402615303525977,
-0.585714291089116));
#35833=CARTESIAN_POINT('Ctrl Pts',(0.851431422320551,0.00419976430822168,
-0.575129875382545));
#35834=CARTESIAN_POINT('Ctrl Pts',(0.746227693570422,0.409996749113464,
-0.564545459675974));
#35835=CARTESIAN_POINT('Ctrl Pts',(0.460127682361612,0.716404648826047,
-0.553961043969404));
#35836=CARTESIAN_POINT('Ctrl Pts',(0.0624861297268952,0.849145799334128,
-0.543376628262831));
#35837=CARTESIAN_POINT('Ctrl Pts',(-0.350302955852819,0.776041844268606,
-0.532792212556262));
#35838=CARTESIAN_POINT('Ctrl Pts',(-0.67817358692588,0.514814229534427,
-0.522207796849691));
#35839=CARTESIAN_POINT('Ctrl Pts',(-0.841645225850065,0.12878827096765,
-0.511623381143119));
#35840=CARTESIAN_POINT('Ctrl Pts',(-0.80109000565714,-0.288457809343551,
-0.501038965436549));
#35841=CARTESIAN_POINT('Ctrl Pts',(-0.566339092665934,-0.635777584579208,
-0.490454549729978));
#35842=CARTESIAN_POINT('Ctrl Pts',(-0.194299470937418,-0.82897576594764,
-0.479870134023407));
#35843=CARTESIAN_POINT('Ctrl Pts',(0.224841125840774,-0.821218346766367,
-0.469285718316837));
#35844=CARTESIAN_POINT('Ctrl Pts',(0.589477012918694,-0.614385836568145,
-0.458701302610266));
#35845=CARTESIAN_POINT('Ctrl Pts',(0.811215227944597,-0.258617398652365,
-0.448116886903695));
#35846=CARTESIAN_POINT('Ctrl Pts',(0.8363032512486,0.159843601330507,-0.437532471197124));
#35847=CARTESIAN_POINT('Ctrl Pts',(0.658659386600812,0.539556222628657,
-0.426948055490553));
#35848=CARTESIAN_POINT('Ctrl Pts',(0.321347051500517,0.788472686544893,
-0.416363639783983));
#35849=CARTESIAN_POINT('Ctrl Pts',(-0.0938644121072648,0.846252076555809,
-0.405779224077412));
#35850=CARTESIAN_POINT('Ctrl Pts',(-0.48632179762979,0.698887840846459,
-0.395194808370841));
#35851=CARTESIAN_POINT('Ctrl Pts',(-0.760887812970069,0.382103181111099,
-0.38461039266427));
#35852=CARTESIAN_POINT('Ctrl Pts',(-0.851003722888249,-0.0273087632644408,
-0.374025976957699));
#35853=CARTESIAN_POINT('Ctrl Pts',(-0.734824139984663,-0.43010067223277,
-0.363441561251128));
#35854=CARTESIAN_POINT('Ctrl Pts',(-0.440512659294738,-0.728630017160833,
-0.352857145544558));
#35855=CARTESIAN_POINT('Ctrl Pts',(-0.0394145998886176,-0.850529008473494,
-0.342272729837987));
#35856=CARTESIAN_POINT('Ctrl Pts',(0.371238123405903,-0.766247584505002,
-0.331688314131416));
#35857=CARTESIAN_POINT('Ctrl Pts',(0.691897407156195,-0.496216769731146,
-0.321103898424845));
#35858=CARTESIAN_POINT('Ctrl Pts',(0.844830849187047,-0.105895901792902,
-0.310519482718274));
#35859=CARTESIAN_POINT('Ctrl Pts',(0.792965189320117,0.310095649688961,
-0.299935067011704));
#35860=CARTESIAN_POINT('Ctrl Pts',(0.548873412549209,0.650915573609104,
-0.289350651305133));
#35861=CARTESIAN_POINT('Ctrl Pts',(0.171726850179941,0.833944238330876,
-0.278766235598562));
#35862=CARTESIAN_POINT('Ctrl Pts',(-0.247048745074761,0.814812873511381,
-0.268181819891991));
#35863=CARTESIAN_POINT('Ctrl Pts',(-0.605936216145871,0.598159196372131,
-0.257597404185421));
#35864=CARTESIAN_POINT('Ctrl Pts',(-0.817936008537478,0.236503161103038,
-0.247012988478849));
#35865=CARTESIAN_POINT('Ctrl Pts',(-0.831656513568513,-0.182484627408237,
-0.236428572772279));
#35866=CARTESIAN_POINT('Ctrl Pts',(-0.643771334910445,-0.557235529878874,
-0.225844157065708));
#35867=CARTESIAN_POINT('Ctrl Pts',(-0.29982721760122,-0.796904554312883,
-0.215259741359137));
#35868=CARTESIAN_POINT('Ctrl Pts',(0.116800205661488,-0.843392505842622,
-0.204675325652567));
#35869=CARTESIAN_POINT('Ctrl Pts',(0.50511183077167,-0.685430019722115,
-0.194090909945995));
#35870=CARTESIAN_POINT('Ctrl Pts',(0.770980560490097,-0.361309503413322,
-0.183506494239425));
#35871=CARTESIAN_POINT('Ctrl Pts',(0.849945784476039,0.0503976618012751,
-0.172922078532854));
#35872=CARTESIAN_POINT('Ctrl Pts',(0.722885284777081,0.449887613677287,
-0.162337662826283));
#35873=CARTESIAN_POINT('Ctrl Pts',(0.42056085792794,0.740318564577236,-0.151753247119712));
#35874=CARTESIAN_POINT('Ctrl Pts',(0.0163382438424028,0.85128520335196,
-0.141168831413141));
#35875=CARTESIAN_POINT('Ctrl Pts',(-0.391950752487246,0.755890089971351,
-0.130584415706571));
#35876=CARTESIAN_POINT('Ctrl Pts',(-0.600629835243707,0.5701228592569,-0.123528138568857));
#35877=CARTESIAN_POINT('Ctrl Pts',(-0.676565692095422,0.457932546695692,
-0.12));
#35878=CARTESIAN_POINT('Ctrl Pts',(0.589301091561372,-0.565833523687256,
-1.12625));
#35879=CARTESIAN_POINT('Ctrl Pts',(0.681795706363589,-0.469502756447982,
-1.12277201246584));
#35880=CARTESIAN_POINT('Ctrl Pts',(0.81857564756759,-0.230726286157592,
-1.11581603739752));
#35881=CARTESIAN_POINT('Ctrl Pts',(0.83073247791742,0.182054083126401,-1.10538207479504));
#35882=CARTESIAN_POINT('Ctrl Pts',(0.647100797261751,0.551826151980982,
-1.09494811219256));
#35883=CARTESIAN_POINT('Ctrl Pts',(0.310930583933833,0.79157490921723,-1.08451414959008));
#35884=CARTESIAN_POINT('Ctrl Pts',(-0.0985234799625354,0.844718114599206,
-1.0740801869876));
#35885=CARTESIAN_POINT('Ctrl Pts',(-0.48475737907202,0.698765466281198,
-1.06364622438511));
#35886=CARTESIAN_POINT('Ctrl Pts',(-0.756728010910768,0.388101050966165,
-1.05321226178264));
#35887=CARTESIAN_POINT('Ctrl Pts',(-0.850331447180054,-0.0140392876955771,
-1.04277829918015));
#35888=CARTESIAN_POINT('Ctrl Pts',(-0.743503406614721,-0.412872032986844,
-1.03234433657767));
#35889=CARTESIAN_POINT('Ctrl Pts',(-0.461424807647817,-0.714386145646102,
-1.02191037397519));
#35890=CARTESIAN_POINT('Ctrl Pts',(-0.0705839504414228,-0.847513141979658,
-1.01147641137271));
#35891=CARTESIAN_POINT('Ctrl Pts',(0.336894159842277,-0.780873113300908,
-1.00104244877023));
#35892=CARTESIAN_POINT('Ctrl Pts',(0.664963173900133,-0.530174058353571,
-0.990608486167752));
#35893=CARTESIAN_POINT('Ctrl Pts',(0.836294104630413,-0.154507939527313,
-0.980174523565271));
#35894=CARTESIAN_POINT('Ctrl Pts',(0.810502659647234,0.257577125376117,
-0.96974056096279));
#35895=CARTESIAN_POINT('Ctrl Pts',(0.59366811553693,0.608948854591686,-0.95930659836031));
#35896=CARTESIAN_POINT('Ctrl Pts',(0.236900417487042,0.816785607236096,
-0.94887263575783));
#35897=CARTESIAN_POINT('Ctrl Pts',(-0.175706936751581,0.832098317777405,
-0.938438673155349));
#35898=CARTESIAN_POINT('Ctrl Pts',(-0.546898513860029,0.651277630891634,
-0.928004710552868));
#35899=CARTESIAN_POINT('Ctrl Pts',(-0.789180970390855,0.316944685067354,
-0.917570747950387));
#35900=CARTESIAN_POINT('Ctrl Pts',(-0.845446053461757,-0.092095102919769,
-0.907136785347907));
#35901=CARTESIAN_POINT('Ctrl Pts',(-0.702431554241402,-0.479427209172021,
-0.896702822745427));
#35902=CARTESIAN_POINT('Ctrl Pts',(-0.39384733450868,-0.753753815530977,
-0.886268860142945));
#35903=CARTESIAN_POINT('Ctrl Pts',(0.00757040428266388,-0.850413561905815,
-0.875834897540466));
#35904=CARTESIAN_POINT('Ctrl Pts',(0.407203727626896,-0.746622837529435,
-0.865400934937985));
#35905=CARTESIAN_POINT('Ctrl Pts',(0.71085530448089,-0.466846091764925,
-0.854966972335503));
#35906=CARTESIAN_POINT('Ctrl Pts',(0.846951603734271,-0.0770293336317683,
-0.844533009733024));
#35907=CARTESIAN_POINT('Ctrl Pts',(0.783413448288196,0.330943962550494,
-0.834099047130542));
#35908=CARTESIAN_POINT('Ctrl Pts',(0.535217378667919,0.66091065574617,-0.823665084528063));
#35909=CARTESIAN_POINT('Ctrl Pts',(0.160865541628771,0.83509449454775,-0.813231121925581));
#35910=CARTESIAN_POINT('Ctrl Pts',(-0.251403815775338,0.812438710747312,
-0.802797159323101));
#35911=CARTESIAN_POINT('Ctrl Pts',(-0.604414930500539,0.598283485561275,
-0.79236319672062));
#35912=CARTESIAN_POINT('Ctrl Pts',(-0.814959764354287,0.243107218714002,
-0.78192923411814));
#35913=CARTESIAN_POINT('Ctrl Pts',(-0.833410920788056,-0.169371704893341,
-0.771495271515659));
#35914=CARTESIAN_POINT('Ctrl Pts',(-0.655419288781807,-0.541928125492692,
-0.76106130891318));
#35915=CARTESIAN_POINT('Ctrl Pts',(-0.322939169195012,-0.786746992562985,
-0.750627346310697));
#35916=CARTESIAN_POINT('Ctrl Pts',(0.0856607483339354,-0.846122197736321,
-0.740193383708219));
#35917=CARTESIAN_POINT('Ctrl Pts',(0.47406962223381,-0.706058447001635,
-0.729759421105735));
#35918=CARTESIAN_POINT('Ctrl Pts',(0.750735829721,-0.399570083064777,-0.719325458503257));
#35919=CARTESIAN_POINT('Ctrl Pts',(0.850446544913026,0.00110070557588867,
-0.708891495900775));
#35920=CARTESIAN_POINT('Ctrl Pts',(0.749699014916821,0.401512047565224,
-0.698457533298295));
#35921=CARTESIAN_POINT('Ctrl Pts',(0.472240379621288,0.707283225562725,
-0.688023570695814));
#35922=CARTESIAN_POINT('Ctrl Pts',(0.083470247592485,0.84634109853777,-0.677589608093334));
#35923=CARTESIAN_POINT('Ctrl Pts',(-0.32497460644901,0.785908418628138,
-0.667155645490853));
#35924=CARTESIAN_POINT('Ctrl Pts',(-0.656819890853628,0.540229736580928,
-0.656721682888372));
#35925=CARTESIAN_POINT('Ctrl Pts',(-0.83384655260312,0.167213827236748,
-0.646287720285892));
#35926=CARTESIAN_POINT('Ctrl Pts',(-0.81432774339868,-0.24521595306685,
-0.635853757683412));
#35927=CARTESIAN_POINT('Ctrl Pts',(-0.602864230054738,-0.59984602810036,
-0.62541979508093));
#35928=CARTESIAN_POINT('Ctrl Pts',(-0.249299950511683,-0.813086755507764,
-0.614985832478451));
#35929=CARTESIAN_POINT('Ctrl Pts',(0.163026670890489,-0.834675291287357,
-0.604551869875969));
#35930=CARTESIAN_POINT('Ctrl Pts',(0.536926373445071,-0.659523014614649,
-0.59411790727349));
#35931=CARTESIAN_POINT('Ctrl Pts',(0.784267482446793,-0.328914963605851,
-0.583683944671008));
#35932=CARTESIAN_POINT('Ctrl Pts',(0.846749373394363,0.0792214362626901,
-0.573249982068528));
#35933=CARTESIAN_POINT('Ctrl Pts',(0.709644477235602,0.468684598889571,
-0.562816019466046));
#35934=CARTESIAN_POINT('Ctrl Pts',(0.40526970683834,0.74767439572747,-0.552382056863567));
#35935=CARTESIAN_POINT('Ctrl Pts',(0.00536905683500232,0.850430309041236,
-0.541948094261085));
#35936=CARTESIAN_POINT('Ctrl Pts',(-0.395797130335717,0.752731804114374,
-0.531514131658606));
#35937=CARTESIAN_POINT('Ctrl Pts',(-0.703670213228203,0.47760733696484,
-0.521080169056124));
#35938=CARTESIAN_POINT('Ctrl Pts',(-0.845681612069302,0.0899063307845227,
-0.510646206453645));
#35939=CARTESIAN_POINT('Ctrl Pts',(-0.788357905185791,-0.318986442718713,
-0.500212243851163));
#35940=CARTESIAN_POINT('Ctrl Pts',(-0.54521082915687,-0.652691113067545,
-0.489778281248683));
#35941=CARTESIAN_POINT('Ctrl Pts',(-0.173552435486476,-0.832550352497661,
-0.479344318646202));
#35942=CARTESIAN_POINT('Ctrl Pts',(0.239013898693351,-0.816169647523525,
-0.468910356043722));
#35943=CARTESIAN_POINT('Ctrl Pts',(0.595242410120835,-0.607410084292985,
-0.458476393441241));
#35944=CARTESIAN_POINT('Ctrl Pts',(0.811166689955886,-0.255478254286475,
-0.448042430838761));
#35945=CARTESIAN_POINT('Ctrl Pts',(0.835891355663179,0.156672201857554,
-0.43760846823628));
#35946=CARTESIAN_POINT('Ctrl Pts',(0.663588571113166,0.531893547239614,
-0.4271745056338));
#35947=CARTESIAN_POINT('Ctrl Pts',(0.334871722342651,0.781742583516305,
-0.416740543031318));
#35948=CARTESIAN_POINT('Ctrl Pts',(-0.0727775393183068,0.847327544151471,
-0.406306580428838));
#35949=CARTESIAN_POINT('Ctrl Pts',(-0.463272450821894,0.713189437398579,
-0.395872617826357));
#35950=CARTESIAN_POINT('Ctrl Pts',(-0.744569690714111,0.410945875971156,
-0.385438655223877));
#35951=CARTESIAN_POINT('Ctrl Pts',(-0.850364855236199,0.0118385085176672,
-0.375004692621396));
#35952=CARTESIAN_POINT('Ctrl Pts',(-0.755721029601024,-0.390059306686192,
-0.364570730018916));
#35953=CARTESIAN_POINT('Ctrl Pts',(-0.482946653183774,-0.700016476572465,
-0.354136767416435));
#35954=CARTESIAN_POINT('Ctrl Pts',(-0.0963372107351888,-0.844973182506322,
-0.343702804813955));
#35955=CARTESIAN_POINT('Ctrl Pts',(0.312979817940913,-0.790761766178751,
-0.333268842211474));
#35956=CARTESIAN_POINT('Ctrl Pts',(0.648524561294595,-0.550160368159608,
-0.322834879608994));
#35957=CARTESIAN_POINT('Ctrl Pts',(0.831205969332431,-0.179880999456948,
-0.312400917006512));
#35958=CARTESIAN_POINT('Ctrl Pts',(0.817964316356762,0.232798011437263,
-0.301966954404033));
#35959=CARTESIAN_POINT('Ctrl Pts',(0.611920785515871,0.590604343299513,
-0.291532991801551));
#35960=CARTESIAN_POINT('Ctrl Pts',(0.261641771830851,0.809199678217179,
-0.281099029199071));
#35961=CARTESIAN_POINT('Ctrl Pts',(-0.150308664289153,0.837059044723434,
-0.27066506659659));
#35962=CARTESIAN_POINT('Ctrl Pts',(-0.526829940633294,0.667615720654169,
-0.26023110399411));
#35963=CARTESIAN_POINT('Ctrl Pts',(-0.779172437010209,0.340809105248279,
-0.249797141391629));
#35964=CARTESIAN_POINT('Ctrl Pts',(-0.847856686154441,-0.0663294394492015,
-0.239363178789149));
#35965=CARTESIAN_POINT('Ctrl Pts',(-0.716693103442292,-0.457833473536331,
-0.228929216186668));
#35966=CARTESIAN_POINT('Ctrl Pts',(-0.416598299086146,-0.741421929191928,
-0.218495253584187));
#35967=CARTESIAN_POINT('Ctrl Pts',(-0.0183072020772304,-0.850250118821527,
-0.208061290981707));
#35968=CARTESIAN_POINT('Ctrl Pts',(0.384298765226853,-0.758666652961298,
-0.197627328379226));
#35969=CARTESIAN_POINT('Ctrl Pts',(0.696322509060588,-0.488257754713524,
-0.187193365776746));
#35970=CARTESIAN_POINT('Ctrl Pts',(0.84421529649218,-0.102763035312453,
-0.176759403174265));
#35971=CARTESIAN_POINT('Ctrl Pts',(0.793120952222846,0.306956102035912,
-0.166325440571785));
#35972=CARTESIAN_POINT('Ctrl Pts',(0.555075924815366,0.644318467007061,
-0.155891477969304));
#35973=CARTESIAN_POINT('Ctrl Pts',(0.186203366191313,0.829817432539668,
-0.145457515366823));
#35974=CARTESIAN_POINT('Ctrl Pts',(-0.226576956355161,0.819703865231683,
-0.135023552764343));
#35975=CARTESIAN_POINT('Ctrl Pts',(-0.585915510641057,0.616411513065778,
-0.124589590161862));
#35976=CARTESIAN_POINT('Ctrl Pts',(-0.80722132928804,0.267758165995405,
-0.114155627559381));
#35977=CARTESIAN_POINT('Ctrl Pts',(-0.827788619517399,-0.00665018237018045,
-0.107199652491061));
#35978=CARTESIAN_POINT('Ctrl Pts',(-0.805186023504942,-0.138270823372324,
-0.103721664956901));
#35979=CARTESIAN_POINT('Ctrl Pts',(0.591130873629677,-0.567590438870538,
-1.12757052310292));
#35980=CARTESIAN_POINT('Ctrl Pts',(0.683912652131224,-0.470960598009098,
-1.12409253556876));
#35981=CARTESIAN_POINT('Ctrl Pts',(0.821117344248753,-0.23144266899012,
-1.11713656050044));
#35982=CARTESIAN_POINT('Ctrl Pts',(0.833311893543813,0.182619350617632,
-1.10670259789796));
#35983=CARTESIAN_POINT('Ctrl Pts',(0.64911004990092,0.553539577591926,-1.09626863529548));
#35984=CARTESIAN_POINT('Ctrl Pts',(0.31189602120762,0.794032746862491,-1.085834672693));
#35985=CARTESIAN_POINT('Ctrl Pts',(-0.0988293942380984,0.847340965934937,
-1.07540071009052));
#35986=CARTESIAN_POINT('Ctrl Pts',(-0.486262551456742,0.7009351325576,-1.06496674748804));
#35987=CARTESIAN_POINT('Ctrl Pts',(-0.759077651294708,0.389306105187746,
-1.05453278488556));
#35988=CARTESIAN_POINT('Ctrl Pts',(-0.85297172671121,-0.0140828798662705,
-1.04409882228308));
#35989=CARTESIAN_POINT('Ctrl Pts',(-0.745811984820572,-0.414154000672732,
-1.0336648596806));
#35990=CARTESIAN_POINT('Ctrl Pts',(-0.462857531842693,-0.716604314872263,
-1.02323089707812));
#35991=CARTESIAN_POINT('Ctrl Pts',(-0.0708031136070292,-0.850144670496582,
-1.01279693447564));
#35992=CARTESIAN_POINT('Ctrl Pts',(0.337940216291634,-0.783297724545797,
-1.00236297187316));
#35993=CARTESIAN_POINT('Ctrl Pts',(0.667027884744334,-0.531820248945421,
-0.991929009270677));
#35994=CARTESIAN_POINT('Ctrl Pts',(0.838890798054125,-0.154987686725405,
-0.981495046668197));
#35995=CARTESIAN_POINT('Ctrl Pts',(0.813019270631117,0.258376902423277,
-0.971061084065716));
#35996=CARTESIAN_POINT('Ctrl Pts',(0.595511455199308,0.61083964095294,-0.960627121463235));
#35997=CARTESIAN_POINT('Ctrl Pts',(0.237635993349256,0.819321726773046,
-0.950193158860755));
#35998=CARTESIAN_POINT('Ctrl Pts',(-0.176252506839004,0.834681983284209,
-0.939759196258274));
#35999=CARTESIAN_POINT('Ctrl Pts',(-0.548596633896848,0.653299848115922,
-0.929325233655793));
#36000=CARTESIAN_POINT('Ctrl Pts',(-0.791631377522398,0.31792879840216,
-0.918891271053313));
#36001=CARTESIAN_POINT('Ctrl Pts',(-0.848071163691739,-0.092381058239798,
-0.908457308450832));
#36002=CARTESIAN_POINT('Ctrl Pts',(-0.704612604411756,-0.480915830789212,
-0.898023345848352));
#36003=CARTESIAN_POINT('Ctrl Pts',(-0.395070230591335,-0.756094221336823,
-0.887589383245871));
#36004=CARTESIAN_POINT('Ctrl Pts',(0.00759391039005402,-0.853054096250918,
-0.87715542064339));
#36005=CARTESIAN_POINT('Ctrl Pts',(0.408468095313887,-0.748941101646617,
-0.86672145804091));
#36006=CARTESIAN_POINT('Ctrl Pts',(0.713062510398058,-0.468295649009072,
-0.856287495438429));
#36007=CARTESIAN_POINT('Ctrl Pts',(0.849581388698289,-0.077268509734015,
-0.845853532835948));
#36008=CARTESIAN_POINT('Ctrl Pts',(0.785845947261969,0.331971543645813,
-0.835419570233468));
#36009=CARTESIAN_POINT('Ctrl Pts',(0.536879228776822,0.662962783515193,
-0.824985607630987));
#36010=CARTESIAN_POINT('Ctrl Pts',(0.161365029180054,0.837687463184462,
-0.814551645028507));
#36011=CARTESIAN_POINT('Ctrl Pts',(-0.252184424692906,0.814961333169054,
-0.804117682426026));
#36012=CARTESIAN_POINT('Ctrl Pts',(-0.606291639027035,0.600141155949539,
-0.793683719823546));
#36013=CARTESIAN_POINT('Ctrl Pts',(-0.817490214648178,0.243862066695398,
-0.783249757221065));
#36014=CARTESIAN_POINT('Ctrl Pts',(-0.835998661927777,-0.169897604083914,
-0.772815794618584));
#36015=CARTESIAN_POINT('Ctrl Pts',(-0.657454365854886,-0.543610812472344,
-0.762381832016104));
#36016=CARTESIAN_POINT('Ctrl Pts',(-0.323941895404747,-0.789189842192653,
-0.751947869413623));
#36017=CARTESIAN_POINT('Ctrl Pts',(0.0859267249812216,-0.848749407394487,
-0.741513906811143));
#36018=CARTESIAN_POINT('Ctrl Pts',(0.475541608542061,-0.708250758675002,
-0.731079944208662));
#36019=CARTESIAN_POINT('Ctrl Pts',(0.753066864680076,-0.400810748283288,
-0.720645981606182));
#36020=CARTESIAN_POINT('Ctrl Pts',(0.853087181670373,0.00110412326700639,
-0.7102120190037));
#36021=CARTESIAN_POINT('Ctrl Pts',(0.752026830565643,0.402758742584047,
-0.69977805640122));
#36022=CARTESIAN_POINT('Ctrl Pts',(0.473706686130722,0.709479340173862,
-0.689344093798739));
#36023=CARTESIAN_POINT('Ctrl Pts',(0.0837294227343626,0.848968987882984,
-0.678910131196258));
#36024=CARTESIAN_POINT('Ctrl Pts',(-0.325983652691982,0.788348664485507,
-0.668476168593779));
#36025=CARTESIAN_POINT('Ctrl Pts',(-0.658859316796526,0.541907150062539,
-0.658042205991297));
#36026=CARTESIAN_POINT('Ctrl Pts',(-0.836435646379749,0.167733026216601,
-0.647608243388818));
#36027=CARTESIAN_POINT('Ctrl Pts',(-0.816856231267326,-0.245977348668995,
-0.637174280786336));
#36028=CARTESIAN_POINT('Ctrl Pts',(-0.604736123655922,-0.60170855018364,
-0.626740318183856));
#36029=CARTESIAN_POINT('Ctrl Pts',(-0.250074026927025,-0.815611390108666,
-0.616306355581375));
#36030=CARTESIAN_POINT('Ctrl Pts',(0.163532868748728,-0.83726695829783,
-0.605872392978895));
#36031=CARTESIAN_POINT('Ctrl Pts',(0.538593529983231,-0.661570833757573,
-0.595438430376414));
#36032=CARTESIAN_POINT('Ctrl Pts',(0.786702633196865,-0.329936244658886,
-0.585004467773934));
#36033=CARTESIAN_POINT('Ctrl Pts',(0.849378530433119,0.079467418844213,
-0.574570505171453));
#36034=CARTESIAN_POINT('Ctrl Pts',(0.711847923533838,0.470139864698849,
-0.564136542568972));
#36035=CARTESIAN_POINT('Ctrl Pts',(0.406528069390245,0.749995924933148,
-0.553702579966493));
#36036=CARTESIAN_POINT('Ctrl Pts',(0.00538572775796149,0.853070895386196,
-0.54326861736401));
#36037=CARTESIAN_POINT('Ctrl Pts',(-0.397026080534961,0.755069036574494,
-0.532834654761531));
#36038=CARTESIAN_POINT('Ctrl Pts',(-0.705855109435041,0.479090307878311,
-0.522400692159049));
#36039=CARTESIAN_POINT('Ctrl Pts',(-0.848307453708849,0.0901854899664934,
-0.51196672955657));
#36040=CARTESIAN_POINT('Ctrl Pts',(-0.7908057566996,-0.319976895711645,
-0.501532766954088));
#36041=CARTESIAN_POINT('Ctrl Pts',(-0.546903708932309,-0.654717719154274,
-0.491098804351608));
#36042=CARTESIAN_POINT('Ctrl Pts',(-0.174091315846699,-0.835135421572604,
-0.480664841749128));
#36043=CARTESIAN_POINT('Ctrl Pts',(0.23975603691495,-0.81870385450499,-0.470230879146647));
#36044=CARTESIAN_POINT('Ctrl Pts',(0.597090637969014,-0.609296092772836,
-0.459796916544167));
#36045=CARTESIAN_POINT('Ctrl Pts',(0.813685362752719,-0.256271514336748,
-0.449362953941686));
#36046=CARTESIAN_POINT('Ctrl Pts',(0.838486798553875,0.157158669087687,
-0.438928991339205));
#36047=CARTESIAN_POINT('Ctrl Pts',(0.665649013810144,0.533545076851013,
-0.428495028736725));
#36048=CARTESIAN_POINT('Ctrl Pts',(0.335911499133212,0.784169894454498,
-0.418061066134244));
#36049=CARTESIAN_POINT('Ctrl Pts',(-0.0730035135980338,0.849958496410589,
-0.407627103531763));
#36050=CARTESIAN_POINT('Ctrl Pts',(-0.464710911909924,0.715403890799101,
-0.397193140929283));
#36051=CARTESIAN_POINT('Ctrl Pts',(-0.746881579809863,0.412221863029791,
-0.386759178326802));
#36052=CARTESIAN_POINT('Ctrl Pts',(-0.853005238347077,0.0118752670898904,
-0.376325215724322));
#36053=CARTESIAN_POINT('Ctrl Pts',(-0.758067543607107,-0.391270440941414,
-0.36589125312184));
#36054=CARTESIAN_POINT('Ctrl Pts',(-0.484446202675582,-0.702190027925981,
-0.355457290519361));
#36055=CARTESIAN_POINT('Ctrl Pts',(-0.0966363378011864,-0.847596824471871,
-0.34502332791688));
#36056=CARTESIAN_POINT('Ctrl Pts',(0.313951620362249,-0.793217081681625,
-0.334589365314399));
#36057=CARTESIAN_POINT('Ctrl Pts',(0.650538230236913,-0.551868616254985,
-0.324155402711919));
#36058=CARTESIAN_POINT('Ctrl Pts',(0.833786864097282,-0.18043953001012,
-0.313721440109438));
#36059=CARTESIAN_POINT('Ctrl Pts',(0.820504095785434,0.233520849327348,
-0.303287477506957));
#36060=CARTESIAN_POINT('Ctrl Pts',(0.6138207997243,0.592438169948658,-0.292853514904477));
#36061=CARTESIAN_POINT('Ctrl Pts',(0.262454169604745,0.81171224344255,-0.282419552301996));
#36062=CARTESIAN_POINT('Ctrl Pts',(-0.150775372733257,0.839658113287939,
-0.271985589699516));
#36063=CARTESIAN_POINT('Ctrl Pts',(-0.528465747745009,0.669688667653643,
-0.261551627097035));
#36064=CARTESIAN_POINT('Ctrl Pts',(-0.781591767642338,0.341867317610364,
-0.251117664494554));
#36065=CARTESIAN_POINT('Ctrl Pts',(-0.850489281400512,-0.0665353923691048,
-0.240683701892074));
#36066=CARTESIAN_POINT('Ctrl Pts',(-0.718918435725105,-0.459255046614001,
-0.230249739289593));
#36067=CARTESIAN_POINT('Ctrl Pts',(-0.417891836923549,-0.743724044456582,
-0.219815776687113));
#36068=CARTESIAN_POINT('Ctrl Pts',(-0.0183640459380012,-0.852890145736156,
-0.209381814084632));
#36069=CARTESIAN_POINT('Ctrl Pts',(0.38549201298599,-0.761022313010097,
-0.198947851482151));
#36070=CARTESIAN_POINT('Ctrl Pts',(0.69848459067002,-0.489773795410256,
-0.188513888879671));
#36071=CARTESIAN_POINT('Ctrl Pts',(0.846836585170213,-0.103082114107123,
-0.17807992627719));
#36072=CARTESIAN_POINT('Ctrl Pts',(0.795583593099752,0.30790919991655,-0.16764596367471));
#36073=CARTESIAN_POINT('Ctrl Pts',(0.556799435517531,0.646319077797012,
-0.157212001072229));
#36074=CARTESIAN_POINT('Ctrl Pts',(0.186781528084318,0.832394012413366,
-0.146778038469748));
#36075=CARTESIAN_POINT('Ctrl Pts',(-0.227280478634909,0.822249052826763,
-0.136344075867268));
#36076=CARTESIAN_POINT('Ctrl Pts',(-0.58773477693239,0.61832545728428,-0.125910113264787));
#36077=CARTESIAN_POINT('Ctrl Pts',(-0.809727755002954,0.268589584372275,
-0.115476150662307));
#36078=CARTESIAN_POINT('Ctrl Pts',(-0.830358898319076,-0.00667087734730495,
-0.108520175593986));
#36079=CARTESIAN_POINT('Ctrl Pts',(-0.80768612908519,-0.138700154790167,
-0.105042188059826));
#36080=CARTESIAN_POINT('Ctrl Pts',(0.594875448103842,-0.571185894232435,
-1.13205842314276));
#36081=CARTESIAN_POINT('Ctrl Pts',(0.688244416305435,-0.47394451036991,
-1.1285804356086));
#36082=CARTESIAN_POINT('Ctrl Pts',(0.826319063393537,-0.232908375337079,
-1.12162446054028));
#36083=CARTESIAN_POINT('Ctrl Pts',(0.838590388344208,0.183775983334789,
-1.1111904979378));
#36084=CARTESIAN_POINT('Ctrl Pts',(0.653221937147487,0.557046083095301,
-1.10075653533532));
#36085=CARTESIAN_POINT('Ctrl Pts',(0.313871699922466,0.799062532067009,
-1.09032257273284));
#36086=CARTESIAN_POINT('Ctrl Pts',(-0.0994554132647963,0.852708501700446,
-1.07988861013036));
#36087=CARTESIAN_POINT('Ctrl Pts',(-0.489342809626885,0.705375220702387,
-1.06945464752788));
#36088=CARTESIAN_POINT('Ctrl Pts',(-0.763886051959438,0.391772185135781,
-1.0590206849254));
#36089=CARTESIAN_POINT('Ctrl Pts',(-0.858374910495864,-0.0141720913963306,
-1.04858672232292));
#36090=CARTESIAN_POINT('Ctrl Pts',(-0.750536357358176,-0.416777473112902,
-1.03815275972044));
#36091=CARTESIAN_POINT('Ctrl Pts',(-0.465789520808075,-0.721143672414928,
-1.02771879711796));
#36092=CARTESIAN_POINT('Ctrl Pts',(-0.0712516182342999,-0.855529943231549,
-1.01728483451548));
#36093=CARTESIAN_POINT('Ctrl Pts',(0.340080911027169,-0.788259553404189,
-1.006850871913));
#36094=CARTESIAN_POINT('Ctrl Pts',(0.67125319785122,-0.535189084049821,
-0.996416909310514));
#36095=CARTESIAN_POINT('Ctrl Pts',(0.844204783065118,-0.15596946206087,
-0.985982946708034));
#36096=CARTESIAN_POINT('Ctrl Pts',(0.81816937155348,0.260013600576988,-0.975548984105553));
#36097=CARTESIAN_POINT('Ctrl Pts',(0.599283744716542,0.614709027432676,
-0.965115021503073));
#36098=CARTESIAN_POINT('Ctrl Pts',(0.239141307420065,0.824511750823222,
-0.954681058900592));
#36099=CARTESIAN_POINT('Ctrl Pts',(-0.177368984921709,0.83996930744194,
-0.944247096298111));
#36100=CARTESIAN_POINT('Ctrl Pts',(-0.552071739738344,0.657438200377163,
-0.933813133695632));
#36101=CARTESIAN_POINT('Ctrl Pts',(-0.796645996016166,0.319942730235181,
-0.923379171093149));
#36102=CARTESIAN_POINT('Ctrl Pts',(-0.853443302115344,-0.092966249499067,
-0.91294520849067));
#36103=CARTESIAN_POINT('Ctrl Pts',(-0.709075999240419,-0.483962210060312,
-0.902511245888189));
#36104=CARTESIAN_POINT('Ctrl Pts',(-0.397572817705147,-0.760883728388119,
-0.892077283285709));
#36105=CARTESIAN_POINT('Ctrl Pts',(0.00764201429866176,-0.858457799247161,
-0.881643320683228));
#36106=CARTESIAN_POINT('Ctrl Pts',(0.411055551701723,-0.753685296994473,
-0.871209358080748));
#36107=CARTESIAN_POINT('Ctrl Pts',(0.717579431471206,-0.471262085267668,
-0.860775395478267));
#36108=CARTESIAN_POINT('Ctrl Pts',(0.854963093698934,-0.0777579699914457,
-0.850341432875786));
#36109=CARTESIAN_POINT('Ctrl Pts',(0.790823917731152,0.334074429773347,
-0.839907470273306));
#36110=CARTESIAN_POINT('Ctrl Pts',(0.540280110279977,0.667162345999428,
-0.829473507670825));
#36111=CARTESIAN_POINT('Ctrl Pts',(0.162387201977173,0.842993825670225,
-0.819039545068344));
#36112=CARTESIAN_POINT('Ctrl Pts',(-0.25378189633895,0.820123736136429,
-0.808605582465865));
#36113=CARTESIAN_POINT('Ctrl Pts',(-0.610132216032373,0.603942772490375,
-0.798171619863382));
#36114=CARTESIAN_POINT('Ctrl Pts',(-0.822668636909623,0.245406820054239,
-0.787737657260903));
#36115=CARTESIAN_POINT('Ctrl Pts',(-0.841294326638979,-0.170973826795073,
-0.777303694658422));
#36116=CARTESIAN_POINT('Ctrl Pts',(-0.661619035061958,-0.547054335443541,
-0.766869732055942));
#36117=CARTESIAN_POINT('Ctrl Pts',(-0.325993917425953,-0.794188994689024,
-0.75643576945346));
#36118=CARTESIAN_POINT('Ctrl Pts',(0.0864710310261411,-0.854125842178518,
-0.746001806850982));
#36119=CARTESIAN_POINT('Ctrl Pts',(0.478553944601616,-0.71273719952737,
-0.735567844248499));
#36120=CARTESIAN_POINT('Ctrl Pts',(0.757837194827813,-0.403349698920672,
-0.72513388164602));
#36121=CARTESIAN_POINT('Ctrl Pts',(0.858491094247378,0.00111111737703042,
-0.714699919043537));
#36122=CARTESIAN_POINT('Ctrl Pts',(0.756790572578483,0.405310032864,-0.704265956441059));
#36123=CARTESIAN_POINT('Ctrl Pts',(0.476707398805809,0.713973563521567,
-0.693831993838577));
#36124=CARTESIAN_POINT('Ctrl Pts',(0.0842598098862286,0.854346813607812,
-0.683398031236096));
#36125=CARTESIAN_POINT('Ctrl Pts',(-0.328048608300893,0.793342488510311,
-0.672964068633616));
#36126=CARTESIAN_POINT('Ctrl Pts',(-0.663032885717749,0.545339881120644,
-0.662530106031135));
#36127=CARTESIAN_POINT('Ctrl Pts',(-0.841734079185264,0.168795537328509,
-0.652096143428655));
#36128=CARTESIAN_POINT('Ctrl Pts',(-0.822030637537394,-0.24753550136041,
-0.641662180826173));
#36129=CARTESIAN_POINT('Ctrl Pts',(-0.608566847191112,-0.605520095441724,
-0.631228218223695));
#36130=CARTESIAN_POINT('Ctrl Pts',(-0.251658130179693,-0.820777910885976,
-0.620794255621212));
#36131=CARTESIAN_POINT('Ctrl Pts',(0.164568773806467,-0.842570657079702,
-0.610360293018733));
#36132=CARTESIAN_POINT('Ctrl Pts',(0.542005270791329,-0.66576157888414,
-0.599926330416251));
#36133=CARTESIAN_POINT('Ctrl Pts',(0.791686030375065,-0.332026238109064,
-0.589492367813771));
#36134=CARTESIAN_POINT('Ctrl Pts',(0.85475895042051,0.0799708081734412,
-0.57905840521129));
#36135=CARTESIAN_POINT('Ctrl Pts',(0.716357150761197,0.473117983210515,
-0.56862444260881));
#36136=CARTESIAN_POINT('Ctrl Pts',(0.409103236611468,0.754746802098496,
-0.558190480006329));
#36137=CARTESIAN_POINT('Ctrl Pts',(0.00541984385136099,0.858474704797125,
-0.547756517403849));
#36138=CARTESIAN_POINT('Ctrl Pts',(-0.399541057053306,0.759852049554789,
-0.537322554801367));
#36139=CARTESIAN_POINT('Ctrl Pts',(-0.710326374957927,0.482125123306196,
-0.526888592198888));
#36140=CARTESIAN_POINT('Ctrl Pts',(-0.853681088920773,0.0907567733170878,
-0.516454629596407));
#36141=CARTESIAN_POINT('Ctrl Pts',(-0.795815145266696,-0.32200380129438,
-0.506020666993927));
#36142=CARTESIAN_POINT('Ctrl Pts',(-0.550368090878974,-0.658865052970729,
-0.495586704391446));
#36143=CARTESIAN_POINT('Ctrl Pts',(-0.175194103781467,-0.840425618055572,
-0.485152741788965));
#36144=CARTESIAN_POINT('Ctrl Pts',(0.24127478047497,-0.823889964613384,
-0.474718779186485));
#36145=CARTESIAN_POINT('Ctrl Pts',(0.600872930889902,-0.613155701602509,
-0.464284816584004));
#36146=CARTESIAN_POINT('Ctrl Pts',(0.818839683037892,-0.257894875804611,
-0.453850853981523));
#36147=CARTESIAN_POINT('Ctrl Pts',(0.843798224459356,0.158154196539881,
-0.443416891379043));
#36148=CARTESIAN_POINT('Ctrl Pts',(0.669865592320392,0.536924838044412,
-0.432982928776562));
#36149=CARTESIAN_POINT('Ctrl Pts',(0.338039343055767,0.789137247904648,
-0.422548966174082));
#36150=CARTESIAN_POINT('Ctrl Pts',(-0.0734659570783422,0.855342590214103,
-0.412115003571601));
#36151=CARTESIAN_POINT('Ctrl Pts',(-0.467654640517619,0.719935643433753,
-0.40168104096912));
#36152=CARTESIAN_POINT('Ctrl Pts',(-0.751612729039847,0.414833097799243,
-0.39124707836664));
#36153=CARTESIAN_POINT('Ctrl Pts',(-0.85840863185104,0.0119504914122616,
-0.380813115764159));
#36154=CARTESIAN_POINT('Ctrl Pts',(-0.762869550742065,-0.393748958145996,
-0.370379153161678));
#36155=CARTESIAN_POINT('Ctrl Pts',(-0.487514945218855,-0.7066380768534,
-0.359945190559198));
#36156=CARTESIAN_POINT('Ctrl Pts',(-0.0972484842880587,-0.852965958176227,
-0.349511227956717));
#36157=CARTESIAN_POINT('Ctrl Pts',(0.315940358613543,-0.798241744877081,
-0.339077265354237));
#36158=CARTESIAN_POINT('Ctrl Pts',(0.654659088924836,-0.555364448591704,
-0.328643302751756));
#36159=CARTESIAN_POINT('Ctrl Pts',(0.839068518092747,-0.181582530945507,
-0.318209340149276));
#36160=CARTESIAN_POINT('Ctrl Pts',(0.825701609589118,0.235000095861305,
-0.307775377546795));
#36161=CARTESIAN_POINT('Ctrl Pts',(0.617709070479461,0.596190991632757,
-0.297341414944314));
#36162=CARTESIAN_POINT('Ctrl Pts',(0.26411669533205,0.816854064938793,-0.286907452341834));
#36163=CARTESIAN_POINT('Ctrl Pts',(-0.151730464954597,0.844976958912708,
-0.276473489739353));
#36164=CARTESIAN_POINT('Ctrl Pts',(-0.531813333742563,0.673930835536443,
-0.266039527136873));
#36165=CARTESIAN_POINT('Ctrl Pts',(-0.786542789844422,0.344032888819272,
-0.255605564534392));
#36166=CARTESIAN_POINT('Ctrl Pts',(-0.855876737496278,-0.0669568631605737,
-0.245171601931911));
#36167=CARTESIAN_POINT('Ctrl Pts',(-0.723472451346347,-0.462164215102107,
-0.234737639329431));
#36168=CARTESIAN_POINT('Ctrl Pts',(-0.420538988411856,-0.748435191644753,
-0.22430367672695));
#36169=CARTESIAN_POINT('Ctrl Pts',(-0.0184803735586201,-0.858292811196644,
-0.21386971412447));
#36170=CARTESIAN_POINT('Ctrl Pts',(0.387933926300145,-0.765843035246914,
-0.203435751521989));
#36171=CARTESIAN_POINT('Ctrl Pts',(0.702909167805226,-0.492876289710407,
-0.193001788919508));
#36172=CARTESIAN_POINT('Ctrl Pts',(0.852200902248733,-0.103735083894904,
-0.182567826317028));
#36173=CARTESIAN_POINT('Ctrl Pts',(0.80062324874381,0.309859647074902,-0.172133863714547));
#36174=CARTESIAN_POINT('Ctrl Pts',(0.560326498983091,0.650413239900023,
-0.161699901112067));
#36175=CARTESIAN_POINT('Ctrl Pts',(0.18796470919147,0.837666784744461,-0.151265938509586));
#36176=CARTESIAN_POINT('Ctrl Pts',(-0.228720208214088,0.827457735607709,
-0.140831975907105));
#36177=CARTESIAN_POINT('Ctrl Pts',(-0.591457779048169,0.622242032554347,
-0.130398013304625));
#36178=CARTESIAN_POINT('Ctrl Pts',(-0.814857060568082,0.270291466147333,
-0.119964050702144));
#36179=CARTESIAN_POINT('Ctrl Pts',(-0.83561875211749,-0.00671391055874626,
-0.113008075633824));
#36180=CARTESIAN_POINT('Ctrl Pts',(-0.812802493323686,-0.139578764049739,
-0.109530088099664));
#36181=CARTESIAN_POINT('Ctrl Pts',(0.596426278379634,-0.572674966240204,
-1.13871522674109));
#36182=CARTESIAN_POINT('Ctrl Pts',(0.690040836764293,-0.475177806505627,
-1.13523723920693));
#36183=CARTESIAN_POINT('Ctrl Pts',(0.828472169960178,-0.233517118585332,
-1.12828126413861));
#36184=CARTESIAN_POINT('Ctrl Pts',(0.840777371648047,0.184255830864911,
-1.11784730153613));
#36185=CARTESIAN_POINT('Ctrl Pts',(0.65492472312175,0.558498066470781,-1.10741333893365));
#36186=CARTESIAN_POINT('Ctrl Pts',(0.314690182553937,0.80114603583872,-1.09697937633117));
#36187=CARTESIAN_POINT('Ctrl Pts',(-0.099714792256329,0.854931601464745,
-1.08654541372869));
#36188=CARTESIAN_POINT('Ctrl Pts',(-0.490618589981855,0.70721432902319,
-1.07611145112621));
#36189=CARTESIAN_POINT('Ctrl Pts',(-0.765877684119506,0.392793594264123,
-1.06567748852373));
#36190=CARTESIAN_POINT('Ctrl Pts',(-0.860612864682261,-0.0142090290307453,
-1.05524352592124));
#36191=CARTESIAN_POINT('Ctrl Pts',(-0.752493169135755,-0.417864105986004,
-1.04480956331877));
#36192=CARTESIAN_POINT('Ctrl Pts',(-0.467003929674384,-0.723023842952487,
-1.03437560071628));
#36193=CARTESIAN_POINT('Ctrl Pts',(-0.0714373875773892,-0.857760491803007,
-1.02394163811381));
#36194=CARTESIAN_POINT('Ctrl Pts',(0.340967574370296,-0.790314711499318,
-1.01350767551132));
#36195=CARTESIAN_POINT('Ctrl Pts',(0.673003296155675,-0.536584435271303,
-1.00307371290884));
#36196=CARTESIAN_POINT('Ctrl Pts',(0.846405803153589,-0.156376107134283,
-0.992639750306363));
#36197=CARTESIAN_POINT('Ctrl Pts',(0.820302511565667,0.260691510764428,
-0.982205787703882));
#36198=CARTESIAN_POINT('Ctrl Pts',(0.600846203873041,0.616311703562287,
-0.971771825101402));
#36199=CARTESIAN_POINT('Ctrl Pts',(0.239764799219726,0.826661426818636,
-0.96133786249892));
#36200=CARTESIAN_POINT('Ctrl Pts',(-0.177831423260395,0.842159284588733,
-0.950903899896441));
#36201=CARTESIAN_POINT('Ctrl Pts',(-0.553511107201052,0.659152280411272,
-0.94046993729396));
#36202=CARTESIAN_POINT('Ctrl Pts',(-0.798723020136248,0.320776888411988,
-0.930035974691479));
#36203=CARTESIAN_POINT('Ctrl Pts',(-0.855668408795536,-0.0932086321197977,
-0.919602012088999));
#36204=CARTESIAN_POINT('Ctrl Pts',(-0.710924709912794,-0.485224001607969,
-0.909168049486518));
#36205=CARTESIAN_POINT('Ctrl Pts',(-0.398609373888867,-0.762867512737829,
-0.898734086884038));
#36206=CARTESIAN_POINT('Ctrl Pts',(0.0076619386418344,-0.860695979777121,
-0.888300124281556));
#36207=CARTESIAN_POINT('Ctrl Pts',(0.412127260215954,-0.75565031351505,
-0.877866161679076));
#36208=CARTESIAN_POINT('Ctrl Pts',(0.719450312385616,-0.472490764912421,
-0.867432199076595));
#36209=CARTESIAN_POINT('Ctrl Pts',(0.857192162794716,-0.0779607014182942,
-0.856998236474115));
#36210=CARTESIAN_POINT('Ctrl Pts',(0.792885762468364,0.334945432267619,
-0.846564273871634));
#36211=CARTESIAN_POINT('Ctrl Pts',(0.5416887344718,0.668901778939058,-0.836130311269154));
#36212=CARTESIAN_POINT('Ctrl Pts',(0.162810579659967,0.845191688359987,
-0.825696348666673));
#36213=CARTESIAN_POINT('Ctrl Pts',(-0.254443559264959,0.822261971679498,
-0.815262386064192));
#36214=CARTESIAN_POINT('Ctrl Pts',(-0.611722959395611,0.605517378668957,
-0.804828423461712));
#36215=CARTESIAN_POINT('Ctrl Pts',(-0.824813507545726,0.246046647390079,
-0.794394460859231));
#36216=CARTESIAN_POINT('Ctrl Pts',(-0.84348775837634,-0.171419591619671,
-0.783960498256751));
#36217=CARTESIAN_POINT('Ctrl Pts',(-0.663344015420905,-0.548480621469046,
-0.77352653565427));
#36218=CARTESIAN_POINT('Ctrl Pts',(-0.32684385232035,-0.796259612891541,
-0.76309257305179));
#36219=CARTESIAN_POINT('Ctrl Pts',(0.0866964792406478,-0.856352728383039,
-0.752658610449309));
#36220=CARTESIAN_POINT('Ctrl Pts',(0.479801635661559,-0.714595455721829,
-0.742224647846828));
#36221=CARTESIAN_POINT('Ctrl Pts',(0.759813036221548,-0.404401316651654,
-0.731790685244348));
#36222=CARTESIAN_POINT('Ctrl Pts',(0.860729361584667,0.00111401429436622,
-0.721356722641867));
#36223=CARTESIAN_POINT('Ctrl Pts',(0.758763685207283,0.406366761599003,
-0.710922760039386));
#36224=CARTESIAN_POINT('Ctrl Pts',(0.477950275531429,0.715835043177707,
-0.700488797436906));
#36225=CARTESIAN_POINT('Ctrl Pts',(0.0844794929808797,0.856574275931452,
-0.690054834834425));
#36226=CARTESIAN_POINT('Ctrl Pts',(-0.328903900207732,0.795410899692694,
-0.679620872231945));
#36227=CARTESIAN_POINT('Ctrl Pts',(-0.664761552283536,0.546761697202154,
-0.669186909629464));
#36228=CARTESIAN_POINT('Ctrl Pts',(-0.843928657450255,0.16923562289307,
-0.658752947026984));
#36229=CARTESIAN_POINT('Ctrl Pts',(-0.824173844774582,-0.248180878617352,
-0.648318984424503));
#36230=CARTESIAN_POINT('Ctrl Pts',(-0.610153509307647,-0.607098814033894,
-0.637885021822023));
#36231=CARTESIAN_POINT('Ctrl Pts',(-0.252314255999424,-0.822917852000584,
-0.627451059219541));
#36232=CARTESIAN_POINT('Ctrl Pts',(0.164997839307108,-0.844767416479698,
-0.617017096617062));
#36233=CARTESIAN_POINT('Ctrl Pts',(0.543418392840446,-0.667497359728489,
-0.606583134014579));
#36234=CARTESIAN_POINT('Ctrl Pts',(0.793750122821744,-0.33289190053569,
-0.596149171412101));
#36235=CARTESIAN_POINT('Ctrl Pts',(0.856987487271739,0.0801793089360827,
-0.585715208809619));
#36236=CARTESIAN_POINT('Ctrl Pts',(0.718224844931966,0.474351501572674,
-0.575281246207139));
#36237=CARTESIAN_POINT('Ctrl Pts',(0.410169855028622,0.756714586186626,
-0.564847283604658));
#36238=CARTESIAN_POINT('Ctrl Pts',(0.00543397452731906,0.860712929403663,
-0.554413321002177));
#36239=CARTESIAN_POINT('Ctrl Pts',(-0.400582744851701,0.761833144099726,
-0.543979358399697));
#36240=CARTESIAN_POINT('Ctrl Pts',(-0.712178345624295,0.483382125182179,
-0.533545395797217));
#36241=CARTESIAN_POINT('Ctrl Pts',(-0.855906815559753,0.090993395365603,
-0.523111433194736));
#36242=CARTESIAN_POINT('Ctrl Pts',(-0.797890003186722,-0.322843333114511,
-0.512677470592255));
#36243=CARTESIAN_POINT('Ctrl Pts',(-0.551803016563766,-0.660582853117555,
-0.502243507989775));
#36244=CARTESIAN_POINT('Ctrl Pts',(-0.175650871758219,-0.842616784886445,
-0.491809545387294));
#36245=CARTESIAN_POINT('Ctrl Pts',(0.241903834712186,-0.826038019508388,
-0.481375582784813));
#36246=CARTESIAN_POINT('Ctrl Pts',(0.602439533344005,-0.614754327830277,
-0.470941620182333));
#36247=CARTESIAN_POINT('Ctrl Pts',(0.82097457078373,-0.258567262135508,
-0.460507657579852));
#36248=CARTESIAN_POINT('Ctrl Pts',(0.845998184386402,0.158566537884764,
-0.450073694977372));
#36249=CARTESIAN_POINT('Ctrl Pts',(0.671612073193301,0.538324714333898,
-0.439639732374891));
#36250=CARTESIAN_POINT('Ctrl Pts',(0.338920682915143,0.791194695137898,
-0.429205769772411));
#36251=CARTESIAN_POINT('Ctrl Pts',(-0.0736574983223131,0.857572648737351,
-0.41877180716993));
#36252=CARTESIAN_POINT('Ctrl Pts',(-0.468873914793169,0.72181266748964,
-0.408337844567449));
#36253=CARTESIAN_POINT('Ctrl Pts',(-0.753572341938536,0.415914655172892,
-0.397903881964968));
#36254=CARTESIAN_POINT('Ctrl Pts',(-0.86064668419148,0.0119816488637972,
-0.387469919362488));
#36255=CARTESIAN_POINT('Ctrl Pts',(-0.764858512548967,-0.394775544721155,
-0.377035956760007));
#36256=CARTESIAN_POINT('Ctrl Pts',(-0.488785999497305,-0.708480431348438,
-0.366601994157526));
#36257=CARTESIAN_POINT('Ctrl Pts',(-0.0975020315960993,-0.855189820319156,
-0.356168031555046));
#36258=CARTESIAN_POINT('Ctrl Pts',(0.316764081759698,-0.800322929452839,
-0.345734068952565));
#36259=CARTESIAN_POINT('Ctrl Pts',(0.656365923236629,-0.556812400837173,
-0.335300106350085));
#36260=CARTESIAN_POINT('Ctrl Pts',(0.841256146677281,-0.182055954894479,
-0.324866143747604));
#36261=CARTESIAN_POINT('Ctrl Pts',(0.827854387825681,0.235612790663157,
-0.314432181145124));
#36262=CARTESIAN_POINT('Ctrl Pts',(0.619319568298158,0.597745387301993,
-0.303998218542643));
#36263=CARTESIAN_POINT('Ctrl Pts',(0.264805303262624,0.818983775723723,
-0.293564255940162));
#36264=CARTESIAN_POINT('Ctrl Pts',(-0.152126058284336,0.847179992119362,
-0.283130293337682));
#36265=CARTESIAN_POINT('Ctrl Pts',(-0.533199883246883,0.67568791521759,
-0.272696330735201));
#36266=CARTESIAN_POINT('Ctrl Pts',(-0.788593472808696,0.34492985538811,
-0.262262368132721));
#36267=CARTESIAN_POINT('Ctrl Pts',(-0.85810818859447,-0.0671314343578877,
-0.25182840553024));
#36268=CARTESIAN_POINT('Ctrl Pts',(-0.725358696723672,-0.463369173631078,
-0.241394442927759));
#36269=CARTESIAN_POINT('Ctrl Pts',(-0.42163542201511,-0.750386522096553,
-0.230960480325279));
#36270=CARTESIAN_POINT('Ctrl Pts',(-0.0185285562433286,-0.86053055751242,
-0.220526517722798));
#36271=CARTESIAN_POINT('Ctrl Pts',(0.388945352751919,-0.767839757527661,
-0.210092555120318));
#36272=CARTESIAN_POINT('Ctrl Pts',(0.704741798496438,-0.494161306472502,
-0.199658592517837));
#36273=CARTESIAN_POINT('Ctrl Pts',(0.854422773172538,-0.104005573943587,
-0.189224629915357));
#36274=CARTESIAN_POINT('Ctrl Pts',(0.802710635634209,0.310667577083977,
-0.178790667312876));
#36275=CARTESIAN_POINT('Ctrl Pts',(0.561787401646006,0.652108885332522,
-0.168356704710395));
#36276=CARTESIAN_POINT('Ctrl Pts',(0.188454746657786,0.839850992854134,
-0.157922742107915));
#36277=CARTESIAN_POINT('Ctrl Pts',(-0.229316478451291,0.829614630969344,
-0.147488779505434));
#36278=CARTESIAN_POINT('Ctrl Pts',(-0.592999937130289,0.623865269466565,
-0.137054816902953));
#36279=CARTESIAN_POINT('Ctrl Pts',(-0.816981345420958,0.270994210833155,
-0.126620854300473));
#36280=CARTESIAN_POINT('Ctrl Pts',(-0.837797728572329,-0.00672831308054614,
-0.119664879232153));
#36281=CARTESIAN_POINT('Ctrl Pts',(-0.81492145573658,-0.139942643537178,
-0.116186891697992));
#36282=CARTESIAN_POINT('Ctrl Pts',(0.596426278379634,-0.572674966240204,
-1.1425283350431));
#36283=CARTESIAN_POINT('Ctrl Pts',(0.690039237300988,-0.475179472305605,
-1.13905034750894));
#36284=CARTESIAN_POINT('Ctrl Pts',(0.82847297254682,-0.233515977058047,
-1.13209437244062));
#36285=CARTESIAN_POINT('Ctrl Pts',(0.840776790045668,0.184255282770994,
-1.12166040983814));
#36286=CARTESIAN_POINT('Ctrl Pts',(0.654924835154705,0.558498232654801,
-1.11122644723566));
#36287=CARTESIAN_POINT('Ctrl Pts',(0.314690017828941,0.801145770682765,
-1.10079248463318));
#36288=CARTESIAN_POINT('Ctrl Pts',(-0.0997147185513843,0.854931525810343,
-1.0903585220307));
#36289=CARTESIAN_POINT('Ctrl Pts',(-0.490618537208122,0.707214177068773,
-1.07992455942821));
#36290=CARTESIAN_POINT('Ctrl Pts',(-0.765877541643972,0.392793546079606,
-1.06949059682574));
#36291=CARTESIAN_POINT('Ctrl Pts',(-0.860612728693631,-0.0142090354680799,
-1.05905663422325));
#36292=CARTESIAN_POINT('Ctrl Pts',(-0.752493039839578,-0.417864031829528,
-1.04862267162077));
#36293=CARTESIAN_POINT('Ctrl Pts',(-0.467003853748614,-0.723023724671487,
-1.03818870901829));
#36294=CARTESIAN_POINT('Ctrl Pts',(-0.0714373746764496,-0.857760347616997,
-1.02775474641581));
#36295=CARTESIAN_POINT('Ctrl Pts',(0.340967517012713,-0.790314580308689,
-1.01732078381333));
#36296=CARTESIAN_POINT('Ctrl Pts',(0.673003184192239,-0.536584345498902,
-1.00688682121085));
#36297=CARTESIAN_POINT('Ctrl Pts',(0.846405661890073,-0.156376081212101,
-0.996452858608372));
#36298=CARTESIAN_POINT('Ctrl Pts',(0.820302374851196,0.260691467373266,
-0.986018896005888));
#36299=CARTESIAN_POINT('Ctrl Pts',(0.600846103651696,0.616311600756361,
-0.97558493340341));
#36300=CARTESIAN_POINT('Ctrl Pts',(0.239764759257472,0.826661288997698,
-0.965150970800928));
#36301=CARTESIAN_POINT('Ctrl Pts',(-0.17783139361675,0.842159144153302,
-0.954717008198448));
#36302=CARTESIAN_POINT('Ctrl Pts',(-0.553511014901828,0.659152170506626,
-0.944283045595968));
#36303=CARTESIAN_POINT('Ctrl Pts',(-0.798722886956041,0.320776834921644,
-0.933849082993486));
#36304=CARTESIAN_POINT('Ctrl Pts',(-0.855668266116611,-0.0932086165764496,
-0.923415120391006));
#36305=CARTESIAN_POINT('Ctrl Pts',(-0.710924591370777,-0.485223920700346,
-0.912981157788526));
#36306=CARTESIAN_POINT('Ctrl Pts',(-0.398609307422754,-0.762867385533718,
-0.902547195186045));
#36307=CARTESIAN_POINT('Ctrl Pts',(0.00766193736409961,-0.860695836261202,
-0.892113232583564));
#36308=CARTESIAN_POINT('Ctrl Pts',(0.412127191496183,-0.755650187514622,
-0.881679269981084));
#36309=CARTESIAN_POINT('Ctrl Pts',(0.719450192421382,-0.472490686127355,
-0.871245307378603));
#36310=CARTESIAN_POINT('Ctrl Pts',(0.857192019862882,-0.0779606884187723,
-0.860811344776123));
#36311=CARTESIAN_POINT('Ctrl Pts',(0.79288563025922,0.334945376417385,-0.850377382173642));
#36312=CARTESIAN_POINT('Ctrl Pts',(0.541688644148329,0.668901667403547,
-0.839943419571162));
#36313=CARTESIAN_POINT('Ctrl Pts',(0.162810552512238,0.845191547429138,
-0.829509456968681));
#36314=CARTESIAN_POINT('Ctrl Pts',(-0.25444351683796,0.822261834572052,
-0.8190754943662));
#36315=CARTESIAN_POINT('Ctrl Pts',(-0.611722857394332,0.605517277702421,
-0.80864153176372));
#36316=CARTESIAN_POINT('Ctrl Pts',(-0.824813370012825,0.246046606363219,
-0.798207569161239));
#36317=CARTESIAN_POINT('Ctrl Pts',(-0.843487617729615,-0.171419563036442,
-0.787773606558759));
#36318=CARTESIAN_POINT('Ctrl Pts',(-0.663343904812112,-0.548480530013062,
-0.777339643956278));
#36319=CARTESIAN_POINT('Ctrl Pts',(-0.32684379782102,-0.796259480119838,
-0.766905681353796));
#36320=CARTESIAN_POINT('Ctrl Pts',(0.0866964647845089,-0.856352585591155,
-0.756471718751317));
#36321=CARTESIAN_POINT('Ctrl Pts',(0.479801555657401,-0.714595336567153,
-0.746037756148836));
#36322=CARTESIAN_POINT('Ctrl Pts',(0.7598129095271,-0.404401249220064,-0.735603793546356));
#36323=CARTESIAN_POINT('Ctrl Pts',(0.860729218063005,0.00111401410861053,
-0.725169830943874));
#36324=CARTESIAN_POINT('Ctrl Pts',(0.758763558687808,0.406366693839686,
-0.714735868341394));
#36325=CARTESIAN_POINT('Ctrl Pts',(0.477950195835974,0.715834923816337,
-0.704301905738913));
#36326=CARTESIAN_POINT('Ctrl Pts',(0.0844794788944107,0.856574133102626,
-0.693867943136432));
#36327=CARTESIAN_POINT('Ctrl Pts',(-0.328903845364902,0.795410767062507,
-0.683433980533953));
#36328=CARTESIAN_POINT('Ctrl Pts',(-0.664761441438376,0.546761606032791,
-0.673000017931471));
#36329=CARTESIAN_POINT('Ctrl Pts',(-0.843928516730013,0.169235594674005,
-0.662566055328991));
#36330=CARTESIAN_POINT('Ctrl Pts',(-0.82417370734834,-0.24818083723462,
-0.652132092726511));
#36331=CARTESIAN_POINT('Ctrl Pts',(-0.610153407568064,-0.607098712803663,
-0.64169813012403));
#36332=CARTESIAN_POINT('Ctrl Pts',(-0.252314213927475,-0.822917714783773,
-0.63126416752155));
#36333=CARTESIAN_POINT('Ctrl Pts',(0.164997811794668,-0.844767275619597,
-0.620830204919068));
#36334=CARTESIAN_POINT('Ctrl Pts',(0.543418302228559,-0.66749724842715,
-0.610396242316588));
#36335=CARTESIAN_POINT('Ctrl Pts',(0.793749990468483,-0.332891845027883,
-0.599962279714107));
#36336=CARTESIAN_POINT('Ctrl Pts',(0.856987344374013,0.0801792955666445,
-0.589528317111627));
#36337=CARTESIAN_POINT('Ctrl Pts',(0.71822472517211,0.474351422477294,-0.579094354509146));
#36338=CARTESIAN_POINT('Ctrl Pts',(0.410169786635162,0.756714460008827,
-0.568660391906666));
#36339=CARTESIAN_POINT('Ctrl Pts',(0.00543397362123471,0.86071278588474,
-0.558226429304185));
#36340=CARTESIAN_POINT('Ctrl Pts',(-0.400582678056836,0.761833017068438,
-0.547792466701704));
#36341=CARTESIAN_POINT('Ctrl Pts',(-0.712178226872659,0.483382044580994,
-0.537358504099224));
#36342=CARTESIAN_POINT('Ctrl Pts',(-0.855906672842221,0.0909933801929788,
-0.526924541496743));
#36343=CARTESIAN_POINT('Ctrl Pts',(-0.797889870143161,-0.322843279282246,
-0.516490578894263));
#36344=CARTESIAN_POINT('Ctrl Pts',(-0.551802924553791,-0.660582742969169,
-0.506056616291782));
#36345=CARTESIAN_POINT('Ctrl Pts',(-0.175650842469449,-0.842616644384951,
-0.495622653689302));
#36346=CARTESIAN_POINT('Ctrl Pts',(0.241903794376115,-0.826037881771306,
-0.485188691086821));
#36347=CARTESIAN_POINT('Ctrl Pts',(0.602439432890683,-0.614754225323535,
-0.47475472848434));
#36348=CARTESIAN_POINT('Ctrl Pts',(0.82097443389095,-0.258567219020906,
-0.46432076588186));
#36349=CARTESIAN_POINT('Ctrl Pts',(0.845998043321078,0.158566511444706,
-0.453886803279379));
#36350=CARTESIAN_POINT('Ctrl Pts',(0.671611961205856,0.538324624571355,
-0.443452840676899));
#36351=CARTESIAN_POINT('Ctrl Pts',(0.338920626402072,0.791194563210736,
-0.433018878074418));
#36352=CARTESIAN_POINT('Ctrl Pts',(-0.0736574860403502,0.85757250574206,
-0.422584915471937));
#36353=CARTESIAN_POINT('Ctrl Pts',(-0.468873836611143,0.72181254713152,
-0.412150952869456));
#36354=CARTESIAN_POINT('Ctrl Pts',(-0.753572216284692,0.41591458582155,
-0.401716990266976));
#36355=CARTESIAN_POINT('Ctrl Pts',(-0.860646540683597,0.0119816468658661,
-0.391283027664495));
#36356=CARTESIAN_POINT('Ctrl Pts',(-0.764858385013229,-0.394775478894489,
-0.380849065062015));
#36357=CARTESIAN_POINT('Ctrl Pts',(-0.48878591799503,-0.708480313213638,
-0.370415102459534));
#36358=CARTESIAN_POINT('Ctrl Pts',(-0.0975020153382475,-0.855189677720724,
-0.359981139857053));
#36359=CARTESIAN_POINT('Ctrl Pts',(0.316764028941211,-0.800322796004496,
-0.349547177254573));
#36360=CARTESIAN_POINT('Ctrl Pts',(0.656365813791197,-0.556812307990154,
-0.339113214652092));
#36361=CARTESIAN_POINT('Ctrl Pts',(0.84125600640305,-0.182055924541153,
-0.328679252049612));
#36362=CARTESIAN_POINT('Ctrl Pts',(0.827854249784972,0.235612751382874,
-0.318245289447131));
#36363=CARTESIAN_POINT('Ctrl Pts',(0.61931946503168,0.597745287618039,-0.307811326844651));
#36364=CARTESIAN_POINT('Ctrl Pts',(0.264805259104931,0.818983639189147,
-0.29737736424217));
#36365=CARTESIAN_POINT('Ctrl Pts',(-0.152126032912425,0.847179850805378,
-0.286943401639689));
#36366=CARTESIAN_POINT('Ctrl Pts',(-0.533199794350212,0.675687802651956,
-0.276509439037209));
#36367=CARTESIAN_POINT('Ctrl Pts',(-0.78859334129299,0.344929797673649,
-0.266075476434728));
#36368=CARTESIAN_POINT('Ctrl Pts',(-0.858108045553686,-0.067131422772148,
-0.255641513832248));
#36369=CARTESIAN_POINT('Ctrl Pts',(-0.725358575688162,-0.463369097137429,
-0.245207551229767));
#36370=CARTESIAN_POINT('Ctrl Pts',(-0.421635351879133,-0.750386395459336,
-0.234773588627287));
#36371=CARTESIAN_POINT('Ctrl Pts',(-0.0185285528209972,-0.860530417001192,
-0.224339626024805));
#36372=CARTESIAN_POINT('Ctrl Pts',(0.388945287243321,-0.767839623642233,
-0.213905663422325));
#36373=CARTESIAN_POINT('Ctrl Pts',(0.704741682270793,-0.494161235578596,
-0.203471700819845));
#36374=CARTESIAN_POINT('Ctrl Pts',(0.854422628174535,-0.104005533986048,
-0.193037738217364));
#36375=CARTESIAN_POINT('Ctrl Pts',(0.802710506756154,0.310667480825686,
-0.182603775614883));
#36376=CARTESIAN_POINT('Ctrl Pts',(0.561787298202017,0.652108863993629,
-0.172169813012403));
#36377=CARTESIAN_POINT('Ctrl Pts',(0.188454734446523,0.839850680936053,
-0.161735850409922));
#36378=CARTESIAN_POINT('Ctrl Pts',(-0.229316478079899,0.829614831389836,
-0.151301887807442));
#36379=CARTESIAN_POINT('Ctrl Pts',(-0.592999762703061,0.623864489566949,
-0.140867925204961));
#36380=CARTESIAN_POINT('Ctrl Pts',(-0.816981370219958,0.270995606044562,
-0.13043396260248));
#36381=CARTESIAN_POINT('Ctrl Pts',(-0.837797337716894,-0.00673058913073388,
-0.12347798753416));
#36382=CARTESIAN_POINT('Ctrl Pts',(-0.81492145573658,-0.139942643537178,
-0.12));
#36383=CARTESIAN_POINT('Ctrl Pts',(-0.676565692095419,0.457932546695697,
-0.12));
#36384=CARTESIAN_POINT('Ctrl Pts',(-0.715290549838902,0.406460878340127,
-0.12));
#36385=CARTESIAN_POINT('Ctrl Pts',(-0.761722039381187,0.328281076047514,
-0.12));
#36386=CARTESIAN_POINT('Ctrl Pts',(-0.80978086870511,0.169044693082724,
-0.12));
#36387=CARTESIAN_POINT('Ctrl Pts',(-0.820456584566053,0.110526708837256,
-0.12));
#36388=CARTESIAN_POINT('Ctrl Pts',(-0.829018965506486,-0.012510540419889,
-0.12));
#36389=CARTESIAN_POINT('Ctrl Pts',(-0.825768317377141,-0.0767786210857152,
-0.12));
#36390=CARTESIAN_POINT('Ctrl Pts',(-0.81492145573658,-0.139942643537178,
-0.12));
#36391=CARTESIAN_POINT('Origin',(0.23094010767585,0.4,1.6));
#36392=CARTESIAN_POINT('',(0.23094010767585,0.4,1.6));
#36393=CARTESIAN_POINT('',(0.461880215351701,0.,1.6));
#36394=CARTESIAN_POINT('',(0.288675134594813,0.3,1.6));
#36395=CARTESIAN_POINT('',(0.23094010767585,0.4,1.1));
#36396=CARTESIAN_POINT('',(0.23094010767585,0.4,1.6));
#36397=CARTESIAN_POINT('',(0.461880215351701,0.,1.1));
#36398=CARTESIAN_POINT('',(0.461880215351701,0.,1.1));
#36399=CARTESIAN_POINT('',(0.461880215351701,0.,1.6));
#36400=CARTESIAN_POINT('Origin',(-0.23094010767585,0.4,1.6));
#36401=CARTESIAN_POINT('',(-0.23094010767585,0.4,1.6));
#36402=CARTESIAN_POINT('',(-0.115470053837925,0.4,1.6));
#36403=CARTESIAN_POINT('',(-0.23094010767585,0.4,1.1));
#36404=CARTESIAN_POINT('',(-0.23094010767585,0.4,1.6));
#36405=CARTESIAN_POINT('',(0.23094010767585,0.4,1.1));
#36406=CARTESIAN_POINT('Origin',(-0.461880215351701,5.55111512312578E-17,
1.6));
#36407=CARTESIAN_POINT('',(-0.461880215351701,5.6564012731995E-17,1.6));
#36408=CARTESIAN_POINT('',(-0.404145188432738,0.1,1.6));
#36409=CARTESIAN_POINT('',(-0.461880215351701,5.55111512312578E-17,1.1));
#36410=CARTESIAN_POINT('',(-0.461880215351701,5.6564012731995E-17,1.6));
#36411=CARTESIAN_POINT('',(-0.23094010767585,0.4,1.1));
#36412=CARTESIAN_POINT('Origin',(-0.230940107675851,-0.4,1.6));
#36413=CARTESIAN_POINT('',(-0.230940107675851,-0.4,1.6));
#36414=CARTESIAN_POINT('',(-0.288675134594813,-0.3,1.6));
#36415=CARTESIAN_POINT('',(-0.230940107675851,-0.4,1.1));
#36416=CARTESIAN_POINT('',(-0.230940107675851,-0.4,1.6));
#36417=CARTESIAN_POINT('',(-0.461880215351701,5.6564012731995E-17,1.1));
#36418=CARTESIAN_POINT('Origin',(0.23094010767585,-0.4,1.6));
#36419=CARTESIAN_POINT('',(0.23094010767585,-0.4,1.6));
#36420=CARTESIAN_POINT('',(0.115470053837925,-0.4,1.6));
#36421=CARTESIAN_POINT('',(0.23094010767585,-0.4,1.1));
#36422=CARTESIAN_POINT('',(0.23094010767585,-0.4,1.6));
#36423=CARTESIAN_POINT('',(-0.230940107675851,-0.4,1.1));
#36424=CARTESIAN_POINT('Origin',(0.461880215351701,0.,1.6));
#36425=CARTESIAN_POINT('',(0.404145188432738,-0.1,1.6));
#36426=CARTESIAN_POINT('',(0.23094010767585,-0.4,1.1));
#36427=CARTESIAN_POINT('Origin',(0.,0.,1.1));
#36428=CARTESIAN_POINT('Origin',(0.833031364477342,-0.43549827301267,1.54));
#36429=CARTESIAN_POINT('',(0.810450538189109,-0.391369295102443,0.94));
#36430=CARTESIAN_POINT('',(0.810450538189109,-0.391369295102443,1.54));
#36431=CARTESIAN_POINT('',(0.810450538189109,-0.391369295102443,0.795));
#36432=CARTESIAN_POINT('',(0.79021682086085,-0.351827196260567,0.94));
#36433=CARTESIAN_POINT('',(0.833031364477342,-0.43549827301267,0.94));
#36434=CARTESIAN_POINT('',(0.79021682086085,-0.351827196260567,1.54));
#36435=CARTESIAN_POINT('',(0.79021682086085,-0.351827196260567,1.54));
#36436=CARTESIAN_POINT('',(0.833031364477342,-0.43549827301267,1.54));
#36437=CARTESIAN_POINT('Origin',(0.835630945491614,-0.381577998747588,1.54));
#36438=CARTESIAN_POINT('',(0.833141326548458,-0.340404950018469,1.54));
#36439=CARTESIAN_POINT('Origin',(0.,0.,1.54));
#36440=CARTESIAN_POINT('',(0.79021682086085,-0.351827196260567,1.54));
#36441=CARTESIAN_POINT('Origin',(0.79021682086085,-0.351827196260567,1.54));
#36442=CARTESIAN_POINT('',(0.833141326548458,-0.340404950018469,0.94));
#36443=CARTESIAN_POINT('',(0.833141326548458,-0.340404950018469,0.795));
#36444=CARTESIAN_POINT('',(0.79021682086085,-0.351827196260567,0.94));
#36445=CARTESIAN_POINT('Origin',(0.835630945491614,-0.381577998747588,0.94));
#36446=CARTESIAN_POINT('Origin',(0.,0.,0.94));
#36447=CARTESIAN_POINT('Origin',(0.583878913461612,-0.736671849886289,1.54));
#36448=CARTESIAN_POINT('',(0.581199174513752,-0.687173573083638,0.94));
#36449=CARTESIAN_POINT('',(0.581199174513752,-0.687173573083638,1.54));
#36450=CARTESIAN_POINT('',(0.581199174513752,-0.687173573083638,0.795));
#36451=CARTESIAN_POINT('',(0.578797974500412,-0.642820274037946,0.94));
#36452=CARTESIAN_POINT('',(0.583878913461612,-0.736671849886289,0.94));
#36453=CARTESIAN_POINT('',(0.578797974500412,-0.642820274037946,1.54));
#36454=CARTESIAN_POINT('',(0.578797974500412,-0.642820274037946,1.54));
#36455=CARTESIAN_POINT('',(0.583878913461612,-0.736671849886289,1.54));
#36456=CARTESIAN_POINT('Origin',(0.625201146677623,-0.689746061962118,1.54));
#36457=CARTESIAN_POINT('',(0.622657307785777,-0.649844502216468,1.54));
#36458=CARTESIAN_POINT('Origin',(0.,0.,1.54));
#36459=CARTESIAN_POINT('',(0.578797974500412,-0.642820274037946,1.54));
#36460=CARTESIAN_POINT('Origin',(0.578797974500412,-0.642820274037946,1.54));
#36461=CARTESIAN_POINT('',(0.622657307785777,-0.649844502216468,0.94));
#36462=CARTESIAN_POINT('',(0.622657307785776,-0.649844502216468,0.795));
#36463=CARTESIAN_POINT('',(0.578797974500412,-0.642820274037946,0.94));
#36464=CARTESIAN_POINT('Origin',(0.625201146677623,-0.689746061962118,0.94));
#36465=CARTESIAN_POINT('Origin',(0.,0.,0.94));
#36466=CARTESIAN_POINT('Origin',(0.233768493934963,-0.910468171460913,1.54));
#36467=CARTESIAN_POINT('',(0.251453193536225,-0.864159297502743,0.94));
#36468=CARTESIAN_POINT('',(0.251453193536225,-0.864159297502743,1.54));
#36469=CARTESIAN_POINT('',(0.251453193536225,-0.864159297502743,0.795));
#36470=CARTESIAN_POINT('',(0.267299700134329,-0.822663886595308,0.94));
#36471=CARTESIAN_POINT('',(0.233768493934963,-0.910468171460913,0.94));
#36472=CARTESIAN_POINT('',(0.267299700134329,-0.822663886595308,1.54));
#36473=CARTESIAN_POINT('',(0.267299700134329,-0.822663886595308,1.54));
#36474=CARTESIAN_POINT('',(0.233768493934963,-0.910468171460913,1.54));
#36475=CARTESIAN_POINT('Origin',(0.28990278672928,-0.866566029028111,1.54));
#36476=CARTESIAN_POINT('',(0.304510183842877,-0.846920036329273,1.54));
#36477=CARTESIAN_POINT('Origin',(0.,0.,1.54));
#36478=CARTESIAN_POINT('',(0.267299700134329,-0.822663886595308,1.54));
#36479=CARTESIAN_POINT('Origin',(0.267299700134329,-0.822663886595308,1.54));
#36480=CARTESIAN_POINT('',(0.304510183842877,-0.846920036329273,0.94));
#36481=CARTESIAN_POINT('',(0.304510183842877,-0.846920036329273,0.795));
#36482=CARTESIAN_POINT('',(0.267299700134329,-0.822663886595308,0.94));
#36483=CARTESIAN_POINT('Origin',(0.28990278672928,-0.866566029028111,0.94));
#36484=CARTESIAN_POINT('Origin',(0.,0.,0.94));
#36485=CARTESIAN_POINT('Origin',(-0.156762621913137,-0.926836274846275,
1.54));
#36486=CARTESIAN_POINT('',(-0.121771328984263,-0.891724028742865,0.94));
#36487=CARTESIAN_POINT('',(-0.121771328984263,-0.891724028742865,1.54));
#36488=CARTESIAN_POINT('',(-0.121771328984263,-0.891724028742865,0.795));
#36489=CARTESIAN_POINT('',(-0.0904171207265202,-0.860261439493557,0.94));
#36490=CARTESIAN_POINT('',(-0.156762621913137,-0.926836274846275,0.94));
#36491=CARTESIAN_POINT('',(-0.0904171207265202,-0.860261439493557,1.54));
#36492=CARTESIAN_POINT('',(-0.0904171207265202,-0.860261439493557,1.54));
#36493=CARTESIAN_POINT('',(-0.156762621913137,-0.926836274846275,1.54));
#36494=CARTESIAN_POINT('Origin',(-0.0980628682092918,-0.899718449893242,
1.54));
#36495=CARTESIAN_POINT('',(-0.0662895172746297,-0.897555402133761,1.54));
#36496=CARTESIAN_POINT('Origin',(0.,0.,1.54));
#36497=CARTESIAN_POINT('',(-0.0904171207265202,-0.860261439493557,1.54));
#36498=CARTESIAN_POINT('Origin',(-0.0904171207265202,-0.860261439493557,
1.54));
#36499=CARTESIAN_POINT('',(-0.0662895172746297,-0.897555402133761,0.94));
#36500=CARTESIAN_POINT('',(-0.0662895172746297,-0.897555402133761,0.795));
#36501=CARTESIAN_POINT('',(-0.0904171207265202,-0.860261439493557,0.94));
#36502=CARTESIAN_POINT('Origin',(-0.0980628682092918,-0.899718449893242,
0.94));
#36503=CARTESIAN_POINT('Origin',(0.,0.,0.94));
#36504=CARTESIAN_POINT('Origin',(-0.520188056288743,-0.782945966267494,
1.54));
#36505=CARTESIAN_POINT('',(-0.473940482465577,-0.765101574354867,0.94));
#36506=CARTESIAN_POINT('',(-0.473940482465577,-0.765101574354867,1.54));
#36507=CARTESIAN_POINT('',(-0.473940482465577,-0.765101574354867,0.795));
#36508=CARTESIAN_POINT('',(-0.4325,-0.749111974273539,0.94));
#36509=CARTESIAN_POINT('',(-0.520188056288743,-0.782945966267494,0.94));
#36510=CARTESIAN_POINT('',(-0.4325,-0.749111974273539,1.54));
#36511=CARTESIAN_POINT('',(-0.4325,-0.749111974273539,1.54));
#36512=CARTESIAN_POINT('',(-0.520188056288743,-0.782945966267494,1.54));
#36513=CARTESIAN_POINT('Origin',(-0.469072562361288,-0.795540514449294,
1.54));
#36514=CARTESIAN_POINT('',(-0.425627158633995,-0.792995284874477,1.54));
#36515=CARTESIAN_POINT('Origin',(0.,0.,1.54));
#36516=CARTESIAN_POINT('',(-0.4325,-0.749111974273539,1.54));
#36517=CARTESIAN_POINT('Origin',(-0.4325,-0.749111974273539,1.54));
#36518=CARTESIAN_POINT('',(-0.425627158633995,-0.792995284874477,0.94));
#36519=CARTESIAN_POINT('',(-0.425627158633995,-0.792995284874477,0.795));
#36520=CARTESIAN_POINT('',(-0.4325,-0.749111974273539,0.94));
#36521=CARTESIAN_POINT('Origin',(-0.469072562361288,-0.795540514449294,
0.94));
#36522=CARTESIAN_POINT('Origin',(0.,0.,0.94));
#36523=CARTESIAN_POINT('Origin',(-0.793668249971894,-0.503677187280257,
1.54));
#36524=CARTESIAN_POINT('',(-0.744161020914479,-0.506186107031317,0.94));
#36525=CARTESIAN_POINT('',(-0.744161020914479,-0.506186107031317,1.54));
#36526=CARTESIAN_POINT('',(-0.744161020914479,-0.506186107031317,0.795));
#36527=CARTESIAN_POINT('',(-0.69979970013433,-0.508434243232989,0.94));
#36528=CARTESIAN_POINT('',(-0.793668249971894,-0.503677187280257,0.94));
#36529=CARTESIAN_POINT('',(-0.69979970013433,-0.508434243232989,1.54));
#36530=CARTESIAN_POINT('',(-0.69979970013433,-0.508434243232989,1.54));
#36531=CARTESIAN_POINT('',(-0.793668249971894,-0.503677187280257,1.54));
#36532=CARTESIAN_POINT('Origin',(-0.746733975053112,-0.551427868822013,
1.54));
#36533=CARTESIAN_POINT('',(-0.711369997564195,-0.551319078724396,1.54));
#36534=CARTESIAN_POINT('Origin',(0.,0.,1.54));
#36535=CARTESIAN_POINT('',(-0.69979970013433,-0.508434243232989,1.54));
#36536=CARTESIAN_POINT('Origin',(-0.69979970013433,-0.508434243232989,1.54));
#36537=CARTESIAN_POINT('',(-0.711369997564195,-0.551319078724396,0.94));
#36538=CARTESIAN_POINT('',(-0.711369997564195,-0.551319078724396,0.795));
#36539=CARTESIAN_POINT('',(-0.69979970013433,-0.508434243232989,0.94));
#36540=CARTESIAN_POINT('Origin',(-0.746733975053112,-0.551427868822013,
0.94));
#36541=CARTESIAN_POINT('Origin',(0.,0.,0.94));
#36542=CARTESIAN_POINT('Origin',(-0.929915992985209,-0.137318046848667,
1.54));
#36543=CARTESIAN_POINT('',(-0.885709358356629,-0.159746463245636,0.94));
#36544=CARTESIAN_POINT('',(-0.885709358356629,-0.159746463245636,1.54));
#36545=CARTESIAN_POINT('',(-0.885709358356629,-0.159746463245636,0.795));
#36546=CARTESIAN_POINT('',(-0.846097674634742,-0.179843612557362,0.94));
#36547=CARTESIAN_POINT('',(-0.929915992985209,-0.137318046848667,0.94));
#36548=CARTESIAN_POINT('',(-0.846097674634742,-0.179843612557362,1.54));
#36549=CARTESIAN_POINT('',(-0.846097674634742,-0.179843612557362,1.54));
#36550=CARTESIAN_POINT('',(-0.929915992985209,-0.137318046848667,1.54));
#36551=CARTESIAN_POINT('Origin',(-0.888006833809975,-0.195051339113508,
1.54));
#36552=CARTESIAN_POINT('',(-0.874110501322002,-0.214314795286275,1.54));
#36553=CARTESIAN_POINT('Origin',(0.,0.,1.54));
#36554=CARTESIAN_POINT('',(-0.846097674634742,-0.179843612557362,1.54));
#36555=CARTESIAN_POINT('Origin',(-0.846097674634742,-0.179843612557362,
1.54));
#36556=CARTESIAN_POINT('',(-0.874110501322002,-0.214314795286275,0.94));
#36557=CARTESIAN_POINT('',(-0.874110501322002,-0.214314795286275,0.795));
#36558=CARTESIAN_POINT('',(-0.846097674634742,-0.179843612557362,0.94));
#36559=CARTESIAN_POINT('Origin',(-0.888006833809975,-0.195051339113508,
0.94));
#36560=CARTESIAN_POINT('Origin',(0.,0.,0.94));
#36561=CARTESIAN_POINT('Origin',(0.901572562361288,0.,1.54));
#36562=CARTESIAN_POINT('',(0.899567641099572,-0.0278937105196098,1.54));
#36563=CARTESIAN_POINT('',(0.899567641099572,0.0278937105196097,1.54));
#36564=CARTESIAN_POINT('Origin',(0.,0.,1.54));
#36565=CARTESIAN_POINT('',(0.865,0.,1.54));
#36566=CARTESIAN_POINT('',(0.938145124722575,-0.0590230883575546,1.54));
#36567=CARTESIAN_POINT('',(0.865,0.,1.54));
#36568=CARTESIAN_POINT('Origin',(0.938145124722575,-0.0590230883575546,
1.54));
#36569=CARTESIAN_POINT('',(0.899567641099572,-0.0278937105196098,0.94));
#36570=CARTESIAN_POINT('',(0.899567641099572,-0.0278937105196099,0.795));
#36571=CARTESIAN_POINT('',(0.865,0.,0.94));
#36572=CARTESIAN_POINT('',(0.938145124722575,-0.0590230883575546,0.94));
#36573=CARTESIAN_POINT('',(0.865,0.,1.54));
#36574=CARTESIAN_POINT('Origin',(0.865,0.,1.54));
#36575=CARTESIAN_POINT('',(0.899567641099572,0.0278937105196097,0.94));
#36576=CARTESIAN_POINT('',(0.899567641099572,0.0278937105196099,0.795));
#36577=CARTESIAN_POINT('',(0.865,0.,0.94));
#36578=CARTESIAN_POINT('Origin',(0.901572562361288,0.,0.94));
#36579=CARTESIAN_POINT('Origin',(0.,0.,0.94));
#36580=CARTESIAN_POINT('Origin',(-0.833031364477342,0.43549827301267,1.54));
#36581=CARTESIAN_POINT('',(-0.810450538189109,0.391369295102443,0.94));
#36582=CARTESIAN_POINT('',(-0.810450538189109,0.391369295102443,1.54));
#36583=CARTESIAN_POINT('',(-0.810450538189109,0.391369295102443,0.795));
#36584=CARTESIAN_POINT('',(-0.79021682086085,0.351827196260567,0.94));
#36585=CARTESIAN_POINT('',(-0.833031364477342,0.43549827301267,0.94));
#36586=CARTESIAN_POINT('',(-0.79021682086085,0.351827196260567,1.54));
#36587=CARTESIAN_POINT('',(-0.79021682086085,0.351827196260567,1.54));
#36588=CARTESIAN_POINT('',(-0.833031364477342,0.43549827301267,1.54));
#36589=CARTESIAN_POINT('Origin',(-0.835630945491614,0.381577998747588,1.54));
#36590=CARTESIAN_POINT('',(-0.833141326548458,0.340404950018469,1.54));
#36591=CARTESIAN_POINT('Origin',(0.,0.,1.54));
#36592=CARTESIAN_POINT('',(-0.79021682086085,0.351827196260567,1.54));
#36593=CARTESIAN_POINT('Origin',(-0.79021682086085,0.351827196260567,1.54));
#36594=CARTESIAN_POINT('',(-0.833141326548458,0.340404950018469,0.94));
#36595=CARTESIAN_POINT('',(-0.833141326548458,0.340404950018469,0.795));
#36596=CARTESIAN_POINT('',(-0.79021682086085,0.351827196260567,0.94));
#36597=CARTESIAN_POINT('Origin',(-0.835630945491614,0.381577998747588,0.94));
#36598=CARTESIAN_POINT('Origin',(0.,0.,0.94));
#36599=CARTESIAN_POINT('Origin',(-0.583878913461612,0.736671849886289,1.54));
#36600=CARTESIAN_POINT('',(-0.581199174513752,0.687173573083638,0.94));
#36601=CARTESIAN_POINT('',(-0.581199174513752,0.687173573083638,1.54));
#36602=CARTESIAN_POINT('',(-0.581199174513752,0.687173573083638,0.795));
#36603=CARTESIAN_POINT('',(-0.578797974500412,0.642820274037946,0.94));
#36604=CARTESIAN_POINT('',(-0.583878913461612,0.736671849886289,0.94));
#36605=CARTESIAN_POINT('',(-0.578797974500412,0.642820274037946,1.54));
#36606=CARTESIAN_POINT('',(-0.578797974500412,0.642820274037946,1.54));
#36607=CARTESIAN_POINT('',(-0.583878913461612,0.736671849886289,1.54));
#36608=CARTESIAN_POINT('Origin',(-0.625201146677624,0.689746061962118,1.54));
#36609=CARTESIAN_POINT('',(-0.622657307785776,0.649844502216468,1.54));
#36610=CARTESIAN_POINT('Origin',(0.,0.,1.54));
#36611=CARTESIAN_POINT('',(-0.578797974500412,0.642820274037946,1.54));
#36612=CARTESIAN_POINT('Origin',(-0.578797974500412,0.642820274037946,1.54));
#36613=CARTESIAN_POINT('',(-0.622657307785776,0.649844502216468,0.94));
#36614=CARTESIAN_POINT('',(-0.622657307785776,0.649844502216468,0.795));
#36615=CARTESIAN_POINT('',(-0.578797974500412,0.642820274037946,0.94));
#36616=CARTESIAN_POINT('Origin',(-0.625201146677624,0.689746061962118,0.94));
#36617=CARTESIAN_POINT('Origin',(0.,0.,0.94));
#36618=CARTESIAN_POINT('Origin',(-0.233768493934964,0.910468171460913,1.54));
#36619=CARTESIAN_POINT('',(-0.251453193536226,0.864159297502743,0.94));
#36620=CARTESIAN_POINT('',(-0.251453193536226,0.864159297502743,1.54));
#36621=CARTESIAN_POINT('',(-0.251453193536226,0.864159297502743,0.795));
#36622=CARTESIAN_POINT('',(-0.267299700134329,0.822663886595308,0.94));
#36623=CARTESIAN_POINT('',(-0.233768493934964,0.910468171460913,0.94));
#36624=CARTESIAN_POINT('',(-0.267299700134329,0.822663886595308,1.54));
#36625=CARTESIAN_POINT('',(-0.267299700134329,0.822663886595308,1.54));
#36626=CARTESIAN_POINT('',(-0.233768493934964,0.910468171460913,1.54));
#36627=CARTESIAN_POINT('Origin',(-0.28990278672928,0.866566029028111,1.54));
#36628=CARTESIAN_POINT('',(-0.304510183842877,0.846920036329273,1.54));
#36629=CARTESIAN_POINT('Origin',(0.,0.,1.54));
#36630=CARTESIAN_POINT('',(-0.267299700134329,0.822663886595308,1.54));
#36631=CARTESIAN_POINT('Origin',(-0.267299700134329,0.822663886595308,1.54));
#36632=CARTESIAN_POINT('',(-0.304510183842877,0.846920036329273,0.94));
#36633=CARTESIAN_POINT('',(-0.304510183842877,0.846920036329273,0.795));
#36634=CARTESIAN_POINT('',(-0.267299700134329,0.822663886595308,0.94));
#36635=CARTESIAN_POINT('Origin',(-0.28990278672928,0.866566029028111,0.94));
#36636=CARTESIAN_POINT('Origin',(0.,0.,0.94));
#36637=CARTESIAN_POINT('Origin',(0.156762621913136,0.926836274846275,1.54));
#36638=CARTESIAN_POINT('',(0.121771328984262,0.891724028742865,0.94));
#36639=CARTESIAN_POINT('',(0.121771328984262,0.891724028742865,1.54));
#36640=CARTESIAN_POINT('',(0.121771328984263,0.891724028742865,0.795));
#36641=CARTESIAN_POINT('',(0.0904171207265202,0.860261439493556,0.94));
#36642=CARTESIAN_POINT('',(0.156762621913136,0.926836274846275,0.94));
#36643=CARTESIAN_POINT('',(0.0904171207265202,0.860261439493556,1.54));
#36644=CARTESIAN_POINT('',(0.0904171207265202,0.860261439493556,1.54));
#36645=CARTESIAN_POINT('',(0.156762621913136,0.926836274846275,1.54));
#36646=CARTESIAN_POINT('Origin',(0.0980628682092919,0.899718449893242,1.54));
#36647=CARTESIAN_POINT('',(0.0662895172746301,0.897555402133761,1.54));
#36648=CARTESIAN_POINT('Origin',(0.,0.,1.54));
#36649=CARTESIAN_POINT('',(0.0904171207265202,0.860261439493556,1.54));
#36650=CARTESIAN_POINT('Origin',(0.0904171207265202,0.860261439493556,1.54));
#36651=CARTESIAN_POINT('',(0.0662895172746301,0.897555402133761,0.94));
#36652=CARTESIAN_POINT('',(0.0662895172746301,0.897555402133761,0.795));
#36653=CARTESIAN_POINT('',(0.0904171207265202,0.860261439493556,0.94));
#36654=CARTESIAN_POINT('Origin',(0.0980628682092919,0.899718449893242,0.94));
#36655=CARTESIAN_POINT('Origin',(0.,0.,0.94));
#36656=CARTESIAN_POINT('Origin',(0.520188056288743,0.782945966267494,1.54));
#36657=CARTESIAN_POINT('',(0.473940482465577,0.765101574354867,0.94));
#36658=CARTESIAN_POINT('',(0.473940482465577,0.765101574354867,1.54));
#36659=CARTESIAN_POINT('',(0.473940482465577,0.765101574354867,0.795));
#36660=CARTESIAN_POINT('',(0.4325,0.749111974273539,0.94));
#36661=CARTESIAN_POINT('',(0.520188056288743,0.782945966267494,0.94));
#36662=CARTESIAN_POINT('',(0.4325,0.749111974273539,1.54));
#36663=CARTESIAN_POINT('',(0.4325,0.749111974273539,1.54));
#36664=CARTESIAN_POINT('',(0.520188056288743,0.782945966267494,1.54));
#36665=CARTESIAN_POINT('Origin',(0.469072562361288,0.795540514449294,1.54));
#36666=CARTESIAN_POINT('',(0.425627158633995,0.792995284874477,1.54));
#36667=CARTESIAN_POINT('Origin',(0.,0.,1.54));
#36668=CARTESIAN_POINT('',(0.4325,0.749111974273539,1.54));
#36669=CARTESIAN_POINT('Origin',(0.4325,0.749111974273539,1.54));
#36670=CARTESIAN_POINT('',(0.425627158633995,0.792995284874477,0.94));
#36671=CARTESIAN_POINT('',(0.425627158633995,0.792995284874477,0.795));
#36672=CARTESIAN_POINT('',(0.4325,0.749111974273539,0.94));
#36673=CARTESIAN_POINT('Origin',(0.469072562361288,0.795540514449294,0.94));
#36674=CARTESIAN_POINT('Origin',(0.,0.,0.94));
#36675=CARTESIAN_POINT('Origin',(0.793668249971894,0.503677187280257,1.54));
#36676=CARTESIAN_POINT('',(0.744161020914479,0.506186107031317,0.94));
#36677=CARTESIAN_POINT('',(0.744161020914479,0.506186107031317,1.54));
#36678=CARTESIAN_POINT('',(0.744161020914479,0.506186107031317,0.795));
#36679=CARTESIAN_POINT('',(0.69979970013433,0.508434243232989,0.94));
#36680=CARTESIAN_POINT('',(0.793668249971894,0.503677187280257,0.94));
#36681=CARTESIAN_POINT('',(0.69979970013433,0.508434243232989,1.54));
#36682=CARTESIAN_POINT('',(0.69979970013433,0.508434243232989,1.54));
#36683=CARTESIAN_POINT('',(0.793668249971894,0.503677187280257,1.54));
#36684=CARTESIAN_POINT('Origin',(0.746733975053112,0.551427868822013,1.54));
#36685=CARTESIAN_POINT('',(0.711369997564195,0.551319078724396,1.54));
#36686=CARTESIAN_POINT('Origin',(0.,0.,1.54));
#36687=CARTESIAN_POINT('',(0.69979970013433,0.508434243232989,1.54));
#36688=CARTESIAN_POINT('Origin',(0.69979970013433,0.508434243232989,1.54));
#36689=CARTESIAN_POINT('',(0.711369997564195,0.551319078724396,0.94));
#36690=CARTESIAN_POINT('',(0.711369997564195,0.551319078724396,0.795));
#36691=CARTESIAN_POINT('',(0.69979970013433,0.508434243232989,0.94));
#36692=CARTESIAN_POINT('Origin',(0.746733975053112,0.551427868822013,0.94));
#36693=CARTESIAN_POINT('Origin',(0.,0.,0.94));
#36694=CARTESIAN_POINT('Origin',(0.929915992985209,0.137318046848667,1.54));
#36695=CARTESIAN_POINT('',(0.885709358356629,0.159746463245636,0.94));
#36696=CARTESIAN_POINT('',(0.885709358356629,0.159746463245636,1.54));
#36697=CARTESIAN_POINT('',(0.885709358356629,0.159746463245636,0.795));
#36698=CARTESIAN_POINT('',(0.846097674634742,0.179843612557362,0.94));
#36699=CARTESIAN_POINT('',(0.929915992985209,0.137318046848667,0.94));
#36700=CARTESIAN_POINT('',(0.846097674634742,0.179843612557362,1.54));
#36701=CARTESIAN_POINT('',(0.846097674634742,0.179843612557362,1.54));
#36702=CARTESIAN_POINT('',(0.929915992985209,0.137318046848667,1.54));
#36703=CARTESIAN_POINT('Origin',(0.888006833809975,0.195051339113508,1.54));
#36704=CARTESIAN_POINT('',(0.874110501322002,0.214314795286275,1.54));
#36705=CARTESIAN_POINT('Origin',(0.,0.,1.54));
#36706=CARTESIAN_POINT('',(0.846097674634742,0.179843612557362,1.54));
#36707=CARTESIAN_POINT('Origin',(0.846097674634742,0.179843612557362,1.54));
#36708=CARTESIAN_POINT('',(0.874110501322002,0.214314795286275,0.94));
#36709=CARTESIAN_POINT('',(0.874110501322002,0.214314795286275,0.795));
#36710=CARTESIAN_POINT('',(0.846097674634742,0.179843612557362,0.94));
#36711=CARTESIAN_POINT('Origin',(0.888006833809975,0.195051339113508,0.94));
#36712=CARTESIAN_POINT('Origin',(0.,0.,0.94));
#36713=CARTESIAN_POINT('Origin',(0.881045070122378,0.327657724482506,1.54));
#36714=CARTESIAN_POINT('',(0.833141326548458,0.340404950018469,0.94));
#36715=CARTESIAN_POINT('',(0.833141326548458,0.340404950018469,1.54));
#36716=CARTESIAN_POINT('',(0.833141326548458,0.340404950018469,0.795));
#36717=CARTESIAN_POINT('',(0.79021682086085,0.351827196260567,0.94));
#36718=CARTESIAN_POINT('',(0.881045070122378,0.327657724482506,0.94));
#36719=CARTESIAN_POINT('',(0.79021682086085,0.351827196260567,1.54));
#36720=CARTESIAN_POINT('',(0.79021682086085,0.351827196260567,1.54));
#36721=CARTESIAN_POINT('',(0.881045070122378,0.327657724482506,1.54));
#36722=CARTESIAN_POINT('Origin',(0.835630945491614,0.381577998747588,1.54));
#36723=CARTESIAN_POINT('',(0.810450538189109,0.391369295102443,1.54));
#36724=CARTESIAN_POINT('Origin',(0.,0.,1.54));
#36725=CARTESIAN_POINT('',(0.79021682086085,0.351827196260567,1.54));
#36726=CARTESIAN_POINT('Origin',(0.79021682086085,0.351827196260567,1.54));
#36727=CARTESIAN_POINT('',(0.810450538189109,0.391369295102443,0.94));
#36728=CARTESIAN_POINT('',(0.810450538189109,0.391369295102443,0.795));
#36729=CARTESIAN_POINT('',(0.79021682086085,0.351827196260567,0.94));
#36730=CARTESIAN_POINT('Origin',(0.835630945491614,0.381577998747588,0.94));
#36731=CARTESIAN_POINT('Origin',(0.,0.,0.94));
#36732=CARTESIAN_POINT('Origin',(0.671604318854835,0.657683540082563,1.54));
#36733=CARTESIAN_POINT('',(0.622657307785777,0.649844502216468,0.94));
#36734=CARTESIAN_POINT('',(0.622657307785777,0.649844502216468,1.54));
#36735=CARTESIAN_POINT('',(0.622657307785777,0.649844502216468,0.795));
#36736=CARTESIAN_POINT('',(0.578797974500412,0.642820274037946,0.94));
#36737=CARTESIAN_POINT('',(0.671604318854835,0.657683540082563,0.94));
#36738=CARTESIAN_POINT('',(0.578797974500412,0.642820274037946,1.54));
#36739=CARTESIAN_POINT('',(0.578797974500412,0.642820274037946,1.54));
#36740=CARTESIAN_POINT('',(0.671604318854835,0.657683540082563,1.54));
#36741=CARTESIAN_POINT('Origin',(0.625201146677624,0.689746061962118,1.54));
#36742=CARTESIAN_POINT('',(0.581199174513752,0.687173573083638,1.54));
#36743=CARTESIAN_POINT('Origin',(0.,0.,1.54));
#36744=CARTESIAN_POINT('',(0.578797974500412,0.642820274037946,1.54));
#36745=CARTESIAN_POINT('Origin',(0.578797974500412,0.642820274037946,1.54));
#36746=CARTESIAN_POINT('',(0.581199174513752,0.687173573083638,0.94));
#36747=CARTESIAN_POINT('',(0.581199174513752,0.687173573083638,0.795));
#36748=CARTESIAN_POINT('',(0.578797974500412,0.642820274037946,0.94));
#36749=CARTESIAN_POINT('Origin',(0.625201146677624,0.689746061962118,0.94));
#36750=CARTESIAN_POINT('Origin',(0.,0.,0.94));
#36751=CARTESIAN_POINT('Origin',(0.346037079523597,0.873989896734956,1.54));
#36752=CARTESIAN_POINT('',(0.304510183842877,0.846920036329273,0.94));
#36753=CARTESIAN_POINT('',(0.304510183842877,0.846920036329273,1.54));
#36754=CARTESIAN_POINT('',(0.304510183842877,0.846920036329273,0.795));
#36755=CARTESIAN_POINT('',(0.26729970013433,0.822663886595308,0.94));
#36756=CARTESIAN_POINT('',(0.346037079523597,0.873989896734956,0.94));
#36757=CARTESIAN_POINT('',(0.26729970013433,0.822663886595308,1.54));
#36758=CARTESIAN_POINT('',(0.26729970013433,0.822663886595308,1.54));
#36759=CARTESIAN_POINT('',(0.346037079523597,0.873989896734956,1.54));
#36760=CARTESIAN_POINT('Origin',(0.28990278672928,0.866566029028111,1.54));
#36761=CARTESIAN_POINT('',(0.251453193536226,0.864159297502743,1.54));
#36762=CARTESIAN_POINT('Origin',(0.,0.,1.54));
#36763=CARTESIAN_POINT('',(0.26729970013433,0.822663886595308,1.54));
#36764=CARTESIAN_POINT('Origin',(0.26729970013433,0.822663886595308,1.54));
#36765=CARTESIAN_POINT('',(0.251453193536226,0.864159297502743,0.94));
#36766=CARTESIAN_POINT('',(0.251453193536226,0.864159297502743,0.795));
#36767=CARTESIAN_POINT('',(0.26729970013433,0.822663886595308,0.94));
#36768=CARTESIAN_POINT('Origin',(0.28990278672928,0.866566029028111,0.94));
#36769=CARTESIAN_POINT('Origin',(0.,0.,0.94));
#36770=CARTESIAN_POINT('Origin',(-0.0393631145054476,0.939175460292927,
1.54));
#36771=CARTESIAN_POINT('',(-0.0662895172746301,0.89755540213376,0.94));
#36772=CARTESIAN_POINT('',(-0.0662895172746301,0.89755540213376,1.54));
#36773=CARTESIAN_POINT('',(-0.0662895172746301,0.897555402133761,0.795));
#36774=CARTESIAN_POINT('',(-0.0904171207265203,0.860261439493556,0.94));
#36775=CARTESIAN_POINT('',(-0.0393631145054476,0.939175460292927,0.94));
#36776=CARTESIAN_POINT('',(-0.0904171207265203,0.860261439493556,1.54));
#36777=CARTESIAN_POINT('',(-0.0904171207265203,0.860261439493556,1.54));
#36778=CARTESIAN_POINT('',(-0.0393631145054476,0.939175460292927,1.54));
#36779=CARTESIAN_POINT('Origin',(-0.0980628682092919,0.899718449893242,
1.54));
#36780=CARTESIAN_POINT('',(-0.121771328984263,0.891724028742865,1.54));
#36781=CARTESIAN_POINT('Origin',(0.,0.,1.54));
#36782=CARTESIAN_POINT('',(-0.0904171207265203,0.860261439493556,1.54));
#36783=CARTESIAN_POINT('Origin',(-0.0904171207265203,0.860261439493556,
1.54));
#36784=CARTESIAN_POINT('',(-0.121771328984263,0.891724028742865,0.94));
#36785=CARTESIAN_POINT('',(-0.121771328984263,0.891724028742865,0.795));
#36786=CARTESIAN_POINT('',(-0.0904171207265203,0.860261439493556,0.94));
#36787=CARTESIAN_POINT('Origin',(-0.0980628682092919,0.899718449893242,
0.94));
#36788=CARTESIAN_POINT('Origin',(0.,0.,0.94));
#36789=CARTESIAN_POINT('Origin',(-0.417957068433832,0.841969054625048,1.54));
#36790=CARTESIAN_POINT('',(-0.425627158633995,0.792995284874477,0.94));
#36791=CARTESIAN_POINT('',(-0.425627158633995,0.792995284874477,1.54));
#36792=CARTESIAN_POINT('',(-0.425627158633995,0.792995284874477,0.795));
#36793=CARTESIAN_POINT('',(-0.4325,0.749111974273539,0.94));
#36794=CARTESIAN_POINT('',(-0.417957068433832,0.841969054625048,0.94));
#36795=CARTESIAN_POINT('',(-0.4325,0.749111974273539,1.54));
#36796=CARTESIAN_POINT('',(-0.4325,0.749111974273539,1.54));
#36797=CARTESIAN_POINT('',(-0.417957068433832,0.841969054625048,1.54));
#36798=CARTESIAN_POINT('Origin',(-0.469072562361288,0.795540514449294,1.54));
#36799=CARTESIAN_POINT('',(-0.473940482465577,0.765101574354867,1.54));
#36800=CARTESIAN_POINT('Origin',(0.,0.,1.54));
#36801=CARTESIAN_POINT('',(-0.4325,0.749111974273539,1.54));
#36802=CARTESIAN_POINT('Origin',(-0.4325,0.749111974273539,1.54));
#36803=CARTESIAN_POINT('',(-0.473940482465577,0.765101574354867,0.94));
#36804=CARTESIAN_POINT('',(-0.473940482465577,0.765101574354867,0.795));
#36805=CARTESIAN_POINT('',(-0.4325,0.749111974273539,0.94));
#36806=CARTESIAN_POINT('Origin',(-0.469072562361288,0.795540514449294,0.94));
#36807=CARTESIAN_POINT('Origin',(0.,0.,0.94));
#36808=CARTESIAN_POINT('Origin',(-0.724282448209242,0.599178550363768,1.54));
#36809=CARTESIAN_POINT('',(-0.711369997564195,0.551319078724396,0.94));
#36810=CARTESIAN_POINT('',(-0.711369997564195,0.551319078724396,1.54));
#36811=CARTESIAN_POINT('',(-0.711369997564195,0.551319078724396,0.795));
#36812=CARTESIAN_POINT('',(-0.699799700134329,0.508434243232989,0.94));
#36813=CARTESIAN_POINT('',(-0.724282448209242,0.599178550363768,0.94));
#36814=CARTESIAN_POINT('',(-0.699799700134329,0.508434243232989,1.54));
#36815=CARTESIAN_POINT('',(-0.699799700134329,0.508434243232989,1.54));
#36816=CARTESIAN_POINT('',(-0.724282448209242,0.599178550363768,1.54));
#36817=CARTESIAN_POINT('Origin',(-0.746733975053112,0.551427868822013,1.54));
#36818=CARTESIAN_POINT('',(-0.744161020914479,0.506186107031317,1.54));
#36819=CARTESIAN_POINT('Origin',(0.,0.,1.54));
#36820=CARTESIAN_POINT('',(-0.699799700134329,0.508434243232989,1.54));
#36821=CARTESIAN_POINT('Origin',(-0.699799700134329,0.508434243232989,1.54));
#36822=CARTESIAN_POINT('',(-0.744161020914479,0.506186107031317,0.94));
#36823=CARTESIAN_POINT('',(-0.744161020914479,0.506186107031317,0.795));
#36824=CARTESIAN_POINT('',(-0.699799700134329,0.508434243232989,0.94));
#36825=CARTESIAN_POINT('Origin',(-0.746733975053112,0.551427868822013,0.94));
#36826=CARTESIAN_POINT('Origin',(0.,0.,0.94));
#36827=CARTESIAN_POINT('Origin',(-0.905372812789799,0.25278463137835,1.54));
#36828=CARTESIAN_POINT('',(-0.874110501322002,0.214314795286275,0.94));
#36829=CARTESIAN_POINT('',(-0.874110501322002,0.214314795286275,1.54));
#36830=CARTESIAN_POINT('',(-0.874110501322002,0.214314795286275,0.795));
#36831=CARTESIAN_POINT('',(-0.846097674634742,0.179843612557362,0.94));
#36832=CARTESIAN_POINT('',(-0.905372812789799,0.25278463137835,0.94));
#36833=CARTESIAN_POINT('',(-0.846097674634742,0.179843612557362,1.54));
#36834=CARTESIAN_POINT('',(-0.846097674634742,0.179843612557362,1.54));
#36835=CARTESIAN_POINT('',(-0.905372812789799,0.25278463137835,1.54));
#36836=CARTESIAN_POINT('Origin',(-0.888006833809975,0.195051339113509,1.54));
#36837=CARTESIAN_POINT('',(-0.885709358356629,0.159746463245636,1.54));
#36838=CARTESIAN_POINT('Origin',(0.,0.,1.54));
#36839=CARTESIAN_POINT('',(-0.846097674634742,0.179843612557362,1.54));
#36840=CARTESIAN_POINT('Origin',(-0.846097674634742,0.179843612557362,1.54));
#36841=CARTESIAN_POINT('',(-0.885709358356629,0.159746463245636,0.94));
#36842=CARTESIAN_POINT('',(-0.885709358356629,0.159746463245636,0.795));
#36843=CARTESIAN_POINT('',(-0.846097674634742,0.179843612557362,0.94));
#36844=CARTESIAN_POINT('Origin',(-0.888006833809975,0.195051339113509,0.94));
#36845=CARTESIAN_POINT('Origin',(0.,0.,0.94));
#36846=CARTESIAN_POINT('Origin',(-0.938145124722575,0.0590230883575544,
1.54));
#36847=CARTESIAN_POINT('',(-0.899567641099572,0.0278937105196099,0.94));
#36848=CARTESIAN_POINT('',(-0.899567641099572,0.0278937105196099,1.54));
#36849=CARTESIAN_POINT('',(-0.899567641099572,0.0278937105196097,0.795));
#36850=CARTESIAN_POINT('',(-0.865,1.05931948126246E-16,0.94));
#36851=CARTESIAN_POINT('',(-0.938145124722575,0.0590230883575544,0.94));
#36852=CARTESIAN_POINT('',(-0.865,1.05931948126246E-16,1.54));
#36853=CARTESIAN_POINT('',(-0.865,1.05931948126246E-16,1.54));
#36854=CARTESIAN_POINT('',(-0.938145124722575,0.0590230883575544,1.54));
#36855=CARTESIAN_POINT('Origin',(-0.901572562361288,-9.71445146547012E-17,
1.54));
#36856=CARTESIAN_POINT('',(-0.9,-1.10218211923262E-16,1.54));
#36857=CARTESIAN_POINT('Origin',(0.,0.,1.54));
#36858=CARTESIAN_POINT('',(-0.899567641099572,-0.0278937105196098,1.54));
#36859=CARTESIAN_POINT('',(-0.865,1.05931948126246E-16,1.54));
#36860=CARTESIAN_POINT('Origin',(0.,0.,1.54));
#36861=CARTESIAN_POINT('Origin',(-0.865,1.05931948126246E-16,1.54));
#36862=CARTESIAN_POINT('',(-0.899567641099572,-0.0278937105196098,0.94));
#36863=CARTESIAN_POINT('',(-0.899567641099572,-0.0278937105196098,0.795));
#36864=CARTESIAN_POINT('',(-0.865,1.05931948126246E-16,0.94));
#36865=CARTESIAN_POINT('Origin',(-0.901572562361288,-9.71445146547012E-17,
0.94));
#36866=CARTESIAN_POINT('',(-0.9,-1.10218211923262E-16,0.94));
#36867=CARTESIAN_POINT('Origin',(0.,0.,0.94));
#36868=CARTESIAN_POINT('Origin',(0.,0.,0.94));
#36869=CARTESIAN_POINT('Origin',(-0.881045070122378,-0.327657724482506,
1.54));
#36870=CARTESIAN_POINT('',(-0.833141326548458,-0.340404950018469,0.94));
#36871=CARTESIAN_POINT('',(-0.833141326548458,-0.340404950018469,1.54));
#36872=CARTESIAN_POINT('',(-0.833141326548458,-0.340404950018469,0.795));
#36873=CARTESIAN_POINT('',(-0.79021682086085,-0.351827196260567,0.94));
#36874=CARTESIAN_POINT('',(-0.881045070122378,-0.327657724482506,0.94));
#36875=CARTESIAN_POINT('',(-0.79021682086085,-0.351827196260567,1.54));
#36876=CARTESIAN_POINT('',(-0.79021682086085,-0.351827196260567,1.54));
#36877=CARTESIAN_POINT('',(-0.881045070122378,-0.327657724482506,1.54));
#36878=CARTESIAN_POINT('Origin',(-0.835630945491614,-0.381577998747588,
1.54));
#36879=CARTESIAN_POINT('',(-0.810450538189109,-0.391369295102443,1.54));
#36880=CARTESIAN_POINT('Origin',(0.,0.,1.54));
#36881=CARTESIAN_POINT('',(-0.79021682086085,-0.351827196260567,1.54));
#36882=CARTESIAN_POINT('Origin',(-0.79021682086085,-0.351827196260567,1.54));
#36883=CARTESIAN_POINT('',(-0.810450538189109,-0.391369295102443,0.94));
#36884=CARTESIAN_POINT('',(-0.810450538189109,-0.391369295102443,0.795));
#36885=CARTESIAN_POINT('',(-0.79021682086085,-0.351827196260567,0.94));
#36886=CARTESIAN_POINT('Origin',(-0.835630945491614,-0.381577998747588,
0.94));
#36887=CARTESIAN_POINT('Origin',(0.,0.,0.94));
#36888=CARTESIAN_POINT('Origin',(-0.671604318854835,-0.657683540082563,
1.54));
#36889=CARTESIAN_POINT('',(-0.622657307785777,-0.649844502216468,0.94));
#36890=CARTESIAN_POINT('',(-0.622657307785777,-0.649844502216468,1.54));
#36891=CARTESIAN_POINT('',(-0.622657307785777,-0.649844502216468,0.795));
#36892=CARTESIAN_POINT('',(-0.578797974500412,-0.642820274037946,0.94));
#36893=CARTESIAN_POINT('',(-0.671604318854835,-0.657683540082563,0.94));
#36894=CARTESIAN_POINT('',(-0.578797974500412,-0.642820274037946,1.54));
#36895=CARTESIAN_POINT('',(-0.578797974500412,-0.642820274037946,1.54));
#36896=CARTESIAN_POINT('',(-0.671604318854835,-0.657683540082563,1.54));
#36897=CARTESIAN_POINT('Origin',(-0.625201146677624,-0.689746061962118,
1.54));
#36898=CARTESIAN_POINT('',(-0.581199174513752,-0.687173573083637,1.54));
#36899=CARTESIAN_POINT('Origin',(0.,0.,1.54));
#36900=CARTESIAN_POINT('',(-0.578797974500412,-0.642820274037946,1.54));
#36901=CARTESIAN_POINT('Origin',(-0.578797974500412,-0.642820274037946,
1.54));
#36902=CARTESIAN_POINT('',(-0.581199174513752,-0.687173573083637,0.94));
#36903=CARTESIAN_POINT('',(-0.581199174513752,-0.687173573083637,0.795));
#36904=CARTESIAN_POINT('',(-0.578797974500412,-0.642820274037946,0.94));
#36905=CARTESIAN_POINT('Origin',(-0.625201146677624,-0.689746061962118,
0.94));
#36906=CARTESIAN_POINT('Origin',(0.,0.,0.94));
#36907=CARTESIAN_POINT('Origin',(-0.346037079523597,-0.873989896734956,
1.54));
#36908=CARTESIAN_POINT('',(-0.304510183842877,-0.846920036329273,0.94));
#36909=CARTESIAN_POINT('',(-0.304510183842877,-0.846920036329273,1.54));
#36910=CARTESIAN_POINT('',(-0.304510183842877,-0.846920036329273,0.795));
#36911=CARTESIAN_POINT('',(-0.26729970013433,-0.822663886595308,0.94));
#36912=CARTESIAN_POINT('',(-0.346037079523597,-0.873989896734956,0.94));
#36913=CARTESIAN_POINT('',(-0.26729970013433,-0.822663886595308,1.54));
#36914=CARTESIAN_POINT('',(-0.26729970013433,-0.822663886595308,1.54));
#36915=CARTESIAN_POINT('',(-0.346037079523597,-0.873989896734956,1.54));
#36916=CARTESIAN_POINT('Origin',(-0.289902786729281,-0.866566029028111,
1.54));
#36917=CARTESIAN_POINT('',(-0.251453193536226,-0.864159297502742,1.54));
#36918=CARTESIAN_POINT('Origin',(0.,0.,1.54));
#36919=CARTESIAN_POINT('',(-0.26729970013433,-0.822663886595308,1.54));
#36920=CARTESIAN_POINT('Origin',(-0.26729970013433,-0.822663886595308,1.54));
#36921=CARTESIAN_POINT('',(-0.251453193536226,-0.864159297502742,0.94));
#36922=CARTESIAN_POINT('',(-0.251453193536226,-0.864159297502743,0.795));
#36923=CARTESIAN_POINT('',(-0.26729970013433,-0.822663886595308,0.94));
#36924=CARTESIAN_POINT('Origin',(-0.289902786729281,-0.866566029028111,
0.94));
#36925=CARTESIAN_POINT('Origin',(0.,0.,0.94));
#36926=CARTESIAN_POINT('Origin',(0.0393631145054475,-0.939175460292927,
1.54));
#36927=CARTESIAN_POINT('',(0.0662895172746297,-0.897555402133761,0.94));
#36928=CARTESIAN_POINT('',(0.0662895172746297,-0.897555402133761,1.54));
#36929=CARTESIAN_POINT('',(0.0662895172746297,-0.897555402133761,0.795));
#36930=CARTESIAN_POINT('',(0.0904171207265198,-0.860261439493557,0.94));
#36931=CARTESIAN_POINT('',(0.0393631145054475,-0.939175460292927,0.94));
#36932=CARTESIAN_POINT('',(0.0904171207265198,-0.860261439493557,1.54));
#36933=CARTESIAN_POINT('',(0.0904171207265198,-0.860261439493557,1.54));
#36934=CARTESIAN_POINT('',(0.0393631145054475,-0.939175460292927,1.54));
#36935=CARTESIAN_POINT('Origin',(0.0980628682092919,-0.899718449893242,
1.54));
#36936=CARTESIAN_POINT('',(0.121771328984262,-0.891724028742865,1.54));
#36937=CARTESIAN_POINT('Origin',(0.,0.,1.54));
#36938=CARTESIAN_POINT('',(0.0904171207265198,-0.860261439493557,1.54));
#36939=CARTESIAN_POINT('Origin',(0.0904171207265198,-0.860261439493557,
1.54));
#36940=CARTESIAN_POINT('',(0.121771328984262,-0.891724028742865,0.94));
#36941=CARTESIAN_POINT('',(0.121771328984262,-0.891724028742865,0.795));
#36942=CARTESIAN_POINT('',(0.0904171207265198,-0.860261439493557,0.94));
#36943=CARTESIAN_POINT('Origin',(0.0980628682092919,-0.899718449893242,
0.94));
#36944=CARTESIAN_POINT('Origin',(0.,0.,0.94));
#36945=CARTESIAN_POINT('Origin',(0.417957068433832,-0.841969054625048,1.54));
#36946=CARTESIAN_POINT('',(0.425627158633994,-0.792995284874477,0.94));
#36947=CARTESIAN_POINT('',(0.425627158633994,-0.792995284874477,1.54));
#36948=CARTESIAN_POINT('',(0.425627158633994,-0.792995284874477,0.795));
#36949=CARTESIAN_POINT('',(0.4325,-0.749111974273539,0.94));
#36950=CARTESIAN_POINT('',(0.417957068433832,-0.841969054625048,0.94));
#36951=CARTESIAN_POINT('',(0.4325,-0.749111974273539,1.54));
#36952=CARTESIAN_POINT('',(0.4325,-0.749111974273539,1.54));
#36953=CARTESIAN_POINT('',(0.417957068433832,-0.841969054625048,1.54));
#36954=CARTESIAN_POINT('Origin',(0.469072562361288,-0.795540514449294,1.54));
#36955=CARTESIAN_POINT('',(0.473940482465578,-0.765101574354867,1.54));
#36956=CARTESIAN_POINT('Origin',(0.,0.,1.54));
#36957=CARTESIAN_POINT('',(0.4325,-0.749111974273539,1.54));
#36958=CARTESIAN_POINT('Origin',(0.4325,-0.749111974273539,1.54));
#36959=CARTESIAN_POINT('',(0.473940482465578,-0.765101574354867,0.94));
#36960=CARTESIAN_POINT('',(0.473940482465578,-0.765101574354867,0.795));
#36961=CARTESIAN_POINT('',(0.4325,-0.749111974273539,0.94));
#36962=CARTESIAN_POINT('Origin',(0.469072562361288,-0.795540514449294,0.94));
#36963=CARTESIAN_POINT('Origin',(0.,0.,0.94));
#36964=CARTESIAN_POINT('Origin',(0.724282448209242,-0.599178550363769,1.54));
#36965=CARTESIAN_POINT('',(0.711369997564195,-0.551319078724397,0.94));
#36966=CARTESIAN_POINT('',(0.711369997564195,-0.551319078724397,1.54));
#36967=CARTESIAN_POINT('',(0.711369997564195,-0.551319078724397,0.795));
#36968=CARTESIAN_POINT('',(0.699799700134329,-0.508434243232989,0.94));
#36969=CARTESIAN_POINT('',(0.724282448209242,-0.599178550363769,0.94));
#36970=CARTESIAN_POINT('',(0.699799700134329,-0.508434243232989,1.54));
#36971=CARTESIAN_POINT('',(0.699799700134329,-0.508434243232989,1.54));
#36972=CARTESIAN_POINT('',(0.724282448209242,-0.599178550363769,1.54));
#36973=CARTESIAN_POINT('Origin',(0.746733975053112,-0.551427868822013,1.54));
#36974=CARTESIAN_POINT('',(0.744161020914479,-0.506186107031317,1.54));
#36975=CARTESIAN_POINT('Origin',(0.,0.,1.54));
#36976=CARTESIAN_POINT('',(0.699799700134329,-0.508434243232989,1.54));
#36977=CARTESIAN_POINT('Origin',(0.699799700134329,-0.508434243232989,1.54));
#36978=CARTESIAN_POINT('',(0.744161020914479,-0.506186107031317,0.94));
#36979=CARTESIAN_POINT('',(0.744161020914479,-0.506186107031317,0.795));
#36980=CARTESIAN_POINT('',(0.699799700134329,-0.508434243232989,0.94));
#36981=CARTESIAN_POINT('Origin',(0.746733975053112,-0.551427868822013,0.94));
#36982=CARTESIAN_POINT('Origin',(0.,0.,0.94));
#36983=CARTESIAN_POINT('Origin',(0.905372812789799,-0.25278463137835,1.54));
#36984=CARTESIAN_POINT('',(0.874110501322002,-0.214314795286275,0.94));
#36985=CARTESIAN_POINT('',(0.874110501322002,-0.214314795286275,1.54));
#36986=CARTESIAN_POINT('',(0.874110501322002,-0.214314795286275,0.795));
#36987=CARTESIAN_POINT('',(0.846097674634742,-0.179843612557362,0.94));
#36988=CARTESIAN_POINT('',(0.905372812789799,-0.25278463137835,0.94));
#36989=CARTESIAN_POINT('',(0.846097674634742,-0.179843612557362,1.54));
#36990=CARTESIAN_POINT('',(0.846097674634742,-0.179843612557362,1.54));
#36991=CARTESIAN_POINT('',(0.905372812789799,-0.25278463137835,1.54));
#36992=CARTESIAN_POINT('Origin',(0.888006833809975,-0.195051339113508,1.54));
#36993=CARTESIAN_POINT('',(0.885709358356629,-0.159746463245636,1.54));
#36994=CARTESIAN_POINT('Origin',(0.,0.,1.54));
#36995=CARTESIAN_POINT('',(0.846097674634742,-0.179843612557362,1.54));
#36996=CARTESIAN_POINT('Origin',(0.846097674634742,-0.179843612557362,1.54));
#36997=CARTESIAN_POINT('',(0.885709358356629,-0.159746463245636,0.94));
#36998=CARTESIAN_POINT('',(0.885709358356629,-0.159746463245636,0.795));
#36999=CARTESIAN_POINT('',(0.846097674634742,-0.179843612557362,0.94));
#37000=CARTESIAN_POINT('Origin',(0.888006833809975,-0.195051339113508,0.94));
#37001=CARTESIAN_POINT('Origin',(0.,0.,0.94));
#37002=CARTESIAN_POINT('Origin',(0.,0.,0.0794349077448279));
#37003=CARTESIAN_POINT('',(-1.045,-1.27975590510898E-16,-6.93889390390723E-17));
#37004=CARTESIAN_POINT('Origin',(0.,0.,0.));
#37005=CARTESIAN_POINT('',(-1.1,-9.25861368525747E-17,0.0317542648054295));
#37006=CARTESIAN_POINT('',(-1.18258529610859,-1.44824929759811E-16,0.0794349077448279));
#37007=CARTESIAN_POINT('',(-1.1,0.635085296108588,0.130002302030174));
#37008=CARTESIAN_POINT('Ctrl Pts',(-1.1,0.635085296108588,0.130002302030174));
#37009=CARTESIAN_POINT('Ctrl Pts',(-1.1,0.294744111674235,0.0317542648054296));
#37010=CARTESIAN_POINT('Ctrl Pts',(-1.1,-5.04611257989404E-17,0.0317542648054295));
#37011=CARTESIAN_POINT('',(7.77755175064932E-17,1.27017059221718,0.130002302030174));
#37012=CARTESIAN_POINT('Ctrl Pts',(7.77755175064932E-17,1.27017059221718,
0.130002302030174));
#37013=CARTESIAN_POINT('Ctrl Pts',(-0.55,0.952627944162882,-0.0533310313031589));
#37014=CARTESIAN_POINT('Ctrl Pts',(-1.1,0.635085296108588,0.130002302030174));
#37015=CARTESIAN_POINT('',(1.1,0.635085296108588,0.130002302030174));
#37016=CARTESIAN_POINT('Ctrl Pts',(1.1,0.635085296108588,0.130002302030174));
#37017=CARTESIAN_POINT('Ctrl Pts',(0.55,0.952627944162882,-0.0533310313031591));
#37018=CARTESIAN_POINT('Ctrl Pts',(7.77755175064932E-17,1.27017059221718,
0.130002302030174));
#37019=CARTESIAN_POINT('',(1.1,-0.635085296108589,0.130002302030174));
#37020=CARTESIAN_POINT('Ctrl Pts',(1.1,-0.635085296108589,0.130002302030174));
#37021=CARTESIAN_POINT('Ctrl Pts',(1.1,-3.33066907387547E-16,-0.0533310313031591));
#37022=CARTESIAN_POINT('Ctrl Pts',(1.1,0.635085296108588,0.130002302030174));
#37023=CARTESIAN_POINT('',(-2.3332655251948E-16,-1.27017059221718,0.130002302030174));
#37024=CARTESIAN_POINT('Ctrl Pts',(-2.3332655251948E-16,-1.27017059221718,
0.130002302030174));
#37025=CARTESIAN_POINT('Ctrl Pts',(0.55,-0.952627944162883,-0.0533310313031587));
#37026=CARTESIAN_POINT('Ctrl Pts',(1.1,-0.635085296108589,0.130002302030174));
#37027=CARTESIAN_POINT('',(-1.1,-0.635085296108588,0.130002302030174));
#37028=CARTESIAN_POINT('Ctrl Pts',(-1.1,-0.635085296108588,0.130002302030174));
#37029=CARTESIAN_POINT('Ctrl Pts',(-0.55,-0.952627944162882,-0.0533310313031589));
#37030=CARTESIAN_POINT('Ctrl Pts',(-2.3332655251948E-16,-1.27017059221718,
0.130002302030174));
#37031=CARTESIAN_POINT('Ctrl Pts',(-1.1,-5.04611257989404E-17,0.0317542648054295));
#37032=CARTESIAN_POINT('Ctrl Pts',(-1.1,-0.294744111674235,0.0317542648054295));
#37033=CARTESIAN_POINT('Ctrl Pts',(-1.1,-0.635085296108588,0.130002302030174));
#37034=CARTESIAN_POINT('Origin',(-2.3332655251948E-16,-1.27017059221718,
0.));
#37035=CARTESIAN_POINT('',(1.1,-0.635085296108589,0.669997697969826));
#37036=CARTESIAN_POINT('',(1.1,-0.635085296108589,0.));
#37037=CARTESIAN_POINT('',(-2.3332655251948E-16,-1.27017059221718,0.669997697969826));
#37038=CARTESIAN_POINT('Ctrl Pts',(1.1,-0.635085296108589,0.669997697969826));
#37039=CARTESIAN_POINT('Ctrl Pts',(0.55,-0.952627944162883,0.853331031303159));
#37040=CARTESIAN_POINT('Ctrl Pts',(-2.3332655251948E-16,-1.27017059221718,
0.669997697969826));
#37041=CARTESIAN_POINT('',(-2.3332655251948E-16,-1.27017059221718,0.));
#37042=CARTESIAN_POINT('Origin',(1.1,-0.635085296108589,0.));
#37043=CARTESIAN_POINT('',(1.1,0.635085296108588,0.669997697969826));
#37044=CARTESIAN_POINT('',(1.1,0.635085296108588,0.));
#37045=CARTESIAN_POINT('Ctrl Pts',(1.1,0.635085296108588,0.669997697969826));
#37046=CARTESIAN_POINT('Ctrl Pts',(1.1,-3.33066907387547E-16,0.853331031303159));
#37047=CARTESIAN_POINT('Ctrl Pts',(1.1,-0.635085296108589,0.669997697969826));
#37048=CARTESIAN_POINT('Origin',(1.1,0.635085296108588,0.));
#37049=CARTESIAN_POINT('',(7.77755175064932E-17,1.27017059221718,0.669997697969826));
#37050=CARTESIAN_POINT('',(7.77755175064932E-17,1.27017059221718,0.));
#37051=CARTESIAN_POINT('Ctrl Pts',(7.77755175064932E-17,1.27017059221718,
0.669997697969826));
#37052=CARTESIAN_POINT('Ctrl Pts',(0.55,0.952627944162882,0.853331031303159));
#37053=CARTESIAN_POINT('Ctrl Pts',(1.1,0.635085296108588,0.669997697969826));
#37054=CARTESIAN_POINT('Origin',(0.,0.,0.720565092255172));
#37055=CARTESIAN_POINT('',(-1.1,0.635085296108588,0.669997697969826));
#37056=CARTESIAN_POINT('Ctrl Pts',(-1.1,0.635085296108588,0.669997697969826));
#37057=CARTESIAN_POINT('Ctrl Pts',(-0.55,0.952627944162882,0.853331031303159));
#37058=CARTESIAN_POINT('Ctrl Pts',(7.77755175064932E-17,1.27017059221718,
0.669997697969826));
#37059=CARTESIAN_POINT('',(-1.1,-1.43047262651515E-16,0.768245735194571));
#37060=CARTESIAN_POINT('Ctrl Pts',(-1.1,-1.51383377396821E-16,0.768245735194571));
#37061=CARTESIAN_POINT('Ctrl Pts',(-1.1,0.294744111674235,0.768245735194571));
#37062=CARTESIAN_POINT('Ctrl Pts',(-1.1,0.635085296108588,0.669997697969826));
#37063=CARTESIAN_POINT('',(-1.045,-1.27975590510898E-16,0.8));
#37064=CARTESIAN_POINT('',(-1.18258529610859,-1.44824929759811E-16,0.720565092255172));
#37065=CARTESIAN_POINT('Origin',(0.,0.,0.8));
#37066=CARTESIAN_POINT('',(-1.1,-0.635085296108588,0.669997697969826));
#37067=CARTESIAN_POINT('Ctrl Pts',(-1.1,-0.635085296108588,0.669997697969826));
#37068=CARTESIAN_POINT('Ctrl Pts',(-1.1,-0.294744111674235,0.76824573519457));
#37069=CARTESIAN_POINT('Ctrl Pts',(-1.1,-1.51383377396821E-16,0.768245735194571));
#37070=CARTESIAN_POINT('Ctrl Pts',(-2.3332655251948E-16,-1.27017059221718,
0.669997697969826));
#37071=CARTESIAN_POINT('Ctrl Pts',(-0.55,-0.952627944162883,0.853331031303159));
#37072=CARTESIAN_POINT('Ctrl Pts',(-1.1,-0.635085296108588,0.669997697969826));
#37073=CARTESIAN_POINT('Origin',(7.77755175064932E-17,1.27017059221718,
0.));
#37074=CARTESIAN_POINT('',(-1.1,0.635085296108588,0.));
#37075=CARTESIAN_POINT('Origin',(0.,0.,0.8));
#37076=CARTESIAN_POINT('',(-0.9,-1.10218211923262E-16,0.8));
#37077=CARTESIAN_POINT('Origin',(0.,0.,0.8));
#37078=CARTESIAN_POINT('Origin',(0.,0.,0.));
#37079=CARTESIAN_POINT('',(-0.7431,9.10035036446398E-17,0.));
#37080=CARTESIAN_POINT('Origin',(0.,0.,0.));
#37081=CARTESIAN_POINT('Origin',(-1.1,-0.635085296108589,0.));
#37082=CARTESIAN_POINT('',(-1.1,-0.635085296108589,0.));
#37083=CARTESIAN_POINT('Origin',(-1.1,0.635085296108588,0.));
#37084=CARTESIAN_POINT('Origin',(0.,0.,-0.925));
#37085=CARTESIAN_POINT('',(-0.3,-3.67394039744206E-17,-1.2));
#37086=CARTESIAN_POINT('Origin',(0.,0.,-1.2));
#37087=CARTESIAN_POINT('',(-0.3,-3.67394039744206E-17,-0.6));
#37088=CARTESIAN_POINT('',(-0.3,-3.67394039744206E-17,-0.925));
#37089=CARTESIAN_POINT('Origin',(0.,0.,-0.6));
#37090=CARTESIAN_POINT('Origin',(0.,0.,-0.6));
#37091=CARTESIAN_POINT('',(0.,0.,-0.4));
#37092=CARTESIAN_POINT('',(-0.3,-3.67394039744206E-17,-0.6));
#37093=CARTESIAN_POINT('Origin',(0.7531,0.,-1.2));
#37094=CARTESIAN_POINT('',(-0.7531,-9.22281504437872E-17,-1.2));
#37095=CARTESIAN_POINT('Origin',(0.,0.,-1.2));
#37096=CARTESIAN_POINT('Origin',(0.,0.,-1.16));
#37097=CARTESIAN_POINT('',(-0.7931,-9.71267376403766E-17,-1.16));
#37098=CARTESIAN_POINT('Origin',(0.7431,0.,-0.12));
#37099=CARTESIAN_POINT('',(-0.7431,-9.10035036446398E-17,-0.12));
#37100=CARTESIAN_POINT('Origin',(0.,0.,-0.12));
#37101=CARTESIAN_POINT('Origin',(0.,0.,-0.0349999999999999));
#37102=CARTESIAN_POINT('',(-0.7431,-9.10035036446398E-17,-0.0349999999999999));
#37103=CARTESIAN_POINT('Origin',(0.,0.,0.795));
#37104=CARTESIAN_POINT('Origin',(0.,0.,1.54));
#37105=CARTESIAN_POINT('Origin',(0.,0.,1.54));
#37106=CARTESIAN_POINT('Origin',(0.,0.,1.54));
#37107=CARTESIAN_POINT('Origin',(0.,0.,1.54));
#37108=CARTESIAN_POINT('Origin',(0.,0.,1.54));
#37109=CARTESIAN_POINT('Origin',(0.,0.,1.54));
#37110=CARTESIAN_POINT('Origin',(0.,0.,1.54));
#37111=CARTESIAN_POINT('Origin',(0.,0.,1.54));
#37112=CARTESIAN_POINT('Origin',(0.,0.,1.54));
#37113=CARTESIAN_POINT('Origin',(0.,0.,1.54));
#37114=CARTESIAN_POINT('Origin',(0.,0.,1.54));
#37115=CARTESIAN_POINT('Origin',(0.,0.,1.54));
#37116=CARTESIAN_POINT('Origin',(0.,0.,1.54));
#37117=CARTESIAN_POINT('',(-0.9,-1.10218211923262E-16,0.795));
#37118=CARTESIAN_POINT('Origin',(0.,0.,1.54));
#37119=CARTESIAN_POINT('Origin',(0.,0.,1.54));
#37120=CARTESIAN_POINT('Origin',(0.,0.,1.54));
#37121=CARTESIAN_POINT('Origin',(0.,0.,1.54));
#37122=CARTESIAN_POINT('Origin',(0.,0.,1.54));
#37123=CARTESIAN_POINT('Origin',(0.,0.,1.54));
#37124=CARTESIAN_POINT('Origin',(0.,0.,1.54));
#37125=CARTESIAN_POINT('Origin',(0.,0.,1.54));
#37126=CARTESIAN_POINT('Origin',(0.,0.,1.54));
#37127=CARTESIAN_POINT('Origin',(0.,0.,1.54));
#37128=CARTESIAN_POINT('Origin',(0.,0.,1.54));
#37129=CARTESIAN_POINT('Origin',(0.,0.,1.54));
#37130=CARTESIAN_POINT('Origin',(0.,0.,1.54));
#37131=CARTESIAN_POINT('Origin',(0.,0.,1.54));
#37132=CARTESIAN_POINT('Origin',(0.,0.,1.54));
#37133=CARTESIAN_POINT('Origin',(0.,0.,1.54));
#37134=CARTESIAN_POINT('Origin',(0.,0.,1.54));
#37135=CARTESIAN_POINT('Origin',(0.,0.,1.57));
#37136=CARTESIAN_POINT('',(-0.84,-1.02870331128378E-16,1.6));
#37137=CARTESIAN_POINT('Origin',(0.,0.,1.6));
#37138=CARTESIAN_POINT('',(-0.87,-1.0654427152582E-16,1.57));
#37139=CARTESIAN_POINT('Origin',(0.,0.,1.6));
#37140=CARTESIAN_POINT('',(0.,0.,0.));
#37141=CARTESIAN_POINT('Origin',(0.,0.,-0.930039011722494));
#37142=CARTESIAN_POINT('',(-0.572251846808819,1.31896832121565E-5,-0.194775853827758));
#37143=CARTESIAN_POINT('',(-0.572209896248783,5.87811292650231E-6,-0.188250461961717));
#37144=CARTESIAN_POINT('',(-0.57225,6.55557234450825E-15,-0.930039011722494));
#37145=CARTESIAN_POINT('',(0.532887356432457,0.208459172818158,-0.12));
#37146=CARTESIAN_POINT('Ctrl Pts',(-0.572251846808819,1.31896832121572E-5,
-0.194775853827758));
#37147=CARTESIAN_POINT('Ctrl Pts',(-0.572182461406416,-0.0721591436399304,
-0.192092383539388));
#37148=CARTESIAN_POINT('Ctrl Pts',(-0.540797694659007,-0.237406800584547,
-0.185950422500778));
#37149=CARTESIAN_POINT('Ctrl Pts',(-0.385757245550577,-0.453572246869937,
-0.176349970711929));
#37150=CARTESIAN_POINT('Ctrl Pts',(-0.128270146612636,-0.581450425290948,
-0.165974498461211));
#37151=CARTESIAN_POINT('Ctrl Pts',(0.159119430707533,-0.573773118428659,
-0.155599026210492));
#37152=CARTESIAN_POINT('Ctrl Pts',(0.409415432322886,-0.432341853180699,
-0.145223553959774));
#37153=CARTESIAN_POINT('Ctrl Pts',(0.56426305151595,-0.190104706888137,
-0.134848081709056));
#37154=CARTESIAN_POINT('Ctrl Pts',(0.583151179466301,0.0420829677627029,
-0.126440230389131));
#37155=CARTESIAN_POINT('Ctrl Pts',(0.54751143363328,0.171111722668445,-0.121490869819446));
#37156=CARTESIAN_POINT('Ctrl Pts',(0.532887356432457,0.208459172818158,
-0.12));
#37157=CARTESIAN_POINT('',(0.570996795169322,0.0378513197440182,-0.12));
#37158=CARTESIAN_POINT('Origin',(0.,0.,-0.12));
#37159=CARTESIAN_POINT('Ctrl Pts',(-0.572209896248783,5.87811292651272E-6,
-0.188250461961717));
#37160=CARTESIAN_POINT('Ctrl Pts',(-0.572189385338301,-0.0537745726271744,
-0.186251252475915));
#37161=CARTESIAN_POINT('Ctrl Pts',(-0.551638057130558,-0.200606777068497,
-0.180793552239873));
#37162=CARTESIAN_POINT('Ctrl Pts',(-0.427655041590171,-0.414301519355521,
-0.171877361253592));
#37163=CARTESIAN_POINT('Ctrl Pts',(-0.183688600698895,-0.566391183638125,
-0.161501889002873));
#37164=CARTESIAN_POINT('Ctrl Pts',(0.103112831945545,-0.586430161623632,
-0.151126416752155));
#37165=CARTESIAN_POINT('Ctrl Pts',(0.365851355459577,-0.469776284513869,
-0.140750944501437));
#37166=CARTESIAN_POINT('Ctrl Pts',(0.543351022386391,-0.243565284402786,
-0.130375472250718));
#37167=CARTESIAN_POINT('Ctrl Pts',(0.577149518655877,-0.0549640805153465,
-0.123458490750239));
#37168=CARTESIAN_POINT('Ctrl Pts',(0.570996795169322,0.0378513197440182,
-0.12));
#37169=CARTESIAN_POINT('Origin',(0.,0.,-0.930039011722494));
#37170=CARTESIAN_POINT('',(-0.572223068770992,1.08892936001897E-5,-0.328460064354073));
#37171=CARTESIAN_POINT('',(-0.572206446074254,-2.92925376449427E-6,-0.321934672488033));
#37172=CARTESIAN_POINT('',(-0.57225,6.55557234450825E-15,-0.930039011722494));
#37173=CARTESIAN_POINT('Ctrl Pts',(-0.572223068770992,1.08892936001997E-5,
-0.328460064354073));
#37174=CARTESIAN_POINT('Ctrl Pts',(-0.572178592440248,-0.0614397738734596,
-0.326175570310044));
#37175=CARTESIAN_POINT('Ctrl Pts',(-0.547362804764057,-0.215955547533754,
-0.320432585515775));
#37176=CARTESIAN_POINT('Ctrl Pts',(-0.410649598305695,-0.431165515585077,
-0.311231109971268));
#37177=CARTESIAN_POINT('Ctrl Pts',(-0.160760107350392,-0.57331752294948,
-0.300855637720549));
#37178=CARTESIAN_POINT('Ctrl Pts',(0.126606838000238,-0.581813976495778,
-0.290480165469831));
#37179=CARTESIAN_POINT('Ctrl Pts',(0.3844583637991,-0.454674125457656,-0.280104693219112));
#37180=CARTESIAN_POINT('Ctrl Pts',(0.552682425815823,-0.221537651868143,
-0.269729220968394));
#37181=CARTESIAN_POINT('Ctrl Pts',(0.592061522393167,0.0632451413900827,
-0.259353748717676));
#37182=CARTESIAN_POINT('Ctrl Pts',(0.493415341577429,0.333283802752439,
-0.248978276466957));
#37183=CARTESIAN_POINT('Ctrl Pts',(0.279740925892577,0.525625166857998,
-0.238602804216239));
#37184=CARTESIAN_POINT('Ctrl Pts',(0.000851470205678055,0.595429299999864,
-0.228227331965521));
#37185=CARTESIAN_POINT('Ctrl Pts',(-0.278236497349112,0.526423100377946,
-0.217851859714802));
#37186=CARTESIAN_POINT('Ctrl Pts',(-0.492460118502939,0.334693554718123,
-0.207476387464084));
#37187=CARTESIAN_POINT('Ctrl Pts',(-0.56616513883061,0.134706710058056,
-0.199784385501736));
#37188=CARTESIAN_POINT('Ctrl Pts',(-0.57227188619843,0.020857480506449,
-0.195550874289627));
#37189=CARTESIAN_POINT('Ctrl Pts',(-0.572251846808819,1.31896832121572E-5,
-0.194775853827758));
#37190=CARTESIAN_POINT('Ctrl Pts',(-0.572206446074254,-2.92925376450121E-6,
-0.321934672488033));
#37191=CARTESIAN_POINT('Ctrl Pts',(-0.572214485737319,-0.0430512316554342,
-0.320334439246571));
#37192=CARTESIAN_POINT('Ctrl Pts',(-0.557042913275609,-0.179131739323211,
-0.31527571525487));
#37193=CARTESIAN_POINT('Ctrl Pts',(-0.450274644860222,-0.389601769278859,
-0.30675850051293));
#37194=CARTESIAN_POINT('Ctrl Pts',(-0.215241042075345,-0.555164919115264,
-0.296383028262211));
#37195=CARTESIAN_POINT('Ctrl Pts',(0.0699709674208999,-0.591304370416951,
-0.286007556011493));
#37196=CARTESIAN_POINT('Ctrl Pts',(0.338870887774159,-0.489595052448449,
-0.275632083760774));
#37197=CARTESIAN_POINT('Ctrl Pts',(0.528770989858389,-0.273748118747132,
-0.265256611510057));
#37198=CARTESIAN_POINT('Ctrl Pts',(0.595400531599021,0.00591678855841044,
-0.254881139259338));
#37199=CARTESIAN_POINT('Ctrl Pts',(0.523226356835316,0.284202314475096,
-0.24450566700862));
#37200=CARTESIAN_POINT('Ctrl Pts',(0.329074261287382,0.496232767362635,
-0.234130194757902));
#37201=CARTESIAN_POINT('Ctrl Pts',(0.0582061064454895,0.592578090033583,
-0.223754722507183));
#37202=CARTESIAN_POINT('Ctrl Pts',(-0.226231237425986,0.550777869717469,
-0.213379250256465));
#37203=CARTESIAN_POINT('Ctrl Pts',(-0.457928466129024,0.380576366952199,
-0.203003778005746));
#37204=CARTESIAN_POINT('Ctrl Pts',(-0.558795180707474,0.171543964843103,
-0.194627515240831));
#37205=CARTESIAN_POINT('Ctrl Pts',(-0.57222486776007,0.0392617963722867,
-0.189709743226154));
#37206=CARTESIAN_POINT('Ctrl Pts',(-0.572209896248783,5.87811292651272E-6,
-0.188250461961717));
#37207=CARTESIAN_POINT('Origin',(0.,0.,-0.930039011722494));
#37208=CARTESIAN_POINT('',(-0.57220691239729,3.53495086150753E-6,-0.462144274880389));
#37209=CARTESIAN_POINT('',(-0.572221465652637,-1.05155042379457E-5,-0.455618883014349));
#37210=CARTESIAN_POINT('',(-0.57225,6.55557234450825E-15,-0.930039011722494));
#37211=CARTESIAN_POINT('Ctrl Pts',(-0.57220691239729,3.53495086147584E-6,
-0.462144274880389));
#37212=CARTESIAN_POINT('Ctrl Pts',(-0.572195468328224,-0.0507191652367547,
-0.460258757080701));
#37213=CARTESIAN_POINT('Ctrl Pts',(-0.553245437112089,-0.194487822942528,
-0.454914748530773));
#37214=CARTESIAN_POINT('Ctrl Pts',(-0.434242783628202,-0.407394157101084,
-0.446112249230605));
#37215=CARTESIAN_POINT('Ctrl Pts',(-0.192741275441066,-0.563371631442748,
-0.435736776979888));
#37216=CARTESIAN_POINT('Ctrl Pts',(0.0936933474406337,-0.588012203120214,
-0.425361304729168));
#37217=CARTESIAN_POINT('Ctrl Pts',(0.35828556050624,-0.475571499888217,
-0.414985832478451));
#37218=CARTESIAN_POINT('Ctrl Pts',(0.539351885579122,-0.252262438534088,
-0.404610360227732));
#37219=CARTESIAN_POINT('Ctrl Pts',(0.594680949235049,0.0298557028055502,
-0.394234887977014));
#37220=CARTESIAN_POINT('Ctrl Pts',(0.511374075994885,0.30501368620711,-0.383859415726295));
#37221=CARTESIAN_POINT('Ctrl Pts',(0.308852312449722,0.509064871569989,
-0.373483943475578));
#37222=CARTESIAN_POINT('Ctrl Pts',(0.0343288650529642,0.594439503565886,
-0.363108471224859));
#37223=CARTESIAN_POINT('Ctrl Pts',(-0.248197553305573,0.5412344860607,-0.352732998974141));
#37224=CARTESIAN_POINT('Ctrl Pts',(-0.472862524479398,0.361853322940755,
-0.342357526723422));
#37225=CARTESIAN_POINT('Ctrl Pts',(-0.562095633396269,0.156185112186377,
-0.334266548516733));
#37226=CARTESIAN_POINT('Ctrl Pts',(-0.572245925064243,0.0315902564366742,
-0.329634061060284));
#37227=CARTESIAN_POINT('Ctrl Pts',(-0.572223068770992,1.08892936001997E-5,
-0.328460064354073));
#37228=CARTESIAN_POINT('Ctrl Pts',(-0.572221465652637,-1.051550423797E-5,
-0.455618883014349));
#37229=CARTESIAN_POINT('Ctrl Pts',(-0.572243953210631,-0.0323234178361406,
-0.454417626017228));
#37230=CARTESIAN_POINT('Ctrl Pts',(-0.561794458224291,-0.157652709186653,
-0.449757878269868));
#37231=CARTESIAN_POINT('Ctrl Pts',(-0.471468172615134,-0.363668195390408,
-0.441639639772268));
#37232=CARTESIAN_POINT('Ctrl Pts',(-0.24611537226857,-0.542184486739477,
-0.431264167521549));
#37233=CARTESIAN_POINT('Ctrl Pts',(0.0366134635183988,-0.594303162045059,
-0.420888695270832));
#37234=CARTESIAN_POINT('Ctrl Pts',(0.310806727710773,-0.507873972691536,
-0.410513223020113));
#37235=CARTESIAN_POINT('Ctrl Pts',(0.51254268190422,-0.30304586015049,-0.400137750769395));
#37236=CARTESIAN_POINT('Ctrl Pts',(0.594791312689474,-0.0275697021364228,
-0.389762278518676));
#37237=CARTESIAN_POINT('Ctrl Pts',(0.53837827792754,0.254333686297961,-0.379386806267958));
#37238=CARTESIAN_POINT('Ctrl Pts',(0.356454955565181,0.476945131829576,
-0.36901133401724));
#37239=CARTESIAN_POINT('Ctrl Pts',(0.0914325078965691,0.588367989131544,
-0.358635861766521));
#37240=CARTESIAN_POINT('Ctrl Pts',(-0.1949052878214,0.562626628325057,-0.348260389515803));
#37241=CARTESIAN_POINT('Ctrl Pts',(-0.435805479980445,0.405722044928676,
-0.337884917265085));
#37242=CARTESIAN_POINT('Ctrl Pts',(-0.553622904582432,0.19302062926978,
-0.329109678255828));
#37243=CARTESIAN_POINT('Ctrl Pts',(-0.572197110082555,0.0499865529700694,
-0.323792929996811));
#37244=CARTESIAN_POINT('Ctrl Pts',(-0.572206446074254,-2.92925376450121E-6,
-0.321934672488033));
#37245=CARTESIAN_POINT('Origin',(0.,0.,-0.930039011722494));
#37246=CARTESIAN_POINT('',(-0.572208961924848,-5.40006758461863E-6,-0.595828485406705));
#37247=CARTESIAN_POINT('',(-0.572249685678755,-1.32408837813236E-5,-0.589303093540665));
#37248=CARTESIAN_POINT('',(-0.57225,6.55557234450825E-15,-0.930039011722494));
#37249=CARTESIAN_POINT('Ctrl Pts',(-0.572208961924848,-5.40006758461067E-6,
-0.595828485406705));
#37250=CARTESIAN_POINT('Ctrl Pts',(-0.572222810317603,-0.0399947468816952,
-0.594341943851358));
#37251=CARTESIAN_POINT('Ctrl Pts',(-0.558462838001496,-0.173011307588341,
-0.589396911545771));
#37252=CARTESIAN_POINT('Ctrl Pts',(-0.4564620684611,-0.382333849583464,
-0.580993388489942));
#37253=CARTESIAN_POINT('Ctrl Pts',(-0.224112632886457,-0.551643292344488,
-0.570617916239226));
#37254=CARTESIAN_POINT('Ctrl Pts',(0.0604834222543564,-0.592350023747205,
-0.560242443988507));
#37255=CARTESIAN_POINT('Ctrl Pts',(0.330979180111506,-0.494964217078851,
-0.549866971737789));
#37256=CARTESIAN_POINT('Ctrl Pts',(0.524314895013938,-0.282189095361197,
-0.539491499487071));
#37257=CARTESIAN_POINT('Ctrl Pts',(0.595418869741894,-0.00362819397533901,
-0.529116027236352));
#37258=CARTESIAN_POINT('Ctrl Pts',(0.527714879176066,0.27577853563061,-0.518740554985634));
#37259=CARTESIAN_POINT('Ctrl Pts',(0.336986522471297,0.490893958039981,
-0.508365082734915));
#37260=CARTESIAN_POINT('Ctrl Pts',(0.0676976498285046,0.591568949974742,
-0.497989610484197));
#37261=CARTESIAN_POINT('Ctrl Pts',(-0.217373344570204,0.554333494794116,
-0.487614138233479));
#37262=CARTESIAN_POINT('Ctrl Pts',(-0.451768834165619,0.387868166836234,
-0.47723866598276));
#37263=CARTESIAN_POINT('Ctrl Pts',(-0.557388196836304,0.177664246876017,
-0.468748711531731));
#37264=CARTESIAN_POINT('Ctrl Pts',(-0.572216459488857,0.0423184021916877,
-0.46371724783094));
#37265=CARTESIAN_POINT('Ctrl Pts',(-0.57220691239729,3.53495086147584E-6,
-0.462144274880389));
#37266=CARTESIAN_POINT('Ctrl Pts',(-0.572249685678755,-1.32408837812507E-5,
-0.589303093540665));
#37267=CARTESIAN_POINT('Ctrl Pts',(-0.572270338122677,-0.0215909230762567,
-0.588500812787885));
#37268=CARTESIAN_POINT('Ctrl Pts',(-0.565907101669391,-0.136174074584614,
-0.584240041284865));
#37269=CARTESIAN_POINT('Ctrl Pts',(-0.491170026481974,-0.336584016022301,
-0.576520779031606));
#37270=CARTESIAN_POINT('Ctrl Pts',(-0.276211019809465,-0.527488640774144,
-0.566145306780888));
#37271=CARTESIAN_POINT('Ctrl Pts',(0.0031401178304551,-0.595421643954287,
-0.555769834530169));
#37272=CARTESIAN_POINT('Ctrl Pts',(0.281759210488034,-0.524546033533648,
-0.545394362279452));
#37273=CARTESIAN_POINT('Ctrl Pts',(0.494692741566129,-0.331384799915253,
-0.535018890028733));
#37274=CARTESIAN_POINT('Ctrl Pts',(0.59230024480053,-0.0609689603923613,
-0.524643417778015));
#37275=CARTESIAN_POINT('Ctrl Pts',(0.551826816631903,0.223660364318458,
-0.514267945527296));
#37276=CARTESIAN_POINT('Ctrl Pts',(0.382707889009843,0.456148512904055,
-0.503892473276577));
#37277=CARTESIAN_POINT('Ctrl Pts',(0.124369579435742,0.582296317894835,
-0.49351700102586));
#37278=CARTESIAN_POINT('Ctrl Pts',(-0.162962585060135,0.572695372777406,
-0.483141528775141));
#37279=CARTESIAN_POINT('Ctrl Pts',(-0.412303839155969,0.429583913041453,
-0.472766056524423));
#37280=CARTESIAN_POINT('Ctrl Pts',(-0.547786258426805,0.214489182365462,
-0.463591841270825));
#37281=CARTESIAN_POINT('Ctrl Pts',(-0.57217921018603,0.060707360836633,
-0.457876116767467));
#37282=CARTESIAN_POINT('Ctrl Pts',(-0.572221465652637,-1.051550423797E-5,
-0.455618883014349));
#37283=CARTESIAN_POINT('Origin',(0.,0.,-0.930039011722494));
#37284=CARTESIAN_POINT('',(-0.57225,6.55557234450825E-15,-0.72625));
#37285=CARTESIAN_POINT('',(-0.572279863946809,-1.0961849272878E-5,-0.722987304066981));
#37286=CARTESIAN_POINT('',(-0.57225,6.55557234450825E-15,-0.930039011722494));
#37287=CARTESIAN_POINT('',(-0.565534825602702,-0.0874095162469292,-0.72625));
#37288=CARTESIAN_POINT('Origin',(0.,0.,-0.72625));
#37289=CARTESIAN_POINT('Ctrl Pts',(-0.565534825602701,-0.0874095162469292,
-0.72625));
#37290=CARTESIAN_POINT('Ctrl Pts',(-0.551326428453064,-0.179337074585254,
-0.722791509249761));
#37291=CARTESIAN_POINT('Ctrl Pts',(-0.477265386956567,-0.356050729042777,
-0.715874527749281));
#37292=CARTESIAN_POINT('Ctrl Pts',(-0.254761663575757,-0.538176058210883,
-0.705499055498564));
#37293=CARTESIAN_POINT('Ctrl Pts',(0.0270755327719408,-0.594810479406871,
-0.695123583247846));
#37294=CARTESIAN_POINT('Ctrl Pts',(0.302628938713621,-0.512792550344605,
-0.684748110997126));
#37295=CARTESIAN_POINT('Ctrl Pts',(0.507617355421152,-0.311222115434097,
-0.674372638746409));
#37296=CARTESIAN_POINT('Ctrl Pts',(0.594273793373837,-0.0371010254861046,
-0.66399716649569));
#37297=CARTESIAN_POINT('Ctrl Pts',(0.542385624529068,0.245671060423536,
-0.653621694244972));
#37298=CARTESIAN_POINT('Ctrl Pts',(0.364054758182736,0.471169804196079,
-0.643246221994254));
#37299=CARTESIAN_POINT('Ctrl Pts',(0.100852138510465,0.586826789571409,
-0.632870749743535));
#37300=CARTESIAN_POINT('Ctrl Pts',(-0.185861335713837,0.565678625875551,
-0.622495277492817));
#37301=CARTESIAN_POINT('Ctrl Pts',(-0.429245823844828,0.412655851503898,
-0.612119805242099));
#37302=CARTESIAN_POINT('Ctrl Pts',(-0.552028076495681,0.199139421463527,
-0.603230874546727));
#37303=CARTESIAN_POINT('Ctrl Pts',(-0.572190591549094,0.0530418625337585,
-0.597800434601597));
#37304=CARTESIAN_POINT('Ctrl Pts',(-0.572208961924848,-5.40006758461067E-6,
-0.595828485406705));
#37305=CARTESIAN_POINT('Ctrl Pts',(-0.57227986394681,-1.09618492728416E-5,
-0.722987304066981));
#37306=CARTESIAN_POINT('Ctrl Pts',(-0.572288362754473,-0.010857064175054,
-0.722583999558541));
#37307=CARTESIAN_POINT('Ctrl Pts',(-0.569393706449464,-0.114707216006389,
-0.718722204299863));
#37308=CARTESIAN_POINT('Ctrl Pts',(-0.509318192700196,-0.308427575223672,
-0.711401918290944));
#37309=CARTESIAN_POINT('Ctrl Pts',(-0.305432606070274,-0.511127575150115,
-0.701026446040226));
#37310=CARTESIAN_POINT('Ctrl Pts',(-0.0303432431553614,-0.594654413195259,
-0.690650973789507));
#37311=CARTESIAN_POINT('Ctrl Pts',(0.251820278225985,-0.539559427088026,
-0.680275501538789));
#37312=CARTESIAN_POINT('Ctrl Pts',(0.47527762677182,-0.358674800641695,
-0.669900029288071));
#37313=CARTESIAN_POINT('Ctrl Pts',(0.587935213613219,-0.0941755582271385,
-0.659524557037353));
#37314=CARTESIAN_POINT('Ctrl Pts',(0.563529430095987,0.192279525622204,
-0.649149084786634));
#37315=CARTESIAN_POINT('Ctrl Pts',(0.407749978910367,0.433908628992312,
-0.638773612535916));
#37316=CARTESIAN_POINT('Ctrl Pts',(0.156913157834808,0.574382355007991,
-0.628398140285198));
#37317=CARTESIAN_POINT('Ctrl Pts',(-0.130504285744414,0.580952155897969,
-0.618022668034479));
#37318=CARTESIAN_POINT('Ctrl Pts',(-0.387497714117257,0.452086632150457,
-0.607647195783761));
#37319=CARTESIAN_POINT('Ctrl Pts',(-0.541268381761995,0.235941679265191,
-0.598074004285823));
#37320=CARTESIAN_POINT('Ctrl Pts',(-0.572181309081377,0.0714266571357631,
-0.591959303538124));
#37321=CARTESIAN_POINT('Ctrl Pts',(-0.572249685678755,-1.32408837812507E-5,
-0.589303093540665));
#37322=CARTESIAN_POINT('Origin',(0.,0.,0.895));
#37323=CARTESIAN_POINT('',(-0.692512978718214,1.7491275774939E-5,0.74826868253652));
#37324=CARTESIAN_POINT('',(-0.692497106487793,1.22237887413546E-5,0.72673131746348));
#37325=CARTESIAN_POINT('',(-0.6925,-8.48067908409542E-17,0.895));
#37326=CARTESIAN_POINT('',(0.301885354887797,0.623234692956248,0.7));
#37327=CARTESIAN_POINT('Ctrl Pts',(-0.692512978718214,1.7491275774939E-5,
0.74826868253652));
#37328=CARTESIAN_POINT('Ctrl Pts',(-0.692536236153761,0.0225620266177927,
0.747491425144957));
#37329=CARTESIAN_POINT('Ctrl Pts',(-0.691457063407575,0.0451043386912214,
0.746714167753393));
#37330=CARTESIAN_POINT('Ctrl Pts',(-0.68925900073676,0.0675370076365317,
0.74593691036183));
#37331=CARTESIAN_POINT('Ctrl Pts',(-0.678019345746454,0.182245047040874,
0.741962453656916));
#37332=CARTESIAN_POINT('Ctrl Pts',(-0.637523809648264,0.294086221483862,
0.737987996952002));
#37333=CARTESIAN_POINT('Ctrl Pts',(-0.572718974199324,0.389399622791066,
0.734013540247089));
#37334=CARTESIAN_POINT('Ctrl Pts',(-0.507914138750383,0.484713024098269,
0.730039083542176));
#37335=CARTESIAN_POINT('Ctrl Pts',(-0.418800003950691,0.563498652269687,
0.726064626837263));
#37336=CARTESIAN_POINT('Ctrl Pts',(-0.316262007750742,0.616131421297654,
0.72209017013235));
#37337=CARTESIAN_POINT('Ctrl Pts',(-0.213724011550792,0.668764190325621,
0.718115713427437));
#37338=CARTESIAN_POINT('Ctrl Pts',(-0.0977621539505856,0.695244100210136,
0.714141256722523));
#37339=CARTESIAN_POINT('Ctrl Pts',(0.0174586834402198,0.692339189277836,
0.710166800017609));
#37340=CARTESIAN_POINT('Ctrl Pts',(0.115705001414163,0.689862234504694,
0.706777866678406));
#37341=CARTESIAN_POINT('Ctrl Pts',(0.213412552912613,0.666020739137871,
0.703388933339203));
#37342=CARTESIAN_POINT('Ctrl Pts',(0.301912013981581,0.623256720988311,
0.7));
#37343=CARTESIAN_POINT('',(-0.3018853548878,0.623234692956246,0.7));
#37344=CARTESIAN_POINT('Origin',(0.,0.,0.7));
#37345=CARTESIAN_POINT('Ctrl Pts',(-0.301885354887799,0.623234692956247,
0.7));
#37346=CARTESIAN_POINT('Ctrl Pts',(-0.405642496870894,0.572976320013088,
0.703974456704914));
#37347=CARTESIAN_POINT('Ctrl Pts',(-0.496552660568787,0.496329702965772,
0.707948913409827));
#37348=CARTESIAN_POINT('Ctrl Pts',(-0.563546539109462,0.402559533859148,
0.71192337011474));
#37349=CARTESIAN_POINT('Ctrl Pts',(-0.630540417650137,0.308789364752525,
0.715897826819654));
#37350=CARTESIAN_POINT('Ctrl Pts',(-0.673618011033594,0.197895643586594,
0.719872283524567));
#37351=CARTESIAN_POINT('Ctrl Pts',(-0.687511393683796,0.0834733607376968,
0.72384674022948));
#37352=CARTESIAN_POINT('Ctrl Pts',(-0.690872568830618,0.055791597193332,
0.724808265974147));
#37353=CARTESIAN_POINT('Ctrl Pts',(-0.692525640229921,0.0279033127500774,
0.725769791718813));
#37354=CARTESIAN_POINT('Ctrl Pts',(-0.692497106487793,1.22237887413546E-5,
0.72673131746348));
#37355=CARTESIAN_POINT('Origin',(0.,0.,0.895));
#37356=CARTESIAN_POINT('',(-0.692502505300729,-1.80142461571609E-5,0.89826868253652));
#37357=CARTESIAN_POINT('',(-0.692519446907948,-1.67109334056352E-5,0.87673131746348));
#37358=CARTESIAN_POINT('',(-0.6925,-8.48067908409542E-17,0.895));
#37359=CARTESIAN_POINT('Ctrl Pts',(-0.692502505300729,-1.80142461571609E-5,
0.89826868253652));
#37360=CARTESIAN_POINT('Ctrl Pts',(-0.692409964808609,0.0894315645319258,
0.895184905603917));
#37361=CARTESIAN_POINT('Ctrl Pts',(-0.675000463397104,0.178916114041078,
0.892101128671314));
#37362=CARTESIAN_POINT('Ctrl Pts',(-0.641206247017397,0.261713119701919,
0.889017351738711));
#37363=CARTESIAN_POINT('Ctrl Pts',(-0.597651329520742,0.368424182624908,
0.885042895033797));
#37364=CARTESIAN_POINT('Ctrl Pts',(-0.526880147296139,0.46402672372688,
0.881068438328884));
#37365=CARTESIAN_POINT('Ctrl Pts',(-0.43753750447404,0.536842751989744,
0.877093981623971));
#37366=CARTESIAN_POINT('Ctrl Pts',(-0.348194861651941,0.609658780252608,
0.873119524919057));
#37367=CARTESIAN_POINT('Ctrl Pts',(-0.240280758232347,0.659688295676364,
0.869145068214144));
#37368=CARTESIAN_POINT('Ctrl Pts',(-0.126977060875423,0.680820118935961,
0.865170611509231));
#37369=CARTESIAN_POINT('Ctrl Pts',(-0.0136733635184988,0.701951942195558,
0.861196154804318));
#37370=CARTESIAN_POINT('Ctrl Pts',(0.105019927775755,0.694186073290997,
0.857221698099404));
#37371=CARTESIAN_POINT('Ctrl Pts',(0.214604252685671,0.658471125218892,
0.853247241394491));
#37372=CARTESIAN_POINT('Ctrl Pts',(0.324188577595589,0.622756177146787,
0.849272784689577));
#37373=CARTESIAN_POINT('Ctrl Pts',(0.424663936121169,0.55909214990714,0.845298327984664));
#37374=CARTESIAN_POINT('Ctrl Pts',(0.503757115234358,0.475255696844551,
0.841323871279751));
#37375=CARTESIAN_POINT('Ctrl Pts',(0.582850294347546,0.391419243781962,
0.837349414574837));
#37376=CARTESIAN_POINT('Ctrl Pts',(0.640561294048343,0.287410364896433,
0.833374957869924));
#37377=CARTESIAN_POINT('Ctrl Pts',(0.669840630764095,0.175933900582539,
0.82940050116501));
#37378=CARTESIAN_POINT('Ctrl Pts',(0.699119967479848,0.0644574362686454,
0.825426044460097));
#37379=CARTESIAN_POINT('Ctrl Pts',(0.699967641210555,-0.0544866134736121,
0.821451587755184));
#37380=CARTESIAN_POINT('Ctrl Pts',(0.67228010730006,-0.1663690631073,0.81747713105027));
#37381=CARTESIAN_POINT('Ctrl Pts',(0.644592573389564,-0.278251512740987,
0.813502674345357));
#37382=CARTESIAN_POINT('Ctrl Pts',(0.588369831837864,-0.383072362266105,
0.809528217640443));
#37383=CARTESIAN_POINT('Ctrl Pts',(0.5104795734465,-0.468027579985086,0.80555376093553));
#37384=CARTESIAN_POINT('Ctrl Pts',(0.432589315055136,-0.552982797704068,
0.801579304230617));
#37385=CARTESIAN_POINT('Ctrl Pts',(0.333031539824107,-0.618072383616913,
0.797604847525703));
#37386=CARTESIAN_POINT('Ctrl Pts',(0.223967376371222,-0.65534556996308,
0.79363039082079));
#37387=CARTESIAN_POINT('Ctrl Pts',(0.114903212918336,-0.692618756309248,
0.789655934115876));
#37388=CARTESIAN_POINT('Ctrl Pts',(-0.00366733875640471,-0.702075543088738,
0.785681477410963));
#37389=CARTESIAN_POINT('Ctrl Pts',(-0.117260710663312,-0.682560728047434,
0.78170702070605));
#37390=CARTESIAN_POINT('Ctrl Pts',(-0.23085408257022,-0.66304591300613,
0.777732564001136));
#37391=CARTESIAN_POINT('Ctrl Pts',(-0.339470274709293,-0.614559496144031,
0.773758107296224));
#37392=CARTESIAN_POINT('Ctrl Pts',(-0.429841660219421,-0.54302424791586,
0.76978365059131));
#37393=CARTESIAN_POINT('Ctrl Pts',(-0.52021304572955,-0.471488999687688,
0.765809193886397));
#37394=CARTESIAN_POINT('Ctrl Pts',(-0.592339624610732,-0.376904920093444,
0.761834737181483));
#37395=CARTESIAN_POINT('Ctrl Pts',(-0.637411027110111,-0.270825428113474,
0.757860280476569));
#37396=CARTESIAN_POINT('Ctrl Pts',(-0.673668122814433,-0.185491178906639,
0.754663081163219));
#37397=CARTESIAN_POINT('Ctrl Pts',(-0.6924173107223,-0.0927180345585824,
0.75146588184987));
#37398=CARTESIAN_POINT('Ctrl Pts',(-0.692512978718214,1.7491275774939E-5,
0.74826868253652));
#37399=CARTESIAN_POINT('Ctrl Pts',(-0.692497106487793,1.22237887413546E-5,
0.72673131746348));
#37400=CARTESIAN_POINT('Ctrl Pts',(-0.692407696302423,-0.0873842145414211,
0.729744248423727));
#37401=CARTESIAN_POINT('Ctrl Pts',(-0.675807013310445,-0.17480818975405,
0.732757179383974));
#37402=CARTESIAN_POINT('Ctrl Pts',(-0.643510339446282,-0.255991965181027,
0.735770110344221));
#37403=CARTESIAN_POINT('Ctrl Pts',(-0.600906730641617,-0.36308416371899,
0.739744567049134));
#37404=CARTESIAN_POINT('Ctrl Pts',(-0.530990341115338,-0.459317716263051,
0.743719023754047));
#37405=CARTESIAN_POINT('Ctrl Pts',(-0.44229971099925,-0.532927429012877,
0.74769348045896));
#37406=CARTESIAN_POINT('Ctrl Pts',(-0.353609080883162,-0.606537141762702,
0.751667937163873));
#37407=CARTESIAN_POINT('Ctrl Pts',(-0.246144210177266,-0.657523014718292,
0.755642393868788));
#37408=CARTESIAN_POINT('Ctrl Pts',(-0.133033022371476,-0.679662110949492,
0.759616850573701));
#37409=CARTESIAN_POINT('Ctrl Pts',(-0.0199218345656862,-0.701801207180692,
0.763591307278615));
#37410=CARTESIAN_POINT('Ctrl Pts',(0.0988356703399968,-0.695093526687502,
0.767565763983527));
#37411=CARTESIAN_POINT('Ctrl Pts',(0.208733556028134,-0.660355882111,0.771540220688441));
#37412=CARTESIAN_POINT('Ctrl Pts',(0.318631441716272,-0.625618237534498,
0.775514677393354));
#37413=CARTESIAN_POINT('Ctrl Pts',(0.419669708186863,-0.562850628874684,
0.779489134098267));
#37414=CARTESIAN_POINT('Ctrl Pts',(0.499506147484576,-0.479721487442206,
0.783463590803181));
#37415=CARTESIAN_POINT('Ctrl Pts',(0.579342586782288,-0.396592346009729,
0.787438047508095));
#37416=CARTESIAN_POINT('Ctrl Pts',(0.637977198907121,-0.293101671804589,
0.791412504213008));
#37417=CARTESIAN_POINT('Ctrl Pts',(0.668247797592216,-0.181890362651708,
0.795386960917921));
#37418=CARTESIAN_POINT('Ctrl Pts',(0.698518396277312,-0.0706790534988262,
0.799361417622835));
#37419=CARTESIAN_POINT('Ctrl Pts',(0.700424981522668,0.048252890601796,
0.803335874327748));
#37420=CARTESIAN_POINT('Ctrl Pts',(0.673734601904745,0.160377435949487,
0.807310331032661));
#37421=CARTESIAN_POINT('Ctrl Pts',(0.647044222286821,0.272501981297179,
0.811284787737575));
#37422=CARTESIAN_POINT('Ctrl Pts',(0.591756877805617,0.377819127891939,
0.815259244442488));
#37423=CARTESIAN_POINT('Ctrl Pts',(0.514626028750265,0.463464392651226,
0.819233701147402));
#37424=CARTESIAN_POINT('Ctrl Pts',(0.437495179694913,0.549109657410513,
0.823208157852315));
#37425=CARTESIAN_POINT('Ctrl Pts',(0.338520826065412,0.615083040334327,
0.827182614557228));
#37426=CARTESIAN_POINT('Ctrl Pts',(0.22979281598256,0.653325714460818,0.831157071262141));
#37427=CARTESIAN_POINT('Ctrl Pts',(0.121064805899708,0.691568388587309,
0.835131527967055));
#37428=CARTESIAN_POINT('Ctrl Pts',(0.00258313936350399,0.702080353916477,
0.839105984671969));
#37429=CARTESIAN_POINT('Ctrl Pts',(-0.111179466074118,0.683577599114679,
0.843080441376882));
#37430=CARTESIAN_POINT('Ctrl Pts',(-0.22494207151174,0.665074844312881,
0.847054898081795));
#37431=CARTESIAN_POINT('Ctrl Pts',(-0.33398561585078,0.617557369380116,
0.851029354786708));
#37432=CARTESIAN_POINT('Ctrl Pts',(-0.424990273328466,0.546829483415133,
0.855003811491622));
#37433=CARTESIAN_POINT('Ctrl Pts',(-0.515994930806152,0.476101597450151,
0.858978268196535));
#37434=CARTESIAN_POINT('Ctrl Pts',(-0.588960701422483,0.382163300452951,
0.862952724901448));
#37435=CARTESIAN_POINT('Ctrl Pts',(-0.634974706950498,0.276489304008043,
0.866927181606362));
#37436=CARTESIAN_POINT('Ctrl Pts',(-0.67281028172387,0.189597577278057,
0.870195226892068));
#37437=CARTESIAN_POINT('Ctrl Pts',(-0.692423363006564,0.0947711677510941,
0.873463272177774));
#37438=CARTESIAN_POINT('Ctrl Pts',(-0.692519446907948,-1.67109334056352E-5,
0.87673131746348));
#37439=CARTESIAN_POINT('Origin',(0.,0.,0.895));
#37440=CARTESIAN_POINT('',(-0.692459617039174,1.37475917892233E-5,1.04826868253652));
#37441=CARTESIAN_POINT('',(-0.692449505282264,9.96448218454668E-6,1.02673131746348));
#37442=CARTESIAN_POINT('',(-0.6925,-8.48067908409542E-17,0.895));
#37443=CARTESIAN_POINT('Ctrl Pts',(-0.692459617039174,1.37475917892232E-5,
1.04826868253652));
#37444=CARTESIAN_POINT('Ctrl Pts',(-0.692488936078667,0.0410896088323068,
1.04685284276779));
#37445=CARTESIAN_POINT('Ctrl Pts',(-0.688893820320347,0.0821603968297718,
1.04543700299906));
#37446=CARTESIAN_POINT('Ctrl Pts',(-0.681627147119585,0.122570961233086,
1.04402116323033));
#37447=CARTESIAN_POINT('Ctrl Pts',(-0.661228597323865,0.236008966146766,
1.04004670652542));
#37448=CARTESIAN_POINT('Ctrl Pts',(-0.611898100953193,0.34424439584463,
1.03607224982051));
#37449=CARTESIAN_POINT('Ctrl Pts',(-0.539661450787553,0.434056133192316,
1.03209779311559));
#37450=CARTESIAN_POINT('Ctrl Pts',(-0.467424800621913,0.523867870540003,
1.02812333641068));
#37451=CARTESIAN_POINT('Ctrl Pts',(-0.372281996661304,0.595255915537511,
1.02414887970577));
#37452=CARTESIAN_POINT('Ctrl Pts',(-0.265854872524943,0.6395001133563,1.02017442300085));
#37453=CARTESIAN_POINT('Ctrl Pts',(-0.159427748388581,0.68374431117509,
1.01619996629594));
#37454=CARTESIAN_POINT('Ctrl Pts',(-0.0417163040764662,0.700844661815162,
1.01222550959103));
#37455=CARTESIAN_POINT('Ctrl Pts',(0.0729008341367396,0.688712332262305,
1.00825105288611));
#37456=CARTESIAN_POINT('Ctrl Pts',(0.187517972349945,0.676580002709448,
1.0042765961812));
#37457=CARTESIAN_POINT('Ctrl Pts',(0.299040804464242,0.635214992963663,
1.00030213947629));
#37458=CARTESIAN_POINT('Ctrl Pts',(0.393846652298814,0.56967009988322,0.996327682771372));
#37459=CARTESIAN_POINT('Ctrl Pts',(0.488652500133385,0.504125206802777,
0.992353226066459));
#37460=CARTESIAN_POINT('Ctrl Pts',(0.566741363688231,0.414400430387678,
0.988378769361545));
#37461=CARTESIAN_POINT('Ctrl Pts',(0.618574573279787,0.311455784213055,
0.984404312656632));
#37462=CARTESIAN_POINT('Ctrl Pts',(0.670407782871342,0.208511138038433,
0.980429855951718));
#37463=CARTESIAN_POINT('Ctrl Pts',(0.695985338499608,0.0923466221042891,
0.976455399246806));
#37464=CARTESIAN_POINT('Ctrl Pts',(0.692182904076904,-0.0228480968935343,
0.972480942541892));
#37465=CARTESIAN_POINT('Ctrl Pts',(0.6883804696542,-0.138042815891358,0.968506485836979));
#37466=CARTESIAN_POINT('Ctrl Pts',(0.655198045180526,-0.25226773795286,
0.964532029132065));
#37467=CARTESIAN_POINT('Ctrl Pts',(0.596688912672601,-0.351570120632219,
0.960557572427152));
#37468=CARTESIAN_POINT('Ctrl Pts',(0.538179780164675,-0.450872503311578,
0.956583115722238));
#37469=CARTESIAN_POINT('Ctrl Pts',(0.454343939622498,-0.535252346608794,
0.952608659017325));
#37470=CARTESIAN_POINT('Ctrl Pts',(0.355422062432155,-0.594402528397402,
0.948634202312412));
#37471=CARTESIAN_POINT('Ctrl Pts',(0.256500185241811,-0.653552710186011,
0.944659745607498));
#37472=CARTESIAN_POINT('Ctrl Pts',(0.1424922714033,-0.687473230466012,0.940685288902585));
#37473=CARTESIAN_POINT('Ctrl Pts',(0.0273245554897345,-0.692020647736393,
0.936710832197671));
#37474=CARTESIAN_POINT('Ctrl Pts',(-0.0878431604238312,-0.696568065006773,
0.932736375492758));
#37475=CARTESIAN_POINT('Ctrl Pts',(-0.204170678412452,-0.671742379267533,
0.928761918787845));
#37476=CARTESIAN_POINT('Ctrl Pts',(-0.307448420839844,-0.62057608458131,
0.924787462082931));
#37477=CARTESIAN_POINT('Ctrl Pts',(-0.410726163267236,-0.569409789895086,
0.920813005378018));
#37478=CARTESIAN_POINT('Ctrl Pts',(-0.500954130133399,-0.491902886261879,
0.916838548673105));
#37479=CARTESIAN_POINT('Ctrl Pts',(-0.567110842408464,-0.397522956125345,
0.912864091968191));
#37480=CARTESIAN_POINT('Ctrl Pts',(-0.633267554683529,-0.303143025988812,
0.908889635263278));
#37481=CARTESIAN_POINT('Ctrl Pts',(-0.675353012367496,-0.191890069348953,
0.904915178558364));
#37482=CARTESIAN_POINT('Ctrl Pts',(-0.688226414825127,-0.0773537986570187,
0.900940721853451));
#37483=CARTESIAN_POINT('Ctrl Pts',(-0.691111357352151,-0.0516861044096396,
0.900050042081141));
#37484=CARTESIAN_POINT('Ctrl Pts',(-0.692529233545428,-0.0258535179808784,
0.89915936230883));
#37485=CARTESIAN_POINT('Ctrl Pts',(-0.692502505300729,-1.80142461571609E-5,
0.89826868253652));
#37486=CARTESIAN_POINT('Ctrl Pts',(-0.692519446907948,-1.67109334056352E-5,
0.87673131746348));
#37487=CARTESIAN_POINT('Ctrl Pts',(-0.692540216132119,-0.0205057905058466,
0.877437728882687));
#37488=CARTESIAN_POINT('Ctrl Pts',(-0.691649074693246,-0.0409930697662103,
0.878144140301895));
#37489=CARTESIAN_POINT('Ctrl Pts',(-0.689832948476493,-0.0613980215631428,
0.878850551721102));
#37490=CARTESIAN_POINT('Ctrl Pts',(-0.679614944034773,-0.176201654796807,
0.882825008426015));
#37491=CARTESIAN_POINT('Ctrl Pts',(-0.640116694711632,-0.288399225371522,
0.886799465130928));
#37492=CARTESIAN_POINT('Ctrl Pts',(-0.576162969353729,-0.384285632221807,
0.890773921835842));
#37493=CARTESIAN_POINT('Ctrl Pts',(-0.512209243995827,-0.480172039072091,
0.894748378540755));
#37494=CARTESIAN_POINT('Ctrl Pts',(-0.423800042603163,-0.559747282197946,
0.898722835245669));
#37495=CARTESIAN_POINT('Ctrl Pts',(-0.321734679564143,-0.613291129761764,
0.902697291950582));
#37496=CARTESIAN_POINT('Ctrl Pts',(-0.219669316525123,-0.666834977325583,
0.906671748655496));
#37497=CARTESIAN_POINT('Ctrl Pts',(-0.103947791839747,-0.694347429327364,
0.910646205360409));
#37498=CARTESIAN_POINT('Ctrl Pts',(0.0112943399504365,-0.692467798585378,
0.914620662065322));
#37499=CARTESIAN_POINT('Ctrl Pts',(0.12653647174062,-0.690588167843393,
0.918595118770236));
#37500=CARTESIAN_POINT('Ctrl Pts',(0.24129921063561,-0.659316454357642,
0.922569575475149));
#37501=CARTESIAN_POINT('Ctrl Pts',(0.341564119009619,-0.602472544311455,
0.926544032180063));
#37502=CARTESIAN_POINT('Ctrl Pts',(0.441829027383627,-0.545628634265269,
0.930518488884976));
#37503=CARTESIAN_POINT('Ctrl Pts',(0.527596105236653,-0.463212527658647,
0.934492945589889));
#37504=CARTESIAN_POINT('Ctrl Pts',(0.588388777731319,-0.365291473122074,
0.938467402294802));
#37505=CARTESIAN_POINT('Ctrl Pts',(0.649181450225985,-0.2673704185855,0.942441858999716));
#37506=CARTESIAN_POINT('Ctrl Pts',(0.684999717362292,-0.153944416118975,
0.946416315704629));
#37507=CARTESIAN_POINT('Ctrl Pts',(0.691468325045282,-0.0388686190472216,
0.950390772409543));
#37508=CARTESIAN_POINT('Ctrl Pts',(0.697936932728271,0.0762071780245319,
0.954365229114456));
#37509=CARTESIAN_POINT('Ctrl Pts',(0.675055880957944,0.192932769701512,
0.95833968581937));
#37510=CARTESIAN_POINT('Ctrl Pts',(0.625620123912279,0.297049953101773,
0.962314142524283));
#37511=CARTESIAN_POINT('Ctrl Pts',(0.576184366866613,0.401167136502033,
0.966288599229196));
#37512=CARTESIAN_POINT('Ctrl Pts',(0.500193904545608,0.492675911625573,
0.97026305593411));
#37513=CARTESIAN_POINT('Ctrl Pts',(0.406931083827991,0.560398346806577,
0.974237512639023));
#37514=CARTESIAN_POINT('Ctrl Pts',(0.313668263110376,0.628120781987582,
0.978211969343936));
#37515=CARTESIAN_POINT('Ctrl Pts',(0.203133083996148,0.672056877226051,
0.98218642604885));
#37516=CARTESIAN_POINT('Ctrl Pts',(0.0888275813995918,0.686839773795016,
0.986160882753763));
#37517=CARTESIAN_POINT('Ctrl Pts',(-0.0254779211969667,0.701622670363981,
0.990135339458677));
#37518=CARTESIAN_POINT('Ctrl Pts',(-0.143553747275854,0.68725236826344,
0.99410979616359));
#37519=CARTESIAN_POINT('Ctrl Pts',(-0.250976760793945,0.645484221052659,
0.998084252868503));
#37520=CARTESIAN_POINT('Ctrl Pts',(-0.358399774312035,0.603716073841877,
1.00205870957342));
#37521=CARTESIAN_POINT('Ctrl Pts',(-0.455169975269328,0.534550081520856,
1.00603316627833));
#37522=CARTESIAN_POINT('Ctrl Pts',(-0.529466741106335,0.446434971913998,
1.01000762298324));
#37523=CARTESIAN_POINT('Ctrl Pts',(-0.603763506943343,0.358319862307138,
1.01398207968816));
#37524=CARTESIAN_POINT('Ctrl Pts',(-0.655586837660064,0.251255635414442,
1.01795653639307));
#37525=CARTESIAN_POINT('Ctrl Pts',(-0.678606437090228,0.138320344221461,
1.02193099309798));
#37526=CARTESIAN_POINT('Ctrl Pts',(-0.68787408063104,0.092852827502517,
1.02353110121982));
#37527=CARTESIAN_POINT('Ctrl Pts',(-0.69247306823634,0.0464336986844112,
1.02513120934165));
#37528=CARTESIAN_POINT('Ctrl Pts',(-0.692449505282264,9.96448218454669E-6,
1.02673131746348));
#37529=CARTESIAN_POINT('Origin',(0.,0.,0.895));
#37530=CARTESIAN_POINT('',(-0.692553258028562,-7.52956544752825E-6,1.19826868253652));
#37531=CARTESIAN_POINT('',(-0.692559371888614,-2.09617465497895E-6,1.17673131746348));
#37532=CARTESIAN_POINT('',(-0.6925,-8.48067908409542E-17,0.895));
#37533=CARTESIAN_POINT('Ctrl Pts',(-0.692553258028562,-7.52956544752825E-6,
1.19826868253652));
#37534=CARTESIAN_POINT('Ctrl Pts',(-0.692493376955139,0.10794222829347,
1.19454632322675));
#37535=CARTESIAN_POINT('Ctrl Pts',(-0.666836185272269,0.215919453832076,
1.19082396391698));
#37536=CARTESIAN_POINT('Ctrl Pts',(-0.618163761380453,0.312270351368743,
1.18710160460721));
#37537=CARTESIAN_POINT('Ctrl Pts',(-0.566194989592747,0.415146629253594,
1.1831271479023));
#37538=CARTESIAN_POINT('Ctrl Pts',(-0.48798800092297,0.504768462738863,
1.17915269119739));
#37539=CARTESIAN_POINT('Ctrl Pts',(-0.393095894211433,0.570188412879551,
1.17517823449247));
#37540=CARTESIAN_POINT('Ctrl Pts',(-0.298203787499896,0.635608363020239,
1.17120377778756));
#37541=CARTESIAN_POINT('Ctrl Pts',(-0.186626562746599,0.676826429816346,
1.16722932108265));
#37542=CARTESIAN_POINT('Ctrl Pts',(-0.0719935422733182,0.688807765707478,
1.16325486437773));
#37543=CARTESIAN_POINT('Ctrl Pts',(0.042639478199963,0.70078910159861,1.15928040767282));
#37544=CARTESIAN_POINT('Ctrl Pts',(0.160328294393228,0.683533706584767,
1.15530595096791));
#37545=CARTESIAN_POINT('Ctrl Pts',(0.266697044089859,0.639149352578659,
1.15133149426299));
#37546=CARTESIAN_POINT('Ctrl Pts',(0.373065793786489,0.594764998572552,
1.14735703755808));
#37547=CARTESIAN_POINT('Ctrl Pts',(0.468114476986484,0.523251685574181,
1.14338258085317));
#37548=CARTESIAN_POINT('Ctrl Pts',(0.540232757060147,0.433344870082916,
1.13940812414825));
#37549=CARTESIAN_POINT('Ctrl Pts',(0.61235103713381,0.343438054591652,1.13543366744334));
#37550=CARTESIAN_POINT('Ctrl Pts',(0.661538914081142,0.235137736607494,
1.13145921073843));
#37551=CARTESIAN_POINT('Ctrl Pts',(0.681788016294753,0.121672959464514,
1.12748475403351));
#37552=CARTESIAN_POINT('Ctrl Pts',(0.702037118508365,0.00820818232153232,
1.1235102973286));
#37553=CARTESIAN_POINT('Ctrl Pts',(0.693347445988256,-0.110421053980272,
1.11953584062369));
#37554=CARTESIAN_POINT('Ctrl Pts',(0.656780455029912,-0.219724013523077,
1.11556138391877));
#37555=CARTESIAN_POINT('Ctrl Pts',(0.620213464071568,-0.329026973065883,
1.11158692721386));
#37556=CARTESIAN_POINT('Ctrl Pts',(0.555769154674989,-0.42900365584969,
1.10761247050895));
#37557=CARTESIAN_POINT('Ctrl Pts',(0.471319494139167,-0.507441762838246,
1.10363801380403));
#37558=CARTESIAN_POINT('Ctrl Pts',(0.386869833603345,-0.585879869826803,
1.09966355709912));
#37559=CARTESIAN_POINT('Ctrl Pts',(0.28241482192828,-0.642779401020109,
1.09568910039421));
#37560=CARTESIAN_POINT('Ctrl Pts',(0.170713792619461,-0.671189994887787,
1.09171464368929));
#37561=CARTESIAN_POINT('Ctrl Pts',(0.0590127633106426,-0.699600588755465,
1.08774018698438));
#37562=CARTESIAN_POINT('Ctrl Pts',(-0.0599342836319292,-0.699522245297516,
1.08376573027947));
#37563=CARTESIAN_POINT('Ctrl Pts',(-0.171597791252629,-0.670964534282704,
1.07979127357455));
#37564=CARTESIAN_POINT('Ctrl Pts',(-0.283261298873331,-0.642406823267892,
1.07581681686964));
#37565=CARTESIAN_POINT('Ctrl Pts',(-0.38764126717216,-0.585369744696218,
1.07184236016473));
#37566=CARTESIAN_POINT('Ctrl Pts',(-0.47198752930255,-0.506820461712886,
1.06786790345981));
#37567=CARTESIAN_POINT('Ctrl Pts',(-0.556333791432939,-0.428271178729555,
1.0638934467549));
#37568=CARTESIAN_POINT('Ctrl Pts',(-0.62064634739489,-0.328209691334567,
1.05991899004999));
#37569=CARTESIAN_POINT('Ctrl Pts',(-0.657069323765481,-0.218858657572326,
1.05594453334507));
#37570=CARTESIAN_POINT('Ctrl Pts',(-0.680517168622571,-0.148462266883901,
1.05338591640889));
#37571=CARTESIAN_POINT('Ctrl Pts',(-0.692406633507664,-0.0742159756859151,
1.0508272994727));
#37572=CARTESIAN_POINT('Ctrl Pts',(-0.692459617039174,1.37475917892232E-5,
1.04826868253652));
#37573=CARTESIAN_POINT('Ctrl Pts',(-0.692449505282264,9.96448218454669E-6,
1.02673131746348));
#37574=CARTESIAN_POINT('Ctrl Pts',(-0.692414540978377,-0.0688767101246464,
1.02910566604656));
#37575=CARTESIAN_POINT('Ctrl Pts',(-0.68220135351308,-0.137773525156493,
1.03148001462964));
#37576=CARTESIAN_POINT('Ctrl Pts',(-0.661960581745391,-0.203586350969775,
1.03385436321272));
#37577=CARTESIAN_POINT('Ctrl Pts',(-0.628079258826783,-0.313751399474762,
1.03782881991764));
#37578=CARTESIAN_POINT('Ctrl Pts',(-0.566100744845961,-0.41527514099147,
1.04180327662255));
#37579=CARTESIAN_POINT('Ctrl Pts',(-0.483595806560603,-0.495756300981426,
1.04577773332746));
#37580=CARTESIAN_POINT('Ctrl Pts',(-0.401090868275244,-0.576237460971383,
1.04975219003238));
#37581=CARTESIAN_POINT('Ctrl Pts',(-0.298059505685348,-0.635676039434589,
1.05372664673729));
#37582=CARTESIAN_POINT('Ctrl Pts',(-0.187087151464033,-0.666811526477261,
1.0577011034422));
#37583=CARTESIAN_POINT('Ctrl Pts',(-0.0761147972427186,-0.697947013519933,
1.06167556014712));
#37584=CARTESIAN_POINT('Ctrl Pts',(0.0427985486100149,-0.700779409142074,
1.06565001685203));
#37585=CARTESIAN_POINT('Ctrl Pts',(0.155127445776281,-0.674962732047294,
1.06962447355694));
#37586=CARTESIAN_POINT('Ctrl Pts',(0.267456342942549,-0.649146054952514,
1.07359893026186));
#37587=CARTESIAN_POINT('Ctrl Pts',(0.373200791422349,-0.594680305140813,
1.07757338696677));
#37588=CARTESIAN_POINT('Ctrl Pts',(0.459443951105567,-0.518218554162569,
1.08154784367168));
#37589=CARTESIAN_POINT('Ctrl Pts',(0.545687110788785,-0.441756803184324,
1.0855223003766));
#37590=CARTESIAN_POINT('Ctrl Pts',(0.612428981675421,-0.343299051039535,
1.08949675708151));
#37591=CARTESIAN_POINT('Ctrl Pts',(0.651516945946883,-0.234872057150013,
1.09347121378642));
#37592=CARTESIAN_POINT('Ctrl Pts',(0.690604910218345,-0.12644506326049,
1.09744567049134));
#37593=CARTESIAN_POINT('Ctrl Pts',(0.702038967874634,-0.0080488276262343,
1.10142012719625));
#37594=CARTESIAN_POINT('Ctrl Pts',(0.684422431934264,0.105854375209623,
1.10539458390116));
#37595=CARTESIAN_POINT('Ctrl Pts',(0.666805895993895,0.21975757804548,1.10936904060608));
#37596=CARTESIAN_POINT('Ctrl Pts',(0.620138766456867,0.329167748082939,
1.11334349731099));
#37597=CARTESIAN_POINT('Ctrl Pts',(0.550121501922133,0.420720271925147,
1.1173179540159));
#37598=CARTESIAN_POINT('Ctrl Pts',(0.480104237387399,0.512272795767356,
1.12129241072082));
#37599=CARTESIAN_POINT('Ctrl Pts',(0.38673683785496,0.585967673414315,1.12526686742573));
#37600=CARTESIAN_POINT('Ctrl Pts',(0.281424268678516,0.632802967032073,
1.12924132413064));
#37601=CARTESIAN_POINT('Ctrl Pts',(0.176111699502072,0.679638260649832,
1.13321578083556));
#37602=CARTESIAN_POINT('Ctrl Pts',(0.0588539606816214,0.699613970238391,
1.13719023754047));
#37603=CARTESIAN_POINT('Ctrl Pts',(-0.056025742302142,0.690290033453567,
1.14116469424538));
#37604=CARTESIAN_POINT('Ctrl Pts',(-0.170905445285905,0.680966096668744,
1.1451391509503));
#37605=CARTESIAN_POINT('Ctrl Pts',(-0.283407112432982,0.642342513510539,
1.14911360765521));
#37606=CARTESIAN_POINT('Ctrl Pts',(-0.379788499421787,0.579137211542119,
1.15308806436013));
#37607=CARTESIAN_POINT('Ctrl Pts',(-0.476169886410592,0.515931909573698,
1.15706252106504));
#37608=CARTESIAN_POINT('Ctrl Pts',(-0.556430993241123,0.428144888795061,
1.16103697776995));
#37609=CARTESIAN_POINT('Ctrl Pts',(-0.610767807514664,0.326499463076991,
1.16501143447486));
#37610=CARTESIAN_POINT('Ctrl Pts',(-0.664177296537632,0.226588742846052,
1.16891806213774));
#37611=CARTESIAN_POINT('Ctrl Pts',(-0.692539802909692,0.11328860312279,
1.17282468980061));
#37612=CARTESIAN_POINT('Ctrl Pts',(-0.692559371888614,-2.09617465497895E-6,
1.17673131746348));
#37613=CARTESIAN_POINT('Origin',(0.,0.,0.895));
#37614=CARTESIAN_POINT('',(-0.692440804635195,-1.82486148905814E-6,1.34826868253652));
#37615=CARTESIAN_POINT('',(-0.692444362555486,-6.68421405300118E-6,1.32673131746348));
#37616=CARTESIAN_POINT('',(-0.6925,-8.48067908409542E-17,0.895));
#37617=CARTESIAN_POINT('Ctrl Pts',(-0.692440804635195,-1.82486148905814E-6,
1.34826868253652));
#37618=CARTESIAN_POINT('Ctrl Pts',(-0.692435348926581,0.0596050059372995,
1.34621426039063));
#37619=CARTESIAN_POINT('Ctrl Pts',(-0.684818864295023,0.119213205203163,
1.34415983824473));
#37620=CARTESIAN_POINT('Ctrl Pts',(-0.669608294980035,0.176816117822777,
1.34210541609884));
#37621=CARTESIAN_POINT('Ctrl Pts',(-0.640182137692788,0.288253916885169,
1.33813095939392));
#37622=CARTESIAN_POINT('Ctrl Pts',(-0.582334178987605,0.392186682593103,
1.33415650268901));
#37623=CARTESIAN_POINT('Ctrl Pts',(-0.503130632212173,0.475918874555073,
1.3301820459841));
#37624=CARTESIAN_POINT('Ctrl Pts',(-0.423927085436742,0.559651066517042,
1.32620758927918));
#37625=CARTESIAN_POINT('Ctrl Pts',(-0.323367950591062,0.623182684733047,
1.32223313257427));
#37626=CARTESIAN_POINT('Ctrl Pts',(-0.213736674088512,0.658753248475913,
1.31825867586936));
#37627=CARTESIAN_POINT('Ctrl Pts',(-0.104105397585963,0.69432381221878,
1.31428421916444));
#37628=CARTESIAN_POINT('Ctrl Pts',(0.0145980205734564,0.701933321488508,
1.31030976245953));
#37629=CARTESIAN_POINT('Ctrl Pts',(0.12787378304877,0.680652263521384,1.30633530575461));
#37630=CARTESIAN_POINT('Ctrl Pts',(0.241149545524084,0.659371205554261,
1.3023608490497));
#37631=CARTESIAN_POINT('Ctrl Pts',(0.348997652315293,0.609199580350287,
1.29838639234479));
#37632=CARTESIAN_POINT('Ctrl Pts',(0.438244298351508,0.536265925815152,
1.29441193563988));
#37633=CARTESIAN_POINT('Ctrl Pts',(0.527490944387723,0.463332271280017,
1.29043747893496));
#37634=CARTESIAN_POINT('Ctrl Pts',(0.598136129668944,0.367636587413722,
1.28646302223005));
#37635=CARTESIAN_POINT('Ctrl Pts',(0.641550440774931,0.26086824293018,1.28248856552513));
#37636=CARTESIAN_POINT('Ctrl Pts',(0.684964751880918,0.154099898446638,
1.27851410882022));
#37637=CARTESIAN_POINT('Ctrl Pts',(0.701148188811671,0.0362588933458479,
1.27453965211531));
#37638=CARTESIAN_POINT('Ctrl Pts',(0.688123920912985,-0.0782603200563889,
1.2705651954104));
#37639=CARTESIAN_POINT('Ctrl Pts',(0.675099653014299,-0.192779533458624,
1.26659073870548));
#37640=CARTESIAN_POINT('Ctrl Pts',(0.632867680286175,-0.303976955162307,
1.26261628200057));
#37641=CARTESIAN_POINT('Ctrl Pts',(0.566586700391767,-0.398269656347502,
1.25864182529565));
#37642=CARTESIAN_POINT('Ctrl Pts',(0.500305720497359,-0.492562357532699,
1.25466736859074));
#37643=CARTESIAN_POINT('Ctrl Pts',(0.409975733436666,-0.569950338199408,
1.25069291188583));
#37644=CARTESIAN_POINT('Ctrl Pts',(0.306630680156813,-0.620980542541035,
1.24671845518091));
#37645=CARTESIAN_POINT('Ctrl Pts',(0.203285626876962,-0.672010746882661,
1.242743998476));
#37646=CARTESIAN_POINT('Ctrl Pts',(0.0869255073779509,-0.696683174899206,
1.23876954177109));
#37647=CARTESIAN_POINT('Ctrl Pts',(-0.0282361183815551,-0.691984053173721,
1.23479508506617));
#37648=CARTESIAN_POINT('Ctrl Pts',(-0.143397744141063,-0.687284931448236,
1.23082062836126));
#37649=CARTESIAN_POINT('Ctrl Pts',(-0.257360876161066,-0.65321425998072,
1.22684617165635));
#37650=CARTESIAN_POINT('Ctrl Pts',(-0.35620475003347,-0.593933821466316,
1.22287171495143));
#37651=CARTESIAN_POINT('Ctrl Pts',(-0.455048623905873,-0.534653382951911,
1.21889725824652));
#37652=CARTESIAN_POINT('Ctrl Pts',(-0.538773239630678,-0.450163177390616,
1.21492280154161));
#37653=CARTESIAN_POINT('Ctrl Pts',(-0.597151512097071,-0.350783807819245,
1.21094834483669));
#37654=CARTESIAN_POINT('Ctrl Pts',(-0.655529784563464,-0.251404438247874,
1.20697388813178));
#37655=CARTESIAN_POINT('Ctrl Pts',(-0.688561713771447,-0.137135904666427,
1.20299943142687));
#37656=CARTESIAN_POINT('Ctrl Pts',(-0.692212400922621,-0.0219362767334871,
1.19902497472195));
#37657=CARTESIAN_POINT('Ctrl Pts',(-0.692443961809965,-0.0146292337135863,
1.19877287732681));
#37658=CARTESIAN_POINT('Ctrl Pts',(-0.692557313484087,-0.00731844463249064,
1.19852077993167));
#37659=CARTESIAN_POINT('Ctrl Pts',(-0.692553258028562,-7.52956544752825E-6,
1.19826868253652));
#37660=CARTESIAN_POINT('Ctrl Pts',(-0.692559371888614,-2.09617465497895E-6,
1.17673131746348));
#37661=CARTESIAN_POINT('Ctrl Pts',(-0.692559711656109,-0.0019691122992305,
1.17679914650552));
#37662=CARTESIAN_POINT('Ctrl Pts',(-0.692551507208319,-0.00393612557791079,
1.17686697554756));
#37663=CARTESIAN_POINT('Ctrl Pts',(-0.69253474129393,-0.00590306587988918,
1.17693480458961));
#37664=CARTESIAN_POINT('Ctrl Pts',(-0.691552339083105,-0.121156338461197,
1.18090926129452));
#37665=CARTESIAN_POINT('Ctrl Pts',(-0.661175012944903,-0.236159052966311,
1.18488371799943));
#37666=CARTESIAN_POINT('Ctrl Pts',(-0.605113398003355,-0.336863458455597,
1.18885817470434));
#37667=CARTESIAN_POINT('Ctrl Pts',(-0.549051783061807,-0.437567863944884,
1.19283263140926));
#37668=CARTESIAN_POINT('Ctrl Pts',(-0.467305879316914,-0.523973960418344,
1.19680708811417));
#37669=CARTESIAN_POINT('Ctrl Pts',(-0.369861069297117,-0.585527115942743,
1.20078154481909));
#37670=CARTESIAN_POINT('Ctrl Pts',(-0.272416259277321,-0.647080271467141,
1.204756001524));
#37671=CARTESIAN_POINT('Ctrl Pts',(-0.159272542982623,-0.683780486042478,
1.20873045822891));
#37672=CARTESIAN_POINT('Ctrl Pts',(-0.0442505919835302,-0.6911447744105,
1.21270491493383));
#37673=CARTESIAN_POINT('Ctrl Pts',(0.0707713590155626,-0.698509062778522,
1.21667937163874));
#37674=CARTESIAN_POINT('Ctrl Pts',(0.18767154471905,-0.67653742493923,1.22065382834365));
#37675=CARTESIAN_POINT('Ctrl Pts',(0.292170435286043,-0.627913728812006,
1.22462828504857));
#37676=CARTESIAN_POINT('Ctrl Pts',(0.396669325853035,-0.579290032684783,
1.22860274175348));
#37677=CARTESIAN_POINT('Ctrl Pts',(0.488766921283533,-0.504014278269628,
1.23257719845839));
#37678=CARTESIAN_POINT('Ctrl Pts',(0.55721336466491,-0.411281509825865,
1.23655165516331));
#37679=CARTESIAN_POINT('Ctrl Pts',(0.625659808046288,-0.3185487413821,1.24052611186822));
#37680=CARTESIAN_POINT('Ctrl Pts',(0.670455099378544,-0.208358958909726,
1.24450056857313));
#37681=CARTESIAN_POINT('Ctrl Pts',(0.686127427856067,-0.0941720066126366,
1.24847502527805));
#37682=CARTESIAN_POINT('Ctrl Pts',(0.70179975633359,0.0200149456844525,
1.25244948198296));
#37683=CARTESIAN_POINT('Ctrl Pts',(0.688349121956381,0.138199067806256,
1.25642393868787));
#37684=CARTESIAN_POINT('Ctrl Pts',(0.647418539522168,0.245943995187554,
1.26039839539279));
#37685=CARTESIAN_POINT('Ctrl Pts',(0.606487957087956,0.353688922568853,
1.2643728520977));
#37686=CARTESIAN_POINT('Ctrl Pts',(0.538077426596741,0.450994655209645,
1.26834730880261));
#37687=CARTESIAN_POINT('Ctrl Pts',(0.450543395095222,0.525975154567118,
1.27232176550753));
#37688=CARTESIAN_POINT('Ctrl Pts',(0.363009363593702,0.600955653924592,
1.27629622221244));
#37689=CARTESIAN_POINT('Ctrl Pts',(0.256351831081878,0.653610919998746,
1.28027067891735));
#37690=CARTESIAN_POINT('Ctrl Pts',(0.143599172229069,0.677509034493976,
1.28424513562227));
#37691=CARTESIAN_POINT('Ctrl Pts',(0.0308465133762598,0.701407148989206,
1.28821959232718));
#37692=CARTESIAN_POINT('Ctrl Pts',(-0.0880012718175337,0.696548111905513,
1.29219404903209));
#37693=CARTESIAN_POINT('Ctrl Pts',(-0.198426751365481,0.663525461778502,
1.29616850573701));
#37694=CARTESIAN_POINT('Ctrl Pts',(-0.308852230913428,0.630502811651492,
1.30014296244192));
#37695=CARTESIAN_POINT('Ctrl Pts',(-0.410855404815529,0.569316548481164,
1.30411741914683));
#37696=CARTESIAN_POINT('Ctrl Pts',(-0.491976435161048,0.487440664421897,
1.30809187585175));
#37697=CARTESIAN_POINT('Ctrl Pts',(-0.573097465506566,0.40556478036263,
1.31206633255666));
#37698=CARTESIAN_POINT('Ctrl Pts',(-0.633336352295502,0.302999275414424,
1.31604078926157));
#37699=CARTESIAN_POINT('Ctrl Pts',(-0.665334826793653,0.192272677053432,
1.32001524596649));
#37700=CARTESIAN_POINT('Ctrl Pts',(-0.683358593602554,0.129903754168789,
1.32225393646548));
#37701=CARTESIAN_POINT('Ctrl Pts',(-0.692422451300573,0.0649455399355973,
1.32449262696448));
#37702=CARTESIAN_POINT('Ctrl Pts',(-0.692444362555486,-6.68421405300118E-6,
1.32673131746348));
#37703=CARTESIAN_POINT('Origin',(0.,0.,0.895));
#37704=CARTESIAN_POINT('',(-0.692545368475526,1.10096728344264E-5,1.49826868253652));
#37705=CARTESIAN_POINT('',(-0.692531307667519,1.47955152054312E-5,1.47673131746348));
#37706=CARTESIAN_POINT('',(-0.6925,-8.48067908409542E-17,0.895));
#37707=CARTESIAN_POINT('Ctrl Pts',(-0.692545368475526,1.10096728344264E-5,
1.49826868253652));
#37708=CARTESIAN_POINT('Ctrl Pts',(-0.692553862205703,0.0112195835652045,
1.4978821975545));
#37709=CARTESIAN_POINT('Ctrl Pts',(-0.692287383186695,0.0224277534934861,
1.49749571257248));
#37710=CARTESIAN_POINT('Ctrl Pts',(-0.691743262005351,0.0336224285249397,
1.49710922759046));
#37711=CARTESIAN_POINT('Ctrl Pts',(-0.686147737785575,0.148743981257509,
1.49313477088554));
#37712=CARTESIAN_POINT('Ctrl Pts',(-0.651190884302411,0.262438416055945,
1.48916031418063));
#37713=CARTESIAN_POINT('Ctrl Pts',(-0.591142732692494,0.360817790316279,
1.48518585747572));
#37714=CARTESIAN_POINT('Ctrl Pts',(-0.531094581082575,0.459197164576613,
1.4812114007708));
#37715=CARTESIAN_POINT('Ctrl Pts',(-0.445955131345907,0.542261478298842,
1.47723694406589));
#37716=CARTESIAN_POINT('Ctrl Pts',(-0.346124292649832,0.599864303212682,
1.47326248736098));
#37717=CARTESIAN_POINT('Ctrl Pts',(-0.246293453953757,0.657467128126522,
1.46928803065606));
#37718=CARTESIAN_POINT('Ctrl Pts',(-0.131771226298275,0.68960846423197,
1.46531357395115));
#37719=CARTESIAN_POINT('Ctrl Pts',(-0.0165466684475456,0.692362200000473,
1.46133911724624));
#37720=CARTESIAN_POINT('Ctrl Pts',(0.0986778894031835,0.695115935768976,
1.45736466054132));
#37721=CARTESIAN_POINT('Ctrl Pts',(0.214604777449164,0.668482071200535,
1.45339020383641));
#37722=CARTESIAN_POINT('Ctrl Pts',(0.31707335559214,0.61571397207006,1.4494157471315));
#37723=CARTESIAN_POINT('Ctrl Pts',(0.419541933735116,0.562945872939585,
1.44544129042658));
#37724=CARTESIAN_POINT('Ctrl Pts',(0.508552201975089,0.484043539247076,
1.44146683372167));
#37725=CARTESIAN_POINT('Ctrl Pts',(0.573231424962209,0.388645007254125,
1.43749237701676));
#37726=CARTESIAN_POINT('Ctrl Pts',(0.63791064794933,0.293246475261173,1.43351792031184));
#37727=CARTESIAN_POINT('Ctrl Pts',(0.678258825683598,0.181351744967778,
1.42954346360693));
#37728=CARTESIAN_POINT('Ctrl Pts',(0.689347368834701,0.066628922463654,
1.42556900690202));
#37729=CARTESIAN_POINT('Ctrl Pts',(0.700435911985803,-0.0480939000404694,
1.4215945501971));
#37730=CARTESIAN_POINT('Ctrl Pts',(0.68226482055374,-0.16564481475532,1.41762009349219));
#37731=CARTESIAN_POINT('Ctrl Pts',(0.637053720117189,-0.271664804332269,
1.41364563678728));
#37732=CARTESIAN_POINT('Ctrl Pts',(0.591842619680638,-0.377684793909216,
1.40967118008236));
#37733=CARTESIAN_POINT('Ctrl Pts',(0.5195915102396,-0.47217385834826,1.40569672337745));
#37734=CARTESIAN_POINT('Ctrl Pts',(0.429125971215483,-0.543590019275841,
1.40172226667254));
#37735=CARTESIAN_POINT('Ctrl Pts',(0.338660432191365,-0.615006180203423,
1.39774780996762));
#37736=CARTESIAN_POINT('Ctrl Pts',(0.229980463584167,-0.663349437619542,
1.39377335326271));
#37737=CARTESIAN_POINT('Ctrl Pts',(0.116361483610661,-0.682714591436233,
1.3897988965578));
#37738=CARTESIAN_POINT('Ctrl Pts',(0.00274250363715367,-0.702079745252923,
1.38582443985288));
#37739=CARTESIAN_POINT('Ctrl Pts',(-0.115815487702663,-0.692466795470184,
1.38184998314797));
#37740=CARTESIAN_POINT('Ctrl Pts',(-0.22483045716799,-0.655049978060916,
1.37787552644306));
#37741=CARTESIAN_POINT('Ctrl Pts',(-0.333845426633318,-0.617633160651648,
1.37390106973814));
#37742=CARTESIAN_POINT('Ctrl Pts',(-0.433317374224156,-0.552412475615852,
1.36992661303323));
#37743=CARTESIAN_POINT('Ctrl Pts',(-0.511095655051393,-0.467354725680162,
1.36595215632832));
#37744=CARTESIAN_POINT('Ctrl Pts',(-0.58887393587863,-0.382296975744473,
1.3619776996234));
#37745=CARTESIAN_POINT('Ctrl Pts',(-0.644958549942266,-0.277402160908889,
1.35800324291849));
#37746=CARTESIAN_POINT('Ctrl Pts',(-0.672498679039428,-0.165483337282674,
1.35402878621358));
#37747=CARTESIAN_POINT('Ctrl Pts',(-0.685803138881955,-0.111416070956344,
1.35210875165456));
#37748=CARTESIAN_POINT('Ctrl Pts',(-0.692445903465104,-0.0557095455536165,
1.35018871709554));
#37749=CARTESIAN_POINT('Ctrl Pts',(-0.692440804635195,-1.82486148905814E-6,
1.34826868253652));
#37750=CARTESIAN_POINT('Ctrl Pts',(-0.692444362555486,-6.68421405300118E-6,
1.32673131746348));
#37751=CARTESIAN_POINT('Ctrl Pts',(-0.692461351422783,-0.0503673194731426,
1.3284670836694));
#37752=CARTESIAN_POINT('Ctrl Pts',(-0.687042630329724,-0.10072435369821,
1.33020284987531));
#37753=CARTESIAN_POINT('Ctrl Pts',(-0.676149960582673,-0.14986809163355,
1.33193861608123));
#37754=CARTESIAN_POINT('Ctrl Pts',(-0.651208557666179,-0.262394570185764,
1.33591307278614));
#37755=CARTESIAN_POINT('Ctrl Pts',(-0.597567689625827,-0.368559835516417,
1.33988752949105));
#37756=CARTESIAN_POINT('Ctrl Pts',(-0.521779667488874,-0.455395644117324,
1.34386198619597));
#37757=CARTESIAN_POINT('Ctrl Pts',(-0.445991645351922,-0.54223145271823,
1.34783644290088));
#37758=CARTESIAN_POINT('Ctrl Pts',(-0.34805646911837,-0.609737804589392,
1.35181089960579));
#37759=CARTESIAN_POINT('Ctrl Pts',(-0.239937064792858,-0.64966869943412,
1.35578535631071));
#37760=CARTESIAN_POINT('Ctrl Pts',(-0.131817660467342,-0.68959959427885,
1.35975981301562));
#37761=CARTESIAN_POINT('Ctrl Pts',(-0.0135140280498643,-0.701955032097146,
1.36373426972053));
#37762=CARTESIAN_POINT('Ctrl Pts',(0.100522869535734,-0.685225777963829,
1.36770872642545));
#37763=CARTESIAN_POINT('Ctrl Pts',(0.214559767121331,-0.668496523830512,
1.37168318313036));
#37764=CARTESIAN_POINT('Ctrl Pts',(0.32432992987505,-0.622682577745584,
1.37565763983527));
#37765=CARTESIAN_POINT('Ctrl Pts',(0.416424770759598,-0.553380180692849,
1.37963209654019));
#37766=CARTESIAN_POINT('Ctrl Pts',(0.508519611644146,-0.484077783640114,
1.3836065532451));
#37767=CARTESIAN_POINT('Ctrl Pts',(0.582939130659523,-0.391286935619573,
1.38758100995001));
#37768=CARTESIAN_POINT('Ctrl Pts',(0.630592873961455,-0.286342175368675,
1.39155546665493));
#37769=CARTESIAN_POINT('Ctrl Pts',(0.678246617263387,-0.181397415117777,
1.39552992335984));
#37770=CARTESIAN_POINT('Ctrl Pts',(0.699134584851872,-0.0642987426365235,
1.39950438006475));
#37771=CARTESIAN_POINT('Ctrl Pts',(0.690705280724573,0.0506500667819962,
1.40347883676967));
#37772=CARTESIAN_POINT('Ctrl Pts',(0.682275976597274,0.165598876200516,
1.40745329347458));
#37773=CARTESIAN_POINT('Ctrl Pts',(0.64452940075419,0.278397822556301,1.41142775017949));
#37774=CARTESIAN_POINT('Ctrl Pts',(0.582076353023386,0.375268348434599,
1.41540220688441));
#37775=CARTESIAN_POINT('Ctrl Pts',(0.519623305292582,0.472138874312898,
1.41937666358932));
#37776=CARTESIAN_POINT('Ctrl Pts',(0.432463785674058,0.553080979713709,
1.42335112029423));
#37777=CARTESIAN_POINT('Ctrl Pts',(0.331244457847782,0.608207467260103,
1.42732557699915));
#37778=CARTESIAN_POINT('Ctrl Pts',(0.230025130021506,0.663333954806497,
1.43130003370406));
#37779=CARTESIAN_POINT('Ctrl Pts',(0.114745993987475,0.692644824498473,
1.43527449040897));
#37780=CARTESIAN_POINT('Ctrl Pts',(-0.00051143401784693,0.692559710437379,
1.43924894711389));
#37781=CARTESIAN_POINT('Ctrl Pts',(-0.11576886202317,0.692474596376285,
1.4432234038188));
#37782=CARTESIAN_POINT('Ctrl Pts',(-0.231004581999785,0.662993498562121,
1.44719786052371));
#37783=CARTESIAN_POINT('Ctrl Pts',(-0.332142381046561,0.607717576509441,
1.45117231722863));
#37784=CARTESIAN_POINT('Ctrl Pts',(-0.433280180093337,0.552441654456761,
1.45514677393354));
#37785=CARTESIAN_POINT('Ctrl Pts',(-0.520320058210273,0.471370908165566,
1.45912123063845));
#37786=CARTESIAN_POINT('Ctrl Pts',(-0.582629966103052,0.374408248686699,
1.46309568734337));
#37787=CARTESIAN_POINT('Ctrl Pts',(-0.64493987399583,0.277445589207832,
1.46707014404828));
#37788=CARTESIAN_POINT('Ctrl Pts',(-0.68251981166445,0.164591016541294,
1.47104460075319));
#37789=CARTESIAN_POINT('Ctrl Pts',(-0.6907793343792,0.0496298829382655,
1.47501905745811));
#37790=CARTESIAN_POINT('Ctrl Pts',(-0.691965446214347,0.0331208465377808,
1.47558981079323));
#37791=CARTESIAN_POINT('Ctrl Pts',(-0.692546897704824,0.0165683675781126,
1.47616056412836));
#37792=CARTESIAN_POINT('Ctrl Pts',(-0.692531307667519,1.47955152054312E-5,
1.47673131746348));
#37793=CARTESIAN_POINT('Origin',(0.,0.,0.895));
#37794=CARTESIAN_POINT('',(-0.692468966846601,-1.59520066716212E-5,1.64826868253652));
#37795=CARTESIAN_POINT('',(-0.692483926679543,-1.76726015421153E-5,1.62673131746348));
#37796=CARTESIAN_POINT('',(-0.6925,-8.48067908409542E-17,0.895));
#37797=CARTESIAN_POINT('Ctrl Pts',(-0.692468966846601,-1.59520066716212E-5,
1.64826868253652));
#37798=CARTESIAN_POINT('Ctrl Pts',(-0.692403402184756,0.078109577227228,
1.64557567801346));
#37799=CARTESIAN_POINT('Ctrl Pts',(-0.679206900677884,0.156256752068032,
1.6428826734904));
#37800=CARTESIAN_POINT('Ctrl Pts',(-0.653279802282823,0.229923313136639,
1.64018966896734));
#37801=CARTESIAN_POINT('Ctrl Pts',(-0.61501542909934,0.33864372376346,1.63621521226242));
#37802=CARTESIAN_POINT('Ctrl Pts',(-0.549022315525714,0.437604829530587,
1.63224075555751));
#37803=CARTESIAN_POINT('Ctrl Pts',(-0.463361629978389,0.514718550810581,
1.6282662988526));
#37804=CARTESIAN_POINT('Ctrl Pts',(-0.377700944431063,0.591832272090574,
1.62429184214769));
#37805=CARTESIAN_POINT('Ctrl Pts',(-0.272372686910038,0.647098608883435,
1.62031738544277));
#37806=CARTESIAN_POINT('Ctrl Pts',(-0.160242852952848,0.673766613758384,
1.61634292873786));
#37807=CARTESIAN_POINT('Ctrl Pts',(-0.0481130189956584,0.700434618633334,
1.61236847203294));
#37808=CARTESIAN_POINT('Ctrl Pts',(0.0708183913976963,0.698504291590372,
1.60839401532803));
#37809=CARTESIAN_POINT('Ctrl Pts',(0.182023728166554,0.668211466628036,
1.60441955862312));
#37810=CARTESIAN_POINT('Ctrl Pts',(0.293229064935411,0.6379186416657,1.6004451019182));
#37811=CARTESIAN_POINT('Ctrl Pts',(0.396708328079772,0.579263318783989,
1.59647064521329));
#37812=CARTESIAN_POINT('Ctrl Pts',(0.479821374788218,0.499410311096158,
1.59249618850838));
#37813=CARTESIAN_POINT('Ctrl Pts',(0.562934421496663,0.419557303408327,
1.58852173180346));
#37814=CARTESIAN_POINT('Ctrl Pts',(0.625681251769195,0.318506610914376,
1.58454727509855));
#37815=CARTESIAN_POINT('Ctrl Pts',(0.660397247090718,0.208601735049309,
1.58057281839364));
#37816=CARTESIAN_POINT('Ctrl Pts',(0.69511324241224,0.0986968591842446,
1.57659836168873));
#37817=CARTESIAN_POINT('Ctrl Pts',(0.701798402782755,-0.0200622000519314,
1.57262390498381));
#37818=CARTESIAN_POINT('Ctrl Pts',(0.679636126415314,-0.133168853970496,
1.5686494482789));
#37819=CARTESIAN_POINT('Ctrl Pts',(0.657473850047873,-0.246275507889063,
1.56467499157399));
#37820=CARTESIAN_POINT('Ctrl Pts',(0.606464136942474,-0.353729756490014,
1.56070053486907));
#37821=CARTESIAN_POINT('Ctrl Pts',(0.532837898476493,-0.442405902401399,
1.55672607816416));
#37822=CARTESIAN_POINT('Ctrl Pts',(0.459211660010513,-0.531082048312783,
1.55275162145925));
#37823=CARTESIAN_POINT('Ctrl Pts',(0.36296889618395,-0.600980091534601,
1.54877716475433));
#37824=CARTESIAN_POINT('Ctrl Pts',(0.255865802433896,-0.643561884485609,
1.54480270804942));
#37825=CARTESIAN_POINT('Ctrl Pts',(0.148762708683842,-0.686143677436617,
1.5408282513445));
#37826=CARTESIAN_POINT('Ctrl Pts',(0.0307992850102965,-0.701409220116816,
1.53685379463959));
#37827=CARTESIAN_POINT('Ctrl Pts',(-0.0836150627124207,-0.687493803335081,
1.53287933793468));
#37828=CARTESIAN_POINT('Ctrl Pts',(-0.198029410435138,-0.673578386553346,
1.52890488122976));
#37829=CARTESIAN_POINT('Ctrl Pts',(-0.308894682207027,-0.630482010309677,
1.52493042452485));
#37830=CARTESIAN_POINT('Ctrl Pts',(-0.402668521786135,-0.563468960767016,
1.52095596781994));
#37831=CARTESIAN_POINT('Ctrl Pts',(-0.496442361365244,-0.496455911224355,
1.51698151111502));
#37832=CARTESIAN_POINT('Ctrl Pts',(-0.573124768751571,-0.4055261883827,
1.51300705441011));
#37833=CARTESIAN_POINT('Ctrl Pts',(-0.623348874966542,-0.301786991628521,
1.5090325977052));
#37834=CARTESIAN_POINT('Ctrl Pts',(-0.668689077737925,-0.208135624373867,
1.50544462598231));
#37835=CARTESIAN_POINT('Ctrl Pts',(-0.692466516087684,-0.104044899484275,
1.50185665425941));
#37836=CARTESIAN_POINT('Ctrl Pts',(-0.692545368475526,1.10096728344264E-5,
1.49826868253652));
#37837=CARTESIAN_POINT('Ctrl Pts',(-0.692531307667519,1.47955152054312E-5,
1.47673131746348));
#37838=CARTESIAN_POINT('Ctrl Pts',(-0.692438336046953,-0.0987028913474132,
1.48013502083327));
#37839=CARTESIAN_POINT('Ctrl Pts',(-0.671112380384256,-0.197459452965884,
1.48353872420306));
#37840=CARTESIAN_POINT('Ctrl Pts',(-0.630169276665042,-0.287273209389724,
1.48694242757285));
#37841=CARTESIAN_POINT('Ctrl Pts',(-0.582360588475253,-0.392147473575174,
1.49091688427776));
#37842=CARTESIAN_POINT('Ctrl Pts',(-0.507804104334794,-0.484828307406556,
1.49489134098267));
#37843=CARTESIAN_POINT('Ctrl Pts',(-0.415607008579433,-0.553994610538978,
1.49886579768759));
#37844=CARTESIAN_POINT('Ctrl Pts',(-0.323409912824072,-0.623160913671399,
1.5028402543925));
#37845=CARTESIAN_POINT('Ctrl Pts',(-0.213572205453808,-0.668812686104861,
1.50681471109742));
#37846=CARTESIAN_POINT('Ctrl Pts',(-0.0995107241808008,-0.685373496611229,
1.51078916780233));
#37847=CARTESIAN_POINT('Ctrl Pts',(0.0145507570922064,-0.701934307117598,
1.51476362450724));
#37848=CARTESIAN_POINT('Ctrl Pts',(0.132836012267957,-0.689404155696873,
1.51873808121216));
#37849=CARTESIAN_POINT('Ctrl Pts',(0.240896323230717,-0.649313618787479,
1.52271253791707));
#37850=CARTESIAN_POINT('Ctrl Pts',(0.348956634193476,-0.609223081878085,
1.52668699462198));
#37851=CARTESIAN_POINT('Ctrl Pts',(0.446792000943244,-0.54157215948002,
1.5306614513269));
#37852=CARTESIAN_POINT('Ctrl Pts',(0.522451689348894,-0.454624511413833,
1.53463590803181));
#37853=CARTESIAN_POINT('Ctrl Pts',(0.598111377754543,-0.367676863347648,
1.53861036473672));
#37854=CARTESIAN_POINT('Ctrl Pts',(0.651595387816075,-0.26143248961334,
1.54258482144163));
#37855=CARTESIAN_POINT('Ctrl Pts',(0.676370568943166,-0.148869296885099,
1.54655927814655));
#37856=CARTESIAN_POINT('Ctrl Pts',(0.701145750070258,-0.0363061041568547,
1.55053373485146));
#37857=CARTESIAN_POINT('Ctrl Pts',(0.697212102262908,0.0825759075653193,
1.55450819155638));
#37858=CARTESIAN_POINT('Ctrl Pts',(0.665050126386205,0.193255125390099,
1.55848264826129));
#37859=CARTESIAN_POINT('Ctrl Pts',(0.632888150509503,0.303934343214878,
1.5624571049662));
#37860=CARTESIAN_POINT('Ctrl Pts',(0.572497846563448,0.406410767142259,
1.56643156167112));
#37861=CARTESIAN_POINT('Ctrl Pts',(0.491255979126122,0.488166751240568,
1.57040601837603));
#37862=CARTESIAN_POINT('Ctrl Pts',(0.410014111688796,0.569922735338878,
1.57438047508094));
#37863=CARTESIAN_POINT('Ctrl Pts',(0.307920680760198,0.630958279608118,
1.57835493178586));
#37864=CARTESIAN_POINT('Ctrl Pts',(0.197446549249608,0.663817802097849,
1.58232938849077));
#37865=CARTESIAN_POINT('Ctrl Pts',(0.0869724177390183,0.696677324587579,
1.58630384519568));
#37866=CARTESIAN_POINT('Ctrl Pts',(-0.0318824143535636,0.701360825297801,
1.5902783019006));
#37867=CARTESIAN_POINT('Ctrl Pts',(-0.14459965419217,0.67729620838021,1.59425275860551));
#37868=CARTESIAN_POINT('Ctrl Pts',(-0.257316894030777,0.653231591462618,
1.59822721531042));
#37869=CARTESIAN_POINT('Ctrl Pts',(-0.363896541615409,0.600418856917212,
1.60220167201534));
#37870=CARTESIAN_POINT('Ctrl Pts',(-0.451319736154936,0.52530915672931,
1.60617612872025));
#37871=CARTESIAN_POINT('Ctrl Pts',(-0.538742930694463,0.450199456541409,
1.61015058542516));
#37872=CARTESIAN_POINT('Ctrl Pts',(-0.607009672188885,0.35279279071101,
1.61412504213008));
#37873=CARTESIAN_POINT('Ctrl Pts',(-0.647781077390964,0.244987529539448,
1.61809949883499));
#37874=CARTESIAN_POINT('Ctrl Pts',(-0.677297176576543,0.16694286157434,
1.62097677171115));
#37875=CARTESIAN_POINT('Ctrl Pts',(-0.69240322209232,0.0834483851266751,
1.62385404458732));
#37876=CARTESIAN_POINT('Ctrl Pts',(-0.692483926679543,-1.76726015421153E-5,
1.62673131746348));
#37877=CARTESIAN_POINT('Origin',(0.,0.,0.422718733092612));
#37878=CARTESIAN_POINT('',(-0.606822805098715,-1.39790256400196E-5,1.69771873309261));
#37879=CARTESIAN_POINT('',(-0.606828099052645,1.21067951662501E-5,1.72728126690739));
#37880=CARTESIAN_POINT('',(-0.60685,-1.25452023855349E-14,0.422718733092612));
#37881=CARTESIAN_POINT('',(0.298621660385098,-0.528323265936631,1.7475));
#37882=CARTESIAN_POINT('Ctrl Pts',(-0.606822805098715,-1.39790256400533E-5,
1.69771873309261));
#37883=CARTESIAN_POINT('Ctrl Pts',(-0.606850144986406,-0.0325916380113017,
1.69900018527446));
#37884=CARTESIAN_POINT('Ctrl Pts',(-0.59627583269252,-0.166192123249729,
1.70425609416123));
#37885=CARTESIAN_POINT('Ctrl Pts',(-0.499613590710631,-0.388133987750645,
1.71348645975291));
#37886=CARTESIAN_POINT('Ctrl Pts',(-0.252692420892918,-0.580008494847657,
1.72540982986765));
#37887=CARTESIAN_POINT('Ctrl Pts',(0.0408047583705589,-0.62771684740776,
1.73674767661668));
#37888=CARTESIAN_POINT('Ctrl Pts',(0.223596410438565,-0.57063337113422,
1.7441110666608));
#37889=CARTESIAN_POINT('Ctrl Pts',(0.298621660385098,-0.528323265936631,
1.7475));
#37890=CARTESIAN_POINT('',(-0.401912945313201,-0.454678905261359,1.7475));
#37891=CARTESIAN_POINT('Origin',(0.,0.,1.7475));
#37892=CARTESIAN_POINT('Ctrl Pts',(-0.606828099052645,1.21067951662536E-5,
1.72728126690739));
#37893=CARTESIAN_POINT('Ctrl Pts',(-0.606765611668105,-0.0702881660046895,
1.73004638790001));
#37894=CARTESIAN_POINT('Ctrl Pts',(-0.577018035169713,-0.241685874256128,
1.73678596559755));
#37895=CARTESIAN_POINT('Ctrl Pts',(-0.477608641113037,-0.38776777370368,
1.74352554329509));
#37896=CARTESIAN_POINT('Ctrl Pts',(-0.401912945313201,-0.454678905261359,
1.7475));
#37897=CARTESIAN_POINT('Origin',(0.,0.,0.422718733092612));
#37898=CARTESIAN_POINT('',(-0.60688975719765,9.647971041945E-6,1.54771873309261));
#37899=CARTESIAN_POINT('',(-0.606835914664954,-1.54868133572239E-5,1.57728126690739));
#37900=CARTESIAN_POINT('',(-0.60685,-1.25452023855349E-14,0.422718733092612));
#37901=CARTESIAN_POINT('Ctrl Pts',(-0.60688975719765,9.64797104193935E-6,
1.54771873309261));
#37902=CARTESIAN_POINT('Ctrl Pts',(-0.60682065745532,-0.0911763859235254,
1.5513067048155));
#37903=CARTESIAN_POINT('Ctrl Pts',(-0.562903026131426,-0.28343503097576,
1.55886913324331));
#37904=CARTESIAN_POINT('Ctrl Pts',(-0.367843073028309,-0.514736421708243,
1.57040601837603));
#37905=CARTESIAN_POINT('Ctrl Pts',(-0.0763834766033089,-0.628034772279233,
1.58232938849077));
#37906=CARTESIAN_POINT('Ctrl Pts',(0.233736828044883,-0.5879023770064,1.59425275860551));
#37907=CARTESIAN_POINT('Ctrl Pts',(0.486754537336504,-0.404143701789823,
1.60617612872025));
#37908=CARTESIAN_POINT('Ctrl Pts',(0.620856679132942,-0.121651525197101,
1.61809949883499));
#37909=CARTESIAN_POINT('Ctrl Pts',(0.603281706262845,0.190560468004963,
1.63002286894973));
#37910=CARTESIAN_POINT('Ctrl Pts',(0.43832323427345,0.456217996120286,1.64194623906447));
#37911=CARTESIAN_POINT('Ctrl Pts',(0.166281107894437,0.610420087199418,
1.65386960917921));
#37912=CARTESIAN_POINT('Ctrl Pts',(-0.146383988411153,0.615494826402396,
1.66579297929395));
#37913=CARTESIAN_POINT('Ctrl Pts',(-0.423287034230507,0.470202220700963,
1.67771634940869));
#37914=CARTESIAN_POINT('Ctrl Pts',(-0.578133869070706,0.23799899265915,
1.68835826734158));
#37915=CARTESIAN_POINT('Ctrl Pts',(-0.606765349625733,0.0684488042459758,
1.69502572856955));
#37916=CARTESIAN_POINT('Ctrl Pts',(-0.606822805098715,-1.39790256400533E-5,
1.69771873309261));
#37917=CARTESIAN_POINT('Ctrl Pts',(-0.606835914664954,-1.54868133571684E-5,
1.57728126690739));
#37918=CARTESIAN_POINT('Ctrl Pts',(-0.606862883249031,-0.0279068554810485,
1.57837845073614));
#37919=CARTESIAN_POINT('Ctrl Pts',(-0.598137372064807,-0.156815636589154,
1.5834500912698));
#37920=CARTESIAN_POINT('Ctrl Pts',(-0.508466394890466,-0.376462544933448,
1.59249618850838));
#37921=CARTESIAN_POINT('Ctrl Pts',(-0.266054119846729,-0.574001132528779,
1.60441955862312));
#37922=CARTESIAN_POINT('Ctrl Pts',(0.041355953716283,-0.631309625261172,
1.61634292873786));
#37923=CARTESIAN_POINT('Ctrl Pts',(0.338662659096756,-0.534387172794291,
1.6282662988526));
#37924=CARTESIAN_POINT('Ctrl Pts',(0.553233053245814,-0.306912647437654,
1.64018966896734));
#37925=CARTESIAN_POINT('Ctrl Pts',(0.63264703504302,-0.004457885988231,
1.65211303908208));
#37926=CARTESIAN_POINT('Ctrl Pts',(0.557503379173826,0.299084810277989,
1.66403640919682));
#37927=CARTESIAN_POINT('Ctrl Pts',(0.346160212094308,0.529562476556959,
1.67595977931156));
#37928=CARTESIAN_POINT('Ctrl Pts',(0.0502486745876001,0.630661949020613,
1.6878831494263));
#37929=CARTESIAN_POINT('Ctrl Pts',(-0.257937943046404,0.577697854759531,
1.69980651954104));
#37930=CARTESIAN_POINT('Ctrl Pts',(-0.503111198644335,0.383582524720304,
1.71172988965578));
#37931=CARTESIAN_POINT('Ctrl Pts',(-0.597016914950347,0.162533434793575,
1.7208881387779));
#37932=CARTESIAN_POINT('Ctrl Pts',(-0.606855428137301,0.0307581865173095,
1.7260719311951));
#37933=CARTESIAN_POINT('Ctrl Pts',(-0.606828099052645,1.21067951662536E-5,
1.72728126690739));
#37934=CARTESIAN_POINT('Origin',(0.,0.,0.422718733092612));
#37935=CARTESIAN_POINT('',(-0.606798126054683,-1.59915840535429E-6,1.39771873309261));
#37936=CARTESIAN_POINT('',(-0.606877435462865,1.29655716943344E-5,1.42728126690739));
#37937=CARTESIAN_POINT('',(-0.60685,-1.25452023855349E-14,0.422718733092612));
#37938=CARTESIAN_POINT('Ctrl Pts',(-0.606798126054683,-1.59915840541175E-6,
1.39771873309261));
#37939=CARTESIAN_POINT('Ctrl Pts',(-0.606802594249528,-0.0488192602443514,
1.39963876765163));
#37940=CARTESIAN_POINT('Ctrl Pts',(-0.588931640835428,-0.198685886988713,
1.40553325891556));
#37941=CARTESIAN_POINT('Ctrl Pts',(-0.466892707499535,-0.426934784279433,
1.41540220688441));
#37942=CARTESIAN_POINT('Ctrl Pts',(-0.205385625641773,-0.598396904339966,
1.42732557699915));
#37943=CARTESIAN_POINT('Ctrl Pts',(0.106297769497149,-0.623668898169518,
1.43924894711389));
#37944=CARTESIAN_POINT('Ctrl Pts',(0.392012306461527,-0.496576743239674,
1.45117231722863));
#37945=CARTESIAN_POINT('Ctrl Pts',(0.581957082335726,-0.248169427334259,
1.46309568734337));
#37946=CARTESIAN_POINT('Ctrl Pts',(0.629728028915714,0.0608664106211582,
1.47501905745811));
#37947=CARTESIAN_POINT('Ctrl Pts',(0.523654563249111,0.355032405185257,
1.48694242757285));
#37948=CARTESIAN_POINT('Ctrl Pts',(0.289650745423433,0.562462937465252,
1.49886579768759));
#37949=CARTESIAN_POINT('Ctrl Pts',(-0.0151156026373754,0.632482117450919,
1.51078916780233));
#37950=CARTESIAN_POINT('Ctrl Pts',(-0.316189164454242,0.547984053267855,
1.52271253791707));
#37951=CARTESIAN_POINT('Ctrl Pts',(-0.540016782097706,0.329611870817301,
1.53463590803181));
#37952=CARTESIAN_POINT('Ctrl Pts',(-0.604262251146843,0.120658502190452,
1.54297130642366));
#37953=CARTESIAN_POINT('Ctrl Pts',(-0.606897200403655,0.00983191954734194,
1.54733224811059));
#37954=CARTESIAN_POINT('Ctrl Pts',(-0.60688975719765,9.64797104193935E-6,
1.54771873309261));
#37955=CARTESIAN_POINT('Ctrl Pts',(-0.606877435462865,1.29655716943379E-5,
1.42728126690739));
#37956=CARTESIAN_POINT('Ctrl Pts',(-0.606795962787138,-0.0864950896955681,
1.43068497027718));
#37957=CARTESIAN_POINT('Ctrl Pts',(-0.566285570456084,-0.274091234023481,
1.43806313035188));
#37958=CARTESIAN_POINT('Ctrl Pts',(-0.379662553523367,-0.506081476332481,
1.4494157471315));
#37959=CARTESIAN_POINT('Ctrl Pts',(-0.0909043756851951,-0.626097843558096,
1.46133911724624));
#37960=CARTESIAN_POINT('Ctrl Pts',(0.220062008878289,-0.593156663530657,
1.47326248736098));
#37961=CARTESIAN_POINT('Ctrl Pts',(0.477266596511919,-0.415305563499184,
1.48518585747572));
#37962=CARTESIAN_POINT('Ctrl Pts',(0.617873548883792,-0.135994091149731,
1.49710922759046));
#37963=CARTESIAN_POINT('Ctrl Pts',(0.607532173409899,0.176541138367681,
1.5090325977052));
#37964=CARTESIAN_POINT('Ctrl Pts',(0.44876889853771,0.445946847509907,1.52095596781994));
#37965=CARTESIAN_POINT('Ctrl Pts',(0.180370060014882,0.606406428909711,
1.53287933793468));
#37966=CARTESIAN_POINT('Ctrl Pts',(-0.132093715531906,0.618719132473601,
1.54480270804942));
#37967=CARTESIAN_POINT('Ctrl Pts',(-0.412286607098983,0.479876931929719,
1.55672607816416));
#37968=CARTESIAN_POINT('Ctrl Pts',(-0.575241902336924,0.247363534614087,
1.56755226445015));
#37969=CARTESIAN_POINT('Ctrl Pts',(-0.606765191807545,0.0731272960492705,
1.57440399403123));
#37970=CARTESIAN_POINT('Ctrl Pts',(-0.606835914664954,-1.54868133571684E-5,
1.57728126690739));
#37971=CARTESIAN_POINT('Origin',(0.,0.,0.422718733092612));
#37972=CARTESIAN_POINT('',(-0.606896670952539,-6.59829139776882E-6,1.24771873309261));
#37973=CARTESIAN_POINT('',(-0.606801243923172,-5.85749501685884E-6,1.27728126690739));
#37974=CARTESIAN_POINT('',(-0.60685,-1.25452023855349E-14,0.422718733092612));
#37975=CARTESIAN_POINT('Ctrl Pts',(-0.606896670952539,-6.59829139778353E-6,
1.24771873309261));
#37976=CARTESIAN_POINT('Ctrl Pts',(-0.606900224819954,-0.00641328249130264,
1.24797083048776));
#37977=CARTESIAN_POINT('Ctrl Pts',(-0.605234866882428,-0.113823082303296,
1.25219738458781));
#37978=CARTESIAN_POINT('Ctrl Pts',(-0.545505882342923,-0.320445693797292,
1.26039839539279));
#37979=CARTESIAN_POINT('Ctrl Pts',(-0.325397796916506,-0.542566478973631,
1.27232176550753));
#37980=CARTESIAN_POINT('Ctrl Pts',(-0.0257940712861588,-0.632136675277145,
1.28424513562227));
#37981=CARTESIAN_POINT('Ctrl Pts',(0.280111221932506,-0.567274019933433,
1.29616850573701));
#37982=CARTESIAN_POINT('Ctrl Pts',(0.517584518601595,-0.363824650687545,
1.30809187585175));
#37983=CARTESIAN_POINT('Ctrl Pts',(0.628610392897891,-0.0714918476801203,
1.32001524596649));
#37984=CARTESIAN_POINT('Ctrl Pts',(0.586064896718421,0.238306624285571,
1.33193861608123));
#37985=CARTESIAN_POINT('Ctrl Pts',(0.4003420200921,0.489886086036881,1.34386198619597));
#37986=CARTESIAN_POINT('Ctrl Pts',(0.116814408801508,0.621784934073119,
1.35578535631071));
#37987=CARTESIAN_POINT('Ctrl Pts',(-0.195251306621063,0.601779891327988,
1.36770872642545));
#37988=CARTESIAN_POINT('Ctrl Pts',(-0.459616552748575,0.434758248666402,
1.37963209654019));
#37989=CARTESIAN_POINT('Ctrl Pts',(-0.587206566371662,0.205523141855759,
1.38963543209591));
#37990=CARTESIAN_POINT('Ctrl Pts',(-0.606793345120716,0.052232921087437,
1.39566431094672));
#37991=CARTESIAN_POINT('Ctrl Pts',(-0.606798126054683,-1.59915840541175E-6,
1.39771873309261));
#37992=CARTESIAN_POINT('Ctrl Pts',(-0.606801243923172,-5.85749501688312E-6,
1.27728126690739));
#37993=CARTESIAN_POINT('Ctrl Pts',(-0.60681613156811,-0.0441377730285598,
1.2790170331133));
#37994=CARTESIAN_POINT('Ctrl Pts',(-0.591194722324054,-0.189310005818757,
1.28472725602413));
#37995=CARTESIAN_POINT('Ctrl Pts',(-0.476652695565553,-0.416010003536527,
1.29441193563987));
#37996=CARTESIAN_POINT('Ctrl Pts',(-0.219185713483245,-0.593481034437674,
1.30633530575462));
#37997=CARTESIAN_POINT('Ctrl Pts',(0.0918289839862619,-0.625962900603877,
1.31825867586936));
#37998=CARTESIAN_POINT('Ctrl Pts',(0.380409590197501,-0.505520186459593,
1.3301820459841));
#37999=CARTESIAN_POINT('Ctrl Pts',(0.576055013076121,-0.26157740181873,
1.34210541609884));
#38000=CARTESIAN_POINT('Ctrl Pts',(0.630968499564522,0.0462695125289182,
1.35402878621358));
#38001=CARTESIAN_POINT('Ctrl Pts',(0.531734523173002,0.34281264868491,1.36595215632832));
#38002=CARTESIAN_POINT('Ctrl Pts',(0.302596236614874,0.555605645056675,
1.37787552644306));
#38003=CARTESIAN_POINT('Ctrl Pts',(-0.000467201806429895,0.632662545876497,
1.3897988965578));
#38004=CARTESIAN_POINT('Ctrl Pts',(-0.303416501450367,0.555158123312486,
1.40172226667254));
#38005=CARTESIAN_POINT('Ctrl Pts',(-0.532240256115767,0.3420269360772,1.41364563678728));
#38006=CARTESIAN_POINT('Ctrl Pts',(-0.6028333913918,0.130031956601212,1.42216530353223));
#38007=CARTESIAN_POINT('Ctrl Pts',(-0.606891097288336,0.0145191535953422,
1.42671051357226));
#38008=CARTESIAN_POINT('Ctrl Pts',(-0.606877435462865,1.29655716943379E-5,
1.42728126690739));
#38009=CARTESIAN_POINT('Origin',(0.,0.,0.422718733092612));
#38010=CARTESIAN_POINT('',(-0.606814611697072,1.20472578674858E-5,1.09771873309261));
#38011=CARTESIAN_POINT('',(-0.606902028636254,-1.83691493421678E-6,1.12728126690739));
#38012=CARTESIAN_POINT('',(-0.60685,-1.25452023855349E-14,0.422718733092612));
#38013=CARTESIAN_POINT('Ctrl Pts',(-0.606814611697072,1.20472578674785E-5,
1.09771873309261));
#38014=CARTESIAN_POINT('Ctrl Pts',(-0.606768181291156,-0.0650367723393511,
1.1002773500288));
#38015=CARTESIAN_POINT('Ctrl Pts',(-0.580164840953881,-0.231166986996602,
1.10681042366989));
#38016=CARTESIAN_POINT('Ctrl Pts',(-0.431166912267969,-0.462987261281848,
1.1173179540159));
#38017=CARTESIAN_POINT('Ctrl Pts',(-0.156756874309222,-0.612935064016377,
1.12924132413064));
#38018=CARTESIAN_POINT('Ctrl Pts',(0.155949329750418,-0.613141025290557,
1.14116469424539));
#38019=CARTESIAN_POINT('Ctrl Pts',(0.4305566532234,-0.463554828158465,1.15308806436012));
#38020=CARTESIAN_POINT('Ctrl Pts',(0.59997771816483,-0.200720821166321,
1.16501143447486));
#38021=CARTESIAN_POINT('Ctrl Pts',(0.622822459401631,0.111149873634038,
1.17693480458961));
#38022=CARTESIAN_POINT('Ctrl Pts',(0.493509839363413,0.395866326927988,
1.18885817470434));
#38023=CARTESIAN_POINT('Ctrl Pts',(0.243631311999152,0.583871470580239,
1.20078154481908));
#38024=CARTESIAN_POINT('Ctrl Pts',(-0.0657670624710998,0.629235094251649,
1.21270491493383));
#38025=CARTESIAN_POINT('Ctrl Pts',(-0.359098349871265,0.520874731066591,
1.22462828504856));
#38026=CARTESIAN_POINT('Ctrl Pts',(-0.560353771743364,0.290244704085391,
1.23629955776816));
#38027=CARTESIAN_POINT('Ctrl Pts',(-0.60684419610863,0.0945916841009262,
1.24399637378284));
#38028=CARTESIAN_POINT('Ctrl Pts',(-0.606896670952539,-6.59829139778353E-6,
1.24771873309261));
#38029=CARTESIAN_POINT('Ctrl Pts',(-0.606902028636254,-1.83691493418382E-6,
1.12728126690739));
#38030=CARTESIAN_POINT('Ctrl Pts',(-0.60690232638052,-0.00172556794049109,
1.12734909594943));
#38031=CARTESIAN_POINT('Ctrl Pts',(-0.606473854563749,-0.104451525220278,
1.13139138169638));
#38032=CARTESIAN_POINT('Ctrl Pts',(-0.552779171463751,-0.307729268722068,
1.13940812414825));
#38033=CARTESIAN_POINT('Ctrl Pts',(-0.337873026968778,-0.534886841191037,
1.15133149426299));
#38034=CARTESIAN_POINT('Ctrl Pts',(-0.0404235068239226,-0.631369982916851,
1.16325486437773));
#38035=CARTESIAN_POINT('Ctrl Pts',(0.26690159510024,-0.573607578197252,
1.17517823449247));
#38036=CARTESIAN_POINT('Ctrl Pts',(0.509021851217201,-0.375711152636948,
1.18710160460721));
#38037=CARTESIAN_POINT('Ctrl Pts',(0.626786569823609,-0.0860273858787084,
1.19902497472195));
#38038=CARTESIAN_POINT('Ctrl Pts',(0.591425483303132,0.224673124632266,
1.21094834483669));
#38039=CARTESIAN_POINT('Ctrl Pts',(0.411577409244242,0.480485329049876,
1.22287171495143));
#38040=CARTESIAN_POINT('Ctrl Pts',(0.131179761858824,0.618913552373053,
1.23479508506618));
#38041=CARTESIAN_POINT('Ctrl Pts',(-0.181265487721769,0.606139371921474,
1.24671845518091));
#38042=CARTESIAN_POINT('Ctrl Pts',(-0.449427044757826,0.445283557604159,
1.25864182529566));
#38043=CARTESIAN_POINT('Ctrl Pts',(-0.584737949218254,0.214896975434926,
1.26882942920448));
#38044=CARTESIAN_POINT('Ctrl Pts',(-0.606782042702892,0.0569129255016839,
1.27504257640839));
#38045=CARTESIAN_POINT('Ctrl Pts',(-0.606801243923172,-5.85749501688312E-6,
1.27728126690739));
#38046=CARTESIAN_POINT('Origin',(0.,0.,0.422718733092612));
#38047=CARTESIAN_POINT('',(-0.606852195439347,-1.57862025725476E-5,0.947718733092612));
#38048=CARTESIAN_POINT('',(-0.60680575058562,8.7320520037043E-6,0.977281266907388));
#38049=CARTESIAN_POINT('',(-0.60685,-1.25452023855349E-14,0.422718733092612));
#38050=CARTESIAN_POINT('Ctrl Pts',(-0.606852195439347,-1.5786202572584E-5,
0.947718733092612));
#38051=CARTESIAN_POINT('Ctrl Pts',(-0.606875617872986,-0.0226558951432442,
0.948609412864922));
#38052=CARTESIAN_POINT('Ctrl Pts',(-0.600088688538456,-0.146308396998802,
0.953474549342146));
#38053=CARTESIAN_POINT('Ctrl Pts',(-0.518063329334561,-0.363142530047957,
0.962314142524282));
#38054=CARTESIAN_POINT('Ctrl Pts',(-0.280858238968939,-0.566904542191545,
0.974237512639023));
#38055=CARTESIAN_POINT('Ctrl Pts',(0.0249613464089441,-0.632170104895623,
0.986160882753763));
#38056=CARTESIAN_POINT('Ctrl Pts',(0.324682801338475,-0.542994649017271,
0.998084252868503));
#38057=CARTESIAN_POINT('Ctrl Pts',(0.545083291589825,-0.321164001053741,
1.01000762298324));
#38058=CARTESIAN_POINT('Ctrl Pts',(0.632318328233213,-0.0208720416904643,
1.02193099309798));
#38059=CARTESIAN_POINT('Ctrl Pts',(0.565076134877199,0.284519018936116,
1.03385436321272));
#38060=CARTESIAN_POINT('Ctrl Pts',(0.35978417741182,0.520401245221327,1.04577773332746));
#38061=CARTESIAN_POINT('Ctrl Pts',(0.0665958857068623,0.62914791452485,
1.0577011034422));
#38062=CARTESIAN_POINT('Ctrl Pts',(-0.242861977025874,0.584191895235632,
1.06962447355694));
#38063=CARTESIAN_POINT('Ctrl Pts',(-0.492987943452569,0.396516075278645,
1.08154784367169));
#38064=CARTESIAN_POINT('Ctrl Pts',(-0.59484605707748,0.173030452641354,
1.09091259685024));
#38065=CARTESIAN_POINT('Ctrl Pts',(-0.606840304490021,0.0360075510756424,
1.09630289332388));
#38066=CARTESIAN_POINT('Ctrl Pts',(-0.606814611697072,1.20472578674785E-5,
1.09771873309261));
#38067=CARTESIAN_POINT('Ctrl Pts',(-0.60680575058562,8.73205200368002E-6,
0.977281266907388));
#38068=CARTESIAN_POINT('Ctrl Pts',(-0.606775110747621,-0.0603578794789066,
0.97965561549047));
#38069=CARTESIAN_POINT('Ctrl Pts',(-0.582843583723735,-0.22179680306636,
0.986004420778464));
#38070=CARTESIAN_POINT('Ctrl Pts',(-0.441771228592792,-0.452880002671609,
0.996327682771373));
#38071=CARTESIAN_POINT('Ctrl Pts',(-0.170906611750865,-0.6091412359152,
1.00825105288611));
#38072=CARTESIAN_POINT('Ctrl Pts',(0.141710993725228,-0.616587471077492,
1.02017442300085));
#38073=CARTESIAN_POINT('Ctrl Pts',(0.419708186042773,-0.473399570976854,
1.03209779311559));
#38074=CARTESIAN_POINT('Ctrl Pts',(0.595169432313768,-0.214558761349135,
1.04402116323033));
#38075=CARTESIAN_POINT('Ctrl Pts',(0.625229033275726,0.0966993856312912,
1.05594453334507));
#38076=CARTESIAN_POINT('Ctrl Pts',(0.502543339876973,0.384333587886446,
1.06786790345981));
#38077=CARTESIAN_POINT('Ctrl Pts',(0.257084828369703,0.578073962615934,
1.07979127357455));
#38078=CARTESIAN_POINT('Ctrl Pts',(-0.0511802639184789,0.630589165636079,
1.09171464368929));
#38079=CARTESIAN_POINT('Ctrl Pts',(-0.346941866986512,0.529049578172294,
1.10363801380403));
#38080=CARTESIAN_POINT('Ctrl Pts',(-0.556744209089362,0.29957451493303,
1.11549355487673));
#38081=CARTESIAN_POINT('Ctrl Pts',(-0.606884879993859,0.0992768069387203,
1.12337463924452));
#38082=CARTESIAN_POINT('Ctrl Pts',(-0.606902028636254,-1.83691493418382E-6,
1.12728126690739));
#38083=CARTESIAN_POINT('Origin',(0.,0.,0.422718733092612));
#38084=CARTESIAN_POINT('',(-0.606861373480359,1.53279143725419E-5,0.797718733092612));
#38085=CARTESIAN_POINT('',(-0.606867041669442,-1.46440865503583E-5,0.827281266907388));
#38086=CARTESIAN_POINT('',(-0.60685,-1.25452023855349E-14,0.422718733092612));
#38087=CARTESIAN_POINT('Ctrl Pts',(-0.606861373480359,1.53279143725385E-5,
0.797718733092612));
#38088=CARTESIAN_POINT('Ctrl Pts',(-0.606777537923217,-0.0812504538222047,
0.800915932405962));
#38089=CARTESIAN_POINT('Ctrl Pts',(-0.569922761574246,-0.263612138122336,
0.808087588424225));
#38090=CARTESIAN_POINT('Ctrl Pts',(-0.392666097338528,-0.496059852941866,
0.819233701147401));
#38091=CARTESIAN_POINT('Ctrl Pts',(-0.107119225715726,-0.623528367336511,
0.831157071262142));
#38092=CARTESIAN_POINT('Ctrl Pts',(0.204597189954239,-0.59866691871355,
0.843080441376881));
#38093=CARTESIAN_POINT('Ctrl Pts',(0.466329908650049,-0.427549452094589,
0.855003811491622));
#38094=CARTESIAN_POINT('Ctrl Pts',(0.614136857577049,-0.151980358083104,
0.866927181606362));
#38095=CARTESIAN_POINT('Ctrl Pts',(0.611908363121538,0.160717966477571,
0.878850551721102));
#38096=CARTESIAN_POINT('Ctrl Pts',(0.460188853366613,0.434152427784503,
0.890773921835841));
#38097=CARTESIAN_POINT('Ctrl Pts',(0.1960438512529,0.601522167555102,0.902697291950583));
#38098=CARTESIAN_POINT('Ctrl Pts',(-0.115995241116418,0.621938272442033,
0.914620662065322));
#38099=CARTESIAN_POINT('Ctrl Pts',(-0.399696354445721,0.490413024348575,
0.926544032180063));
#38100=CARTESIAN_POINT('Ctrl Pts',(-0.571852165804536,0.257853209547959,
0.937576722522492));
#38101=CARTESIAN_POINT('Ctrl Pts',(-0.606771100569104,0.0783704620017294,
0.944634956160009));
#38102=CARTESIAN_POINT('Ctrl Pts',(-0.606852195439347,-1.5786202572584E-5,
0.947718733092612));
#38103=CARTESIAN_POINT('Ctrl Pts',(-0.606867041669442,-1.46440865504086E-5,
0.827281266907388));
#38104=CARTESIAN_POINT('Ctrl Pts',(-0.606885242107981,-0.0179695869580834,
0.827987678326596));
#38105=CARTESIAN_POINT('Ctrl Pts',(-0.601710640579271,-0.13693331365204,
0.832668546450717));
#38106=CARTESIAN_POINT('Ctrl Pts',(-0.526332568352355,-0.351050058657002,
0.841323871279751));
#38107=CARTESIAN_POINT('Ctrl Pts',(-0.293908927059336,-0.560249638256679,
0.85324724139449));
#38108=CARTESIAN_POINT('Ctrl Pts',(0.0103175303644349,-0.632578583371251,
0.865170611509231));
#38109=CARTESIAN_POINT('Ctrl Pts',(0.31202338494245,-0.550366716242752,
0.877093981623972));
#38110=CARTESIAN_POINT('Ctrl Pts',(0.537501007448335,-0.333698639877864,
0.889017351738711));
#38111=CARTESIAN_POINT('Ctrl Pts',(0.631665550747977,-0.0355070026353613,
0.900940721853452));
#38112=CARTESIAN_POINT('Ctrl Pts',(0.571512339483762,0.271359099787061,
0.912864091968191));
#38113=CARTESIAN_POINT('Ctrl Pts',(0.371736980381227,0.51193137495119,0.924787462082931));
#38114=CARTESIAN_POINT('Ctrl Pts',(0.0811451820615032,0.627437307350318,
0.936710832197672));
#38115=CARTESIAN_POINT('Ctrl Pts',(-0.229270623235126,0.589658457546506,
0.948634202312412));
#38116=CARTESIAN_POINT('Ctrl Pts',(-0.483674939990074,0.407824309791941,
0.960557572427152));
#38117=CARTESIAN_POINT('Ctrl Pts',(-0.592785805966434,0.182407101947706,
0.970106593958811));
#38118=CARTESIAN_POINT('Ctrl Pts',(-0.606826399219094,0.0406906715474857,
0.975681158785556));
#38119=CARTESIAN_POINT('Ctrl Pts',(-0.60680575058562,8.73205200368002E-6,
0.977281266907388));
#38120=CARTESIAN_POINT('Origin',(1.1271216279739E-16,-2.42910627858037E-17,
1.7475));
#38121=CARTESIAN_POINT('',(0.365377360036753,0.588264935868672,1.7475));
#38122=CARTESIAN_POINT('Ctrl Pts',(0.298621660385102,-0.528323265936629,
1.7475));
#38123=CARTESIAN_POINT('Ctrl Pts',(0.312129560427946,-0.521873925222218,
1.7475));
#38124=CARTESIAN_POINT('Ctrl Pts',(0.325379783927112,-0.514929522576798,
1.7475));
#38125=CARTESIAN_POINT('Ctrl Pts',(0.338343379574887,-0.50750179203716,
1.7475));
#38126=CARTESIAN_POINT('Ctrl Pts',(0.36077543119364,-0.494648935514754,
1.7475));
#38127=CARTESIAN_POINT('Ctrl Pts',(0.382349984001486,-0.480350324006014,
1.7475));
#38128=CARTESIAN_POINT('Ctrl Pts',(0.402968596112581,-0.464732386935322,
1.7475));
#38129=CARTESIAN_POINT('Ctrl Pts',(0.412005321941232,-0.457887357087701,
1.7475));
#38130=CARTESIAN_POINT('Ctrl Pts',(0.420858285551003,-0.450788564790034,
1.7475));
#38131=CARTESIAN_POINT('Ctrl Pts',(0.429518414483015,-0.4434452100822,1.7475));
#38132=CARTESIAN_POINT('Ctrl Pts',(0.43632784881018,-0.437671151518334,
1.7475));
#38133=CARTESIAN_POINT('Ctrl Pts',(0.443012226475618,-0.431750667617364,
1.7475));
#38134=CARTESIAN_POINT('Ctrl Pts',(0.449562091487209,-0.425694086415582,
1.7475));
#38135=CARTESIAN_POINT('Ctrl Pts',(0.470631367154316,-0.406211581247191,
1.7475));
#38136=CARTESIAN_POINT('Ctrl Pts',(0.490328809845417,-0.38530767574534,
1.7475));
#38137=CARTESIAN_POINT('Ctrl Pts',(0.508518158509955,-0.363142905055253,
1.7475));
#38138=CARTESIAN_POINT('Ctrl Pts',(0.516442502170421,-0.353486635150102,
1.7475));
#38139=CARTESIAN_POINT('Ctrl Pts',(0.524080348515509,-0.343590638760223,
1.7475));
#38140=CARTESIAN_POINT('Ctrl Pts',(0.531418980886992,-0.333466452816219,
1.7475));
#38141=CARTESIAN_POINT('Ctrl Pts',(0.537374715310306,-0.325250076837359,
1.7475));
#38142=CARTESIAN_POINT('Ctrl Pts',(0.543135758395536,-0.316879252360657,
1.7475));
#38143=CARTESIAN_POINT('Ctrl Pts',(0.54867910249215,-0.308385145523163,
1.7475));
#38144=CARTESIAN_POINT('Ctrl Pts',(0.55198380721638,-0.303321322223592,
1.7475));
#38145=CARTESIAN_POINT('Ctrl Pts',(0.555212267947236,-0.298212252230868,
1.7475));
#38146=CARTESIAN_POINT('Ctrl Pts',(0.558363346279548,-0.293059483804602,
1.7475));
#38147=CARTESIAN_POINT('Ctrl Pts',(0.574646861887172,-0.266432032423531,
1.7475));
#38148=CARTESIAN_POINT('Ctrl Pts',(0.588867110740308,-0.238640752575286,
1.7475));
#38149=CARTESIAN_POINT('Ctrl Pts',(0.600996416107695,-0.209953544278971,
1.7475));
#38150=CARTESIAN_POINT('Ctrl Pts',(0.60904684941943,-0.190913339560379,
1.7475));
#38151=CARTESIAN_POINT('Ctrl Pts',(0.616175424072814,-0.171477546535687,
1.7475));
#38152=CARTESIAN_POINT('Ctrl Pts',(0.62236375672442,-0.151717176539816,
1.7475));
#38153=CARTESIAN_POINT('Ctrl Pts',(0.627198272740129,-0.136279767046878,
1.7475));
#38154=CARTESIAN_POINT('Ctrl Pts',(0.631458783571978,-0.12064412869836,
1.7475));
#38155=CARTESIAN_POINT('Ctrl Pts',(0.635132620377226,-0.104842682574537,
1.7475));
#38156=CARTESIAN_POINT('Ctrl Pts',(0.636966965175414,-0.0969530287772681,
1.7475));
#38157=CARTESIAN_POINT('Ctrl Pts',(0.638655092015668,-0.0890204207899287,
1.7475));
#38158=CARTESIAN_POINT('Ctrl Pts',(0.640191602362932,-0.0810701616342577,
1.7475));
#38159=CARTESIAN_POINT('Ctrl Pts',(0.646042674165708,-0.0507953657285062,
1.7475));
#38160=CARTESIAN_POINT('Ctrl Pts',(0.649715322524794,-0.0201981047171755,
1.7475));
#38161=CARTESIAN_POINT('Ctrl Pts',(0.651168459719186,0.0104864299067928,
1.7475));
#38162=CARTESIAN_POINT('Ctrl Pts',(0.652471176970355,0.0379946877319891,
1.7475));
#38163=CARTESIAN_POINT('Ctrl Pts',(0.651989846702894,0.0655739643226442,
1.7475));
#38164=CARTESIAN_POINT('Ctrl Pts',(0.649775510912856,0.0930641486169698,
1.7475));
#38165=CARTESIAN_POINT('Ctrl Pts',(0.648444472381905,0.109588514380875,
1.7475));
#38166=CARTESIAN_POINT('Ctrl Pts',(0.646486693282225,0.126080801141174,
1.7475));
#38167=CARTESIAN_POINT('Ctrl Pts',(0.643908241891283,0.142506225480307,
1.7475));
#38168=CARTESIAN_POINT('Ctrl Pts',(0.642438854943278,0.151866612968763,
1.7475));
#38169=CARTESIAN_POINT('Ctrl Pts',(0.64076665037931,0.16121004588847,1.7475));
#38170=CARTESIAN_POINT('Ctrl Pts',(0.638898832841581,0.170500427755555,
1.7475));
#38171=CARTESIAN_POINT('Ctrl Pts',(0.63245057878856,0.202573551237074,1.7475));
#38172=CARTESIAN_POINT('Ctrl Pts',(0.623667987104589,0.234074759209373,
1.7475));
#38173=CARTESIAN_POINT('Ctrl Pts',(0.61264701184346,0.26474553850838,1.7475));
#38174=CARTESIAN_POINT('Ctrl Pts',(0.60450404702486,0.287406970085287,1.7475));
#38175=CARTESIAN_POINT('Ctrl Pts',(0.595137974178845,0.309615432087503,
1.7475));
#38176=CARTESIAN_POINT('Ctrl Pts',(0.584569321392081,0.331264976054902,
1.7475));
#38177=CARTESIAN_POINT('Ctrl Pts',(0.577683443413199,0.345370474746717,
1.7475));
#38178=CARTESIAN_POINT('Ctrl Pts',(0.570286748895561,0.359238659304976,
1.7475));
#38179=CARTESIAN_POINT('Ctrl Pts',(0.562398175902974,0.372848797290938,
1.7475));
#38180=CARTESIAN_POINT('Ctrl Pts',(0.557821697642751,0.380744585371992,
1.7475));
#38181=CARTESIAN_POINT('Ctrl Pts',(0.553079623629564,0.388553501647874,
1.7475));
#38182=CARTESIAN_POINT('Ctrl Pts',(0.548175280753752,0.396271270275225,
1.7475));
#38183=CARTESIAN_POINT('Ctrl Pts',(0.54441947391472,0.402181633585185,1.7475));
#38184=CARTESIAN_POINT('Ctrl Pts',(0.540573489524936,0.408030640947142,
1.7475));
#38185=CARTESIAN_POINT('Ctrl Pts',(0.536640687844456,0.413815061624329,
1.7475));
#38186=CARTESIAN_POINT('Ctrl Pts',(0.518064650144307,0.441136962219085,
1.7475));
#38187=CARTESIAN_POINT('Ctrl Pts',(0.497547892662459,0.467031617110893,
1.7475));
#38188=CARTESIAN_POINT('Ctrl Pts',(0.475299963702939,0.491327450504889,
1.7475));
#38189=CARTESIAN_POINT('Ctrl Pts',(0.452956133924144,0.515728012313458,
1.7475));
#38190=CARTESIAN_POINT('Ctrl Pts',(0.4288654429408,0.538516969116918,1.7475));
#38191=CARTESIAN_POINT('Ctrl Pts',(0.40319570009474,0.55949438395691,1.7475));
#38192=CARTESIAN_POINT('Ctrl Pts',(0.390944685394277,0.569505961366299,
1.7475));
#38193=CARTESIAN_POINT('Ctrl Pts',(0.378333424832096,0.579104441213069,
1.7475));
#38194=CARTESIAN_POINT('Ctrl Pts',(0.365377360036757,0.58826493586867,1.7475));
#38195=CARTESIAN_POINT('',(-0.6925,-8.48067908409542E-17,1.7475));
#38196=CARTESIAN_POINT('Origin',(0.,0.,1.7475));
#38197=CARTESIAN_POINT('',(-0.235097938825072,0.6513885053826,1.7475));
#38198=CARTESIAN_POINT('Origin',(0.,0.,1.7475));
#38199=CARTESIAN_POINT('Ctrl Pts',(-0.235110047033021,0.651400850437653,
1.7475));
#38200=CARTESIAN_POINT('Ctrl Pts',(-0.250726404295242,0.644704975861436,
1.7475));
#38201=CARTESIAN_POINT('Ctrl Pts',(-0.266073638896426,0.63743919485856,
1.7475));
#38202=CARTESIAN_POINT('Ctrl Pts',(-0.281117933505346,0.629609469190081,
1.7475));
#38203=CARTESIAN_POINT('Ctrl Pts',(-0.306227709788298,0.616541215409952,
1.7475));
#38204=CARTESIAN_POINT('Ctrl Pts',(-0.330494626537405,0.601902955535088,
1.7475));
#38205=CARTESIAN_POINT('Ctrl Pts',(-0.353792461978798,0.585802237765094,
1.7475));
#38206=CARTESIAN_POINT('Ctrl Pts',(-0.363257657218618,0.579261010466207,
1.7475));
#38207=CARTESIAN_POINT('Ctrl Pts',(-0.372562694887073,0.572478166005196,
1.7475));
#38208=CARTESIAN_POINT('Ctrl Pts',(-0.381698167526852,0.565460062323596,
1.7475));
#38209=CARTESIAN_POINT('Ctrl Pts',(-0.388587317293776,0.560167641312798,
1.7475));
#38210=CARTESIAN_POINT('Ctrl Pts',(-0.395379904167447,0.554741287066626,
1.7475));
#38211=CARTESIAN_POINT('Ctrl Pts',(-0.402060898620473,0.549193220426858,
1.7475));
#38212=CARTESIAN_POINT('Ctrl Pts',(-0.427000921363888,0.528482395241975,
1.7475));
#38213=CARTESIAN_POINT('Ctrl Pts',(-0.450429447471031,0.506047454222527,
1.7475));
#38214=CARTESIAN_POINT('Ctrl Pts',(-0.472148997050359,0.482046003595282,
1.7475));
#38215=CARTESIAN_POINT('Ctrl Pts',(-0.485933688015498,0.466813064329979,
1.7475));
#38216=CARTESIAN_POINT('Ctrl Pts',(-0.499029320708669,0.450948438789647,
1.7475));
#38217=CARTESIAN_POINT('Ctrl Pts',(-0.511376451188905,0.434487136701648,
1.7475));
#38218=CARTESIAN_POINT('Ctrl Pts',(-0.515784428166145,0.42861038333491,
1.7475));
#38219=CARTESIAN_POINT('Ctrl Pts',(-0.520091038783305,0.422665405887042,
1.7475));
#38220=CARTESIAN_POINT('Ctrl Pts',(-0.524293998238925,0.416654482991514,
1.7475));
#38221=CARTESIAN_POINT('Ctrl Pts',(-0.526867829583898,0.412973481087001,
1.7475));
#38222=CARTESIAN_POINT('Ctrl Pts',(-0.529402816011311,0.409267709604622,
1.7475));
#38223=CARTESIAN_POINT('Ctrl Pts',(-0.531898464539994,0.405537607383136,
1.7475));
#38224=CARTESIAN_POINT('Ctrl Pts',(-0.549961436224517,0.378539923200975,
1.7475));
#38225=CARTESIAN_POINT('Ctrl Pts',(-0.565967543335006,0.350269649024675,
1.7475));
#38226=CARTESIAN_POINT('Ctrl Pts',(-0.579839900985994,0.32098090427459,
1.7475));
#38227=CARTESIAN_POINT('Ctrl Pts',(-0.593599071234153,0.291931132382169,
1.7475));
#38228=CARTESIAN_POINT('Ctrl Pts',(-0.605259453146915,0.26187818221775,
1.7475));
#38229=CARTESIAN_POINT('Ctrl Pts',(-0.614696977596504,0.231057442915654,
1.7475));
#38230=CARTESIAN_POINT('Ctrl Pts',(-0.617111680413263,0.223171590390992,
1.7475));
#38231=CARTESIAN_POINT('Ctrl Pts',(-0.61938059889099,0.215235463519407,
1.7475));
#38232=CARTESIAN_POINT('Ctrl Pts',(-0.621501097336438,0.20725302330997,
1.7475));
#38233=CARTESIAN_POINT('Ctrl Pts',(-0.623104950924263,0.201215449739949,
1.7475));
#38234=CARTESIAN_POINT('Ctrl Pts',(-0.624623079632104,0.195154132702508,
1.7475));
#38235=CARTESIAN_POINT('Ctrl Pts',(-0.626052823098529,0.189078984025834,
1.7475));
#38236=CARTESIAN_POINT('Ctrl Pts',(-0.633111115640263,0.159087466245572,
1.7475));
#38237=CARTESIAN_POINT('Ctrl Pts',(-0.638034496402489,0.128701730040447,
1.7475));
#38238=CARTESIAN_POINT('Ctrl Pts',(-0.640738798776169,0.0981336645007876,
1.7475));
#38239=CARTESIAN_POINT('Ctrl Pts',(-0.643080565572788,0.0716635176657487,
1.7475));
#38240=CARTESIAN_POINT('Ctrl Pts',(-0.643757566809919,0.0450560119454282,
1.7475));
#38241=CARTESIAN_POINT('Ctrl Pts',(-0.64278612619871,0.0184659463280288,
1.7475));
#38242=CARTESIAN_POINT('Ctrl Pts',(-0.642239859902067,0.00351366154119593,
1.7475));
#38243=CARTESIAN_POINT('Ctrl Pts',(-0.641171886318131,-0.0114330384723897,
1.7475));
#38244=CARTESIAN_POINT('Ctrl Pts',(-0.639581752812397,-0.0263454637940612,
1.7475));
#38245=CARTESIAN_POINT('Ctrl Pts',(-0.638821341683572,-0.033476672671481,
1.7475));
#38246=CARTESIAN_POINT('Ctrl Pts',(-0.637941215467033,-0.0406019406396422,
1.7475));
#38247=CARTESIAN_POINT('Ctrl Pts',(-0.636942000003881,-0.0477119642894318,
1.7475));
#38248=CARTESIAN_POINT('Ctrl Pts',(-0.632589769711551,-0.0786807207278065,
1.7475));
#38249=CARTESIAN_POINT('Ctrl Pts',(-0.626003853427657,-0.109216644694058,
1.7475));
#38250=CARTESIAN_POINT('Ctrl Pts',(-0.617229743220339,-0.139071444102893,
1.7475));
#38251=CARTESIAN_POINT('Ctrl Pts',(-0.609757341898868,-0.164497047073868,
1.7475));
#38252=CARTESIAN_POINT('Ctrl Pts',(-0.600696874850192,-0.189429019959063,
1.7475));
#38253=CARTESIAN_POINT('Ctrl Pts',(-0.590048925338361,-0.213702422383968,
1.7475));
#38254=CARTESIAN_POINT('Ctrl Pts',(-0.583925064501878,-0.227662569200301,
1.7475));
#38255=CARTESIAN_POINT('Ctrl Pts',(-0.577275630989656,-0.241404620746393,
1.7475));
#38256=CARTESIAN_POINT('Ctrl Pts',(-0.570116349152705,-0.254901826761342,
1.7475));
#38257=CARTESIAN_POINT('Ctrl Pts',(-0.5668391958013,-0.261080157903191,
1.7475));
#38258=CARTESIAN_POINT('Ctrl Pts',(-0.563455183893963,-0.267207155380128,
1.7475));
#38259=CARTESIAN_POINT('Ctrl Pts',(-0.559965690040735,-0.273280088753028,
1.7475));
#38260=CARTESIAN_POINT('Ctrl Pts',(-0.556766845051595,-0.278847191979564,
1.7475));
#38261=CARTESIAN_POINT('Ctrl Pts',(-0.553481278724128,-0.284365348726348,
1.7475));
#38262=CARTESIAN_POINT('Ctrl Pts',(-0.550114798073169,-0.289825771644315,
1.7475));
#38263=CARTESIAN_POINT('Ctrl Pts',(-0.533995756195628,-0.31597081592334,
1.7475));
#38264=CARTESIAN_POINT('Ctrl Pts',(-0.515996952170829,-0.340844013897456,
1.7475));
#38265=CARTESIAN_POINT('Ctrl Pts',(-0.496279916030761,-0.364250604271942,
1.7475));
#38266=CARTESIAN_POINT('Ctrl Pts',(-0.476916572129198,-0.387237317678789,
1.7475));
#38267=CARTESIAN_POINT('Ctrl Pts',(-0.455895145313256,-0.408810364956492,
1.7475));
#38268=CARTESIAN_POINT('Ctrl Pts',(-0.433336781370987,-0.428747731558718,
1.7475));
#38269=CARTESIAN_POINT('Ctrl Pts',(-0.423171392722634,-0.437732030271826,
1.7475));
#38270=CARTESIAN_POINT('Ctrl Pts',(-0.412693557907652,-0.446383597635371,
1.7475));
#38271=CARTESIAN_POINT('Ctrl Pts',(-0.401912945313201,-0.454678905261359,
1.7475));
#38272=CARTESIAN_POINT('Ctrl Pts',(-0.264547476698427,0.546151586166785,
0.650549949443909));
#38273=CARTESIAN_POINT('Ctrl Pts',(-0.355471695633361,0.502109284909664,
0.654524406148822));
#38274=CARTESIAN_POINT('Ctrl Pts',(-0.514804064846549,0.367775712187168,
0.662473319558649));
#38275=CARTESIAN_POINT('Ctrl Pts',(-0.628053036159548,0.0762413236404022,
0.674396689673389));
#38276=CARTESIAN_POINT('Ctrl Pts',(-0.587854166749295,-0.233845911034667,
0.68632005978813));
#38277=CARTESIAN_POINT('Ctrl Pts',(-0.404047259959307,-0.48683940429689,
0.698243429902869));
#38278=CARTESIAN_POINT('Ctrl Pts',(-0.121527158351189,-0.620878871458333,
0.710166800017609));
#38279=CARTESIAN_POINT('Ctrl Pts',(0.190680748588941,-0.603244694242624,
0.72209017013235));
#38280=CARTESIAN_POINT('Ctrl Pts',(0.456305609272025,-0.438231596848221,
0.734013540247088));
#38281=CARTESIAN_POINT('Ctrl Pts',(0.61045325274331,-0.166159471325954,
0.74593691036183));
#38282=CARTESIAN_POINT('Ctrl Pts',(0.615465575874622,0.146507028070995,
0.75786028047657));
#38283=CARTESIAN_POINT('Ctrl Pts',(0.470117741946454,0.423380863786649,
0.76978365059131));
#38284=CARTESIAN_POINT('Ctrl Pts',(0.209918811260263,0.596821791269607,
0.78170702070605));
#38285=CARTESIAN_POINT('Ctrl Pts',(-0.101563929551992,0.624457254778657,
0.79363039082079));
#38286=CARTESIAN_POINT('Ctrl Pts',(-0.388234290052265,0.499536043242417,
0.805553760935531));
#38287=CARTESIAN_POINT('Ctrl Pts',(-0.580057876616252,0.252576669093317,
0.817477131050269));
#38288=CARTESIAN_POINT('Ctrl Pts',(-0.63017161211444,-0.056087911206034,
0.829400501165011));
#38289=CARTESIAN_POINT('Ctrl Pts',(-0.526332568352355,-0.351050058657002,
0.841323871279751));
#38290=CARTESIAN_POINT('Ctrl Pts',(-0.293908927059336,-0.560249638256679,
0.85324724139449));
#38291=CARTESIAN_POINT('Ctrl Pts',(0.0103175303644349,-0.632578583371251,
0.865170611509231));
#38292=CARTESIAN_POINT('Ctrl Pts',(0.31202338494245,-0.550366716242752,
0.877093981623972));
#38293=CARTESIAN_POINT('Ctrl Pts',(0.537501007448335,-0.333698639877864,
0.889017351738711));
#38294=CARTESIAN_POINT('Ctrl Pts',(0.631665550747977,-0.0355070026353613,
0.900940721853452));
#38295=CARTESIAN_POINT('Ctrl Pts',(0.571512339483762,0.271359099787061,
0.912864091968191));
#38296=CARTESIAN_POINT('Ctrl Pts',(0.371736980381227,0.51193137495119,0.924787462082931));
#38297=CARTESIAN_POINT('Ctrl Pts',(0.0811451820615032,0.627437307350318,
0.936710832197672));
#38298=CARTESIAN_POINT('Ctrl Pts',(-0.229270623235126,0.589658457546506,
0.948634202312412));
#38299=CARTESIAN_POINT('Ctrl Pts',(-0.483674939990074,0.407824309791941,
0.960557572427152));
#38300=CARTESIAN_POINT('Ctrl Pts',(-0.619916044302459,0.12635748196595,
0.972480942541892));
#38301=CARTESIAN_POINT('Ctrl Pts',(-0.604709833109451,-0.185978850876312,
0.984404312656632));
#38302=CARTESIAN_POINT('Ctrl Pts',(-0.441771228592792,-0.452880002671609,
0.996327682771373));
#38303=CARTESIAN_POINT('Ctrl Pts',(-0.170906611750865,-0.6091412359152,
1.00825105288611));
#38304=CARTESIAN_POINT('Ctrl Pts',(0.141710993725228,-0.616587471077492,
1.02017442300085));
#38305=CARTESIAN_POINT('Ctrl Pts',(0.419708186042773,-0.473399570976854,
1.03209779311559));
#38306=CARTESIAN_POINT('Ctrl Pts',(0.595169432313768,-0.214558761349135,
1.04402116323033));
#38307=CARTESIAN_POINT('Ctrl Pts',(0.625229033275726,0.0966993856312912,
1.05594453334507));
#38308=CARTESIAN_POINT('Ctrl Pts',(0.502543339876973,0.384333587886446,
1.06786790345981));
#38309=CARTESIAN_POINT('Ctrl Pts',(0.257084828369703,0.578073962615934,
1.07979127357455));
#38310=CARTESIAN_POINT('Ctrl Pts',(-0.0511802639184789,0.630589165636079,
1.09171464368929));
#38311=CARTESIAN_POINT('Ctrl Pts',(-0.346941866986512,0.529049578172294,
1.10363801380403));
#38312=CARTESIAN_POINT('Ctrl Pts',(-0.557944550077233,0.298261620513743,
1.11556138391877));
#38313=CARTESIAN_POINT('Ctrl Pts',(-0.632639736230396,-0.00539252952743912,
1.12748475403351));
#38314=CARTESIAN_POINT('Ctrl Pts',(-0.552779171463751,-0.307729268722068,
1.13940812414825));
#38315=CARTESIAN_POINT('Ctrl Pts',(-0.337873026968778,-0.534886841191037,
1.15133149426299));
#38316=CARTESIAN_POINT('Ctrl Pts',(-0.0404235068239226,-0.631369982916851,
1.16325486437773));
#38317=CARTESIAN_POINT('Ctrl Pts',(0.26690159510024,-0.573607578197252,
1.17517823449247));
#38318=CARTESIAN_POINT('Ctrl Pts',(0.509021851217201,-0.375711152636948,
1.18710160460721));
#38319=CARTESIAN_POINT('Ctrl Pts',(0.626786569823609,-0.0860273858787084,
1.19902497472195));
#38320=CARTESIAN_POINT('Ctrl Pts',(0.591425483303132,0.224673124632266,
1.21094834483669));
#38321=CARTESIAN_POINT('Ctrl Pts',(0.411577409244242,0.480485329049876,
1.22287171495143));
#38322=CARTESIAN_POINT('Ctrl Pts',(0.131179761858824,0.618913552373053,
1.23479508506618));
#38323=CARTESIAN_POINT('Ctrl Pts',(-0.181265487721769,0.606139371921474,
1.24671845518091));
#38324=CARTESIAN_POINT('Ctrl Pts',(-0.449427044757826,0.445283557604159,
1.25864182529566));
#38325=CARTESIAN_POINT('Ctrl Pts',(-0.607792251030169,0.175643658638878,
1.2705651954104));
#38326=CARTESIAN_POINT('Ctrl Pts',(-0.617672020202178,-0.136906503467616,
1.28248856552514));
#38327=CARTESIAN_POINT('Ctrl Pts',(-0.476652695565553,-0.416010003536527,
1.29441193563987));
#38328=CARTESIAN_POINT('Ctrl Pts',(-0.219185713483245,-0.593481034437674,
1.30633530575462));
#38329=CARTESIAN_POINT('Ctrl Pts',(0.0918289839862619,-0.625962900603877,
1.31825867586936));
#38330=CARTESIAN_POINT('Ctrl Pts',(0.380409590197501,-0.505520186459593,
1.3301820459841));
#38331=CARTESIAN_POINT('Ctrl Pts',(0.576055013076121,-0.26157740181873,
1.34210541609884));
#38332=CARTESIAN_POINT('Ctrl Pts',(0.630968499564522,0.0462695125289182,
1.35402878621358));
#38333=CARTESIAN_POINT('Ctrl Pts',(0.531734523173002,0.34281264868491,1.36595215632832));
#38334=CARTESIAN_POINT('Ctrl Pts',(0.302596236614874,0.555605645056675,
1.37787552644306));
#38335=CARTESIAN_POINT('Ctrl Pts',(-0.000467201806429895,0.632662545876497,
1.3897988965578));
#38336=CARTESIAN_POINT('Ctrl Pts',(-0.303416501450367,0.555158123312486,
1.40172226667254));
#38337=CARTESIAN_POINT('Ctrl Pts',(-0.532240256115767,0.3420269360772,1.41364563678728));
#38338=CARTESIAN_POINT('Ctrl Pts',(-0.631036148567181,0.0453375609608587,
1.42556900690202));
#38339=CARTESIAN_POINT('Ctrl Pts',(-0.575668051287862,-0.262427913831801,
1.43749237701676));
#38340=CARTESIAN_POINT('Ctrl Pts',(-0.379662553523367,-0.506081476332481,
1.4494157471315));
#38341=CARTESIAN_POINT('Ctrl Pts',(-0.0909043756851951,-0.626097843558096,
1.46133911724624));
#38342=CARTESIAN_POINT('Ctrl Pts',(0.220062008878289,-0.593156663530657,
1.47326248736098));
#38343=CARTESIAN_POINT('Ctrl Pts',(0.477266596511919,-0.415305563499184,
1.48518585747572));
#38344=CARTESIAN_POINT('Ctrl Pts',(0.617873548883792,-0.135994091149731,
1.49710922759046));
#38345=CARTESIAN_POINT('Ctrl Pts',(0.607532173409899,0.176541138367681,
1.5090325977052));
#38346=CARTESIAN_POINT('Ctrl Pts',(0.44876889853771,0.445946847509907,1.52095596781994));
#38347=CARTESIAN_POINT('Ctrl Pts',(0.180370060014882,0.606406428909711,
1.53287933793468));
#38348=CARTESIAN_POINT('Ctrl Pts',(-0.132093715531906,0.618719132473601,
1.54480270804942));
#38349=CARTESIAN_POINT('Ctrl Pts',(-0.412286607098983,0.479876931929719,
1.55672607816416));
#38350=CARTESIAN_POINT('Ctrl Pts',(-0.591756666633523,0.223799378893573,
1.5686494482789));
#38351=CARTESIAN_POINT('Ctrl Pts',(-0.626658828732613,-0.0869530124049729,
1.58057281839364));
#38352=CARTESIAN_POINT('Ctrl Pts',(-0.508466394890466,-0.376462544933448,
1.59249618850838));
#38353=CARTESIAN_POINT('Ctrl Pts',(-0.266054119846729,-0.574001132528779,
1.60441955862312));
#38354=CARTESIAN_POINT('Ctrl Pts',(0.041355953716283,-0.631309625261172,
1.61634292873786));
#38355=CARTESIAN_POINT('Ctrl Pts',(0.338662659096756,-0.534387172794291,
1.6282662988526));
#38356=CARTESIAN_POINT('Ctrl Pts',(0.553233053245814,-0.306912647437654,
1.64018966896734));
#38357=CARTESIAN_POINT('Ctrl Pts',(0.63264703504302,-0.004457885988231,
1.65211303908208));
#38358=CARTESIAN_POINT('Ctrl Pts',(0.557503379173826,0.299084810277989,
1.66403640919682));
#38359=CARTESIAN_POINT('Ctrl Pts',(0.346160212094308,0.529562476556959,
1.67595977931156));
#38360=CARTESIAN_POINT('Ctrl Pts',(0.0502486745876001,0.630661949020613,
1.6878831494263));
#38361=CARTESIAN_POINT('Ctrl Pts',(-0.257937943046404,0.577697854759531,
1.69980651954104));
#38362=CARTESIAN_POINT('Ctrl Pts',(-0.503111198644335,0.383582524720304,
1.71172988965578));
#38363=CARTESIAN_POINT('Ctrl Pts',(-0.625369568828046,0.09579278701182,
1.72365325977052));
#38364=CARTESIAN_POINT('Ctrl Pts',(-0.594855848719033,-0.215473244051477,
1.73557662988526));
#38365=CARTESIAN_POINT('Ctrl Pts',(-0.477608641113037,-0.38776777370368,
1.74352554329509));
#38366=CARTESIAN_POINT('Ctrl Pts',(-0.401912945313201,-0.454678905261359,
1.7475));
#38367=CARTESIAN_POINT('Ctrl Pts',(-0.276993436094884,0.571845955096606,
0.667033299629272));
#38368=CARTESIAN_POINT('Ctrl Pts',(-0.372195296045872,0.525731629944139,
0.671007756334186));
#38369=CARTESIAN_POINT('Ctrl Pts',(-0.539023651319926,0.385078170097597,
0.678956669744013));
#38370=CARTESIAN_POINT('Ctrl Pts',(-0.657600558912049,0.0798281899004894,
0.690880039858753));
#38371=CARTESIAN_POINT('Ctrl Pts',(-0.615510484555496,-0.244847477748088,
0.702803409973493));
#38372=CARTESIAN_POINT('Ctrl Pts',(-0.423056157169224,-0.509743359133631,
0.714726780088233));
#38373=CARTESIAN_POINT('Ctrl Pts',(-0.127244552057915,-0.650088876863516,
0.726650150202973));
#38374=CARTESIAN_POINT('Ctrl Pts',(0.199651557474521,-0.63162507822652,
0.738573520317714));
#38375=CARTESIAN_POINT('Ctrl Pts',(0.477773064400501,-0.458848737970438,
0.750496890432453));
#38376=CARTESIAN_POINT('Ctrl Pts',(0.639172772172858,-0.173976646750452,
0.762420260547194));
#38377=CARTESIAN_POINT('Ctrl Pts',(0.644420906172423,0.153399630281469,
0.774343630661934));
#38378=CARTESIAN_POINT('Ctrl Pts',(0.492235005739107,0.443299334019999,
0.786267000776673));
#38379=CARTESIAN_POINT('Ctrl Pts',(0.219794698318813,0.624900001932452,
0.798190370891413));
#38380=CARTESIAN_POINT('Ctrl Pts',(-0.106342128758895,0.653835609600986,
0.810113741006155));
#38381=CARTESIAN_POINT('Ctrl Pts',(-0.406499246764783,0.523037326977394,
0.822037111120894));
#38382=CARTESIAN_POINT('Ctrl Pts',(-0.607347408423773,0.264459447214129,
0.833960481235634));
#38383=CARTESIAN_POINT('Ctrl Pts',(-0.659818805862263,-0.0587266355447204,
0.845883851350374));
#38384=CARTESIAN_POINT('Ctrl Pts',(-0.5510945273644,-0.367565637753413,
0.857807221465114));
#38385=CARTESIAN_POINT('Ctrl Pts',(-0.30773623177639,-0.586607267279053,
0.869730591579855));
#38386=CARTESIAN_POINT('Ctrl Pts',(0.0108029311914999,-0.662339016023882,
0.881653961694595));
#38387=CARTESIAN_POINT('Ctrl Pts',(0.326702906471833,-0.576259391119132,
0.893577331809334));
#38388=CARTESIAN_POINT('Ctrl Pts',(0.562788399328783,-0.349397900269251,
0.905500701924076));
#38389=CARTESIAN_POINT('Ctrl Pts',(0.661383028664851,-0.0371774729743906,
0.917424072038814));
#38390=CARTESIAN_POINT('Ctrl Pts',(0.598399836051714,0.284125520317538,
0.929347442153556));
#38391=CARTESIAN_POINT('Ctrl Pts',(0.389225800995687,0.536015812217164,
0.941270812268294));
#38392=CARTESIAN_POINT('Ctrl Pts',(0.0849627563349745,0.656955862388386,
0.953194182383036));
#38393=CARTESIAN_POINT('Ctrl Pts',(-0.240056939941664,0.617399660418637,
0.965117552497775));
#38394=CARTESIAN_POINT('Ctrl Pts',(-0.50643001873559,0.427010902927905,
0.977040922612516));
#38395=CARTESIAN_POINT('Ctrl Pts',(-0.649080752327234,0.132302124151215,
0.988964292727255));
#38396=CARTESIAN_POINT('Ctrl Pts',(-0.633159146342169,-0.194728453236893,
1.000887662842));
#38397=CARTESIAN_POINT('Ctrl Pts',(-0.462554896016907,-0.474186295950466,
1.01281103295674));
#38398=CARTESIAN_POINT('Ctrl Pts',(-0.178947122199061,-0.637799029909398,
1.02473440307148));
#38399=CARTESIAN_POINT('Ctrl Pts',(0.148377960637735,-0.645595582306399,
1.03665777318622));
#38400=CARTESIAN_POINT('Ctrl Pts',(0.439453870662564,-0.495671232427607,
1.04858114330096));
#38401=CARTESIAN_POINT('Ctrl Pts',(0.623169905729864,-0.224652940531005,
1.0605045134157));
#38402=CARTESIAN_POINT('Ctrl Pts',(0.654643697360791,0.101248726423535,
1.07242788353044));
#38403=CARTESIAN_POINT('Ctrl Pts',(0.526186105557929,0.402415031297763,
1.08435125364518));
#38404=CARTESIAN_POINT('Ctrl Pts',(0.269179698353975,0.605270158764381,
1.09627462375992));
#38405=CARTESIAN_POINT('Ctrl Pts',(-0.0535881019919275,0.660256003699702,
1.10819799387466));
#38406=CARTESIAN_POINT('Ctrl Pts',(-0.363264171184361,0.553939362232308,
1.1201213639894));
#38407=CARTESIAN_POINT('Ctrl Pts',(-0.584193733408707,0.312293703014637,
1.13204473410414));
#38408=CARTESIAN_POINT('Ctrl Pts',(-0.662403045894032,-0.00564622767032119,
1.14396810421888));
#38409=CARTESIAN_POINT('Ctrl Pts',(-0.578785343244735,-0.322206768305185,
1.15589147433362));
#38410=CARTESIAN_POINT('Ctrl Pts',(-0.353768676503191,-0.560051246424626,
1.16781484444836));
#38411=CARTESIAN_POINT('Ctrl Pts',(-0.042325280111924,-0.661073555483839,
1.1797382145631));
#38412=CARTESIAN_POINT('Ctrl Pts',(0.279458306874339,-0.600593647831481,
1.19166158467784));
#38413=CARTESIAN_POINT('Ctrl Pts',(0.532969406382811,-0.393386943042789,
1.20358495479258));
#38414=CARTESIAN_POINT('Ctrl Pts',(0.656274510119339,-0.0900746493982562,
1.21550832490732));
#38415=CARTESIAN_POINT('Ctrl Pts',(0.619249818061811,0.235243146397531,
1.22743169502206));
#38416=CARTESIAN_POINT('Ctrl Pts',(0.430940571531337,0.503090348650062,
1.2393550651368));
#38417=CARTESIAN_POINT('Ctrl Pts',(0.1373512740959,0.648031096939669,1.25127843525154));
#38418=CARTESIAN_POINT('Ctrl Pts',(-0.189793344151622,0.634655939554922,
1.26320180536628));
#38419=CARTESIAN_POINT('Ctrl Pts',(-0.470570889411094,0.466232466839719,
1.27512517548102));
#38420=CARTESIAN_POINT('Ctrl Pts',(-0.636386580381591,0.183907029247991,
1.28704854559576));
#38421=CARTESIAN_POINT('Ctrl Pts',(-0.646731155370297,-0.143347437263448,
1.2989719157105));
#38422=CARTESIAN_POINT('Ctrl Pts',(-0.49907740423886,-0.435581702640041,
1.31089528582524));
#38423=CARTESIAN_POINT('Ctrl Pts',(-0.229497573283767,-0.621402075111968,
1.32281865593998));
#38424=CARTESIAN_POINT('Ctrl Pts',(0.0961491907800454,-0.655412090374398,
1.33474202605472));
#38425=CARTESIAN_POINT('Ctrl Pts',(0.398306424341256,-0.529303001526613,
1.34666539616946));
#38426=CARTESIAN_POINT('Ctrl Pts',(0.603156225275714,-0.273883630412164,
1.3585887662842));
#38427=CARTESIAN_POINT('Ctrl Pts',(0.660653183856468,0.0484463183008557,
1.37051213639894));
#38428=CARTESIAN_POINT('Ctrl Pts',(0.556750623752369,0.358940688760636,
1.38243550651368));
#38429=CARTESIAN_POINT('Ctrl Pts',(0.316832246428428,0.581744791742624,
1.39435887662842));
#38430=CARTESIAN_POINT('Ctrl Pts',(-0.000489181886471275,0.662426928647814,
1.40628224674316));
#38431=CARTESIAN_POINT('Ctrl Pts',(-0.317691101625711,0.581276215790976,
1.4182056168579));
#38432=CARTESIAN_POINT('Ctrl Pts',(-0.557280149519581,0.358118011342924,
1.43012898697264));
#38433=CARTESIAN_POINT('Ctrl Pts',(-0.660724015489144,0.0474705219321574,
1.44205235708738));
#38434=CARTESIAN_POINT('Ctrl Pts',(-0.602751058397144,-0.274774155802465,
1.45397572720212));
#38435=CARTESIAN_POINT('Ctrl Pts',(-0.39752424241369,-0.529890697967634,
1.46589909731686));
#38436=CARTESIAN_POINT('Ctrl Pts',(-0.0951810831513113,-0.655553381884837,
1.4778224674316));
#38437=CARTESIAN_POINT('Ctrl Pts',(0.230415095066762,-0.621062443779154,
1.48974583754634));
#38438=CARTESIAN_POINT('Ctrl Pts',(0.499720186905616,-0.434844121360108,
1.50166920766108));
#38439=CARTESIAN_POINT('Ctrl Pts',(0.646942165215064,-0.142392099392831,
1.51359257777582));
#38440=CARTESIAN_POINT('Ctrl Pts',(0.636114267091785,0.18484673200762,1.52551594789056));
#38441=CARTESIAN_POINT('Ctrl Pts',(0.469881779897605,0.466926962029817,
1.5374393180053));
#38442=CARTESIAN_POINT('Ctrl Pts',(0.188855789953788,0.634935560565594,
1.54936268812004));
#38443=CARTESIAN_POINT('Ctrl Pts',(-0.138308225836652,0.647827530318408,
1.56128605823478));
#38444=CARTESIAN_POINT('Ctrl Pts',(-0.431683134466003,0.502453328743748,
1.57320942834952));
#38445=CARTESIAN_POINT('Ctrl Pts',(-0.619596582316783,0.234328294222587,
1.58513279846426));
#38446=CARTESIAN_POINT('Ctrl Pts',(-0.656140759292581,-0.0910438231558368,
1.597056168579));
#38447=CARTESIAN_POINT('Ctrl Pts',(-0.532387817934254,-0.394173685508301,
1.60897953869374));
#38448=CARTESIAN_POINT('Ctrl Pts',(-0.278570961111662,-0.601005717407574,
1.62090290880848));
#38449=CARTESIAN_POINT('Ctrl Pts',(0.0433015951080595,-0.661010358228473,
1.63282627892322));
#38450=CARTESIAN_POINT('Ctrl Pts',(0.354595457839793,-0.559528070517414,
1.64474964903796));
#38451=CARTESIAN_POINT('Ctrl Pts',(0.579260578450012,-0.321351728074295,
1.6566730191527));
#38452=CARTESIAN_POINT('Ctrl Pts',(0.662410688088217,-0.00466761268340117,
1.66859638926744));
#38453=CARTESIAN_POINT('Ctrl Pts',(0.583731807080909,0.313155620747522,
1.68051975938218));
#38454=CARTESIAN_POINT('Ctrl Pts',(0.362445742382341,0.554476390548393,
1.69244312949692));
#38455=CARTESIAN_POINT('Ctrl Pts',(0.0526126849023013,0.660332211267524,
1.70436649961166));
#38456=CARTESIAN_POINT('Ctrl Pts',(-0.270072948853399,0.604876356454159,
1.7162898697264));
#38457=CARTESIAN_POINT('Ctrl Pts',(-0.526780679935092,0.401628633446949,
1.72821323984114));
#38458=CARTESIAN_POINT('Ctrl Pts',(-0.654790844579946,0.10029947576388,
1.74013660995588));
#38459=CARTESIAN_POINT('Ctrl Pts',(-0.622841569211623,-0.225610446189846,
1.75205998007062));
#38460=CARTESIAN_POINT('Ctrl Pts',(-0.500078323413074,-0.406010782584359,
1.76000889348045));
#38461=CARTESIAN_POINT('Ctrl Pts',(-0.420821431081829,-0.476069830111341,
1.76398335018536));
#38462=CARTESIAN_POINT('Ctrl Pts',(-0.289439395491341,0.597540324026427,
0.683516649814636));
#38463=CARTESIAN_POINT('Ctrl Pts',(-0.388918896458382,0.549353974978614,
0.68749110651955));
#38464=CARTESIAN_POINT('Ctrl Pts',(-0.563243237793303,0.402380628008027,
0.695440019929377));
#38465=CARTESIAN_POINT('Ctrl Pts',(-0.687148081664549,0.0834150561605762,
0.707363390044116));
#38466=CARTESIAN_POINT('Ctrl Pts',(-0.643166802361696,-0.255849044461509,
0.719286760158857));
#38467=CARTESIAN_POINT('Ctrl Pts',(-0.442065054379141,-0.532647313970372,
0.731210130273597));
#38468=CARTESIAN_POINT('Ctrl Pts',(-0.132961945764642,-0.679298882268699,
0.743133500388337));
#38469=CARTESIAN_POINT('Ctrl Pts',(0.208622366360101,-0.660005462210415,
0.755056870503077));
#38470=CARTESIAN_POINT('Ctrl Pts',(0.499240519528978,-0.479465879092654,
0.766980240617817));
#38471=CARTESIAN_POINT('Ctrl Pts',(0.667892291602407,-0.181793822174949,
0.778903610732558));
#38472=CARTESIAN_POINT('Ctrl Pts',(0.673376236470223,0.160292232491944,
0.790826980847297));
#38473=CARTESIAN_POINT('Ctrl Pts',(0.51435226953176,0.463217804253349,0.802750350962038));
#38474=CARTESIAN_POINT('Ctrl Pts',(0.229670585377363,0.652978212595296,
0.814673721076777));
#38475=CARTESIAN_POINT('Ctrl Pts',(-0.111120327965797,0.683213964423316,
0.826597091191518));
#38476=CARTESIAN_POINT('Ctrl Pts',(-0.424764203477302,0.546538610712372,
0.838520461306258));
#38477=CARTESIAN_POINT('Ctrl Pts',(-0.634636940231293,0.27634222533494,
0.850443831420998));
#38478=CARTESIAN_POINT('Ctrl Pts',(-0.689465999610088,-0.0613653598834067,
0.862367201535738));
#38479=CARTESIAN_POINT('Ctrl Pts',(-0.575856486376446,-0.384081216849825,
0.874290571650478));
#38480=CARTESIAN_POINT('Ctrl Pts',(-0.321563536493444,-0.612964896301427,
0.886213941765218));
#38481=CARTESIAN_POINT('Ctrl Pts',(0.0112883320185645,-0.692099448676514,
0.898137311879959));
#38482=CARTESIAN_POINT('Ctrl Pts',(0.341382428001217,-0.602152065995511,
0.910060681994698));
#38483=CARTESIAN_POINT('Ctrl Pts',(0.58807579120923,-0.365097160660638,
0.921984052109439));
#38484=CARTESIAN_POINT('Ctrl Pts',(0.691100506581725,-0.0388479433134198,
0.933907422224178));
#38485=CARTESIAN_POINT('Ctrl Pts',(0.625287332619665,0.296891940848016,
0.94583079233892));
#38486=CARTESIAN_POINT('Ctrl Pts',(0.406714621610146,0.560100249483138,
0.957754162453659));
#38487=CARTESIAN_POINT('Ctrl Pts',(0.0887803306084458,0.686474417426454,
0.969677532568399));
#38488=CARTESIAN_POINT('Ctrl Pts',(-0.250843256648201,0.645140863290769,
0.98160090268314));
#38489=CARTESIAN_POINT('Ctrl Pts',(-0.529185097481107,0.44619749606387,
0.993524272797879));
#38490=CARTESIAN_POINT('Ctrl Pts',(-0.678245460352009,0.13824676633648,
1.00544764291262));
#38491=CARTESIAN_POINT('Ctrl Pts',(-0.661608459574888,-0.203478055597473,
1.01737101302736));
#38492=CARTESIAN_POINT('Ctrl Pts',(-0.483338563441022,-0.495492589229323,
1.0292943831421));
#38493=CARTESIAN_POINT('Ctrl Pts',(-0.186987632647257,-0.666456823903595,
1.04121775325684));
#38494=CARTESIAN_POINT('Ctrl Pts',(0.155044927550243,-0.674603693535307,
1.05314112337158));
#38495=CARTESIAN_POINT('Ctrl Pts',(0.459199555282356,-0.517942893878359,
1.06506449348632));
#38496=CARTESIAN_POINT('Ctrl Pts',(0.651170379145961,-0.234747119712876,
1.07698786360106));
#38497=CARTESIAN_POINT('Ctrl Pts',(0.684058361445857,0.105798067215779,
1.0889112337158));
#38498=CARTESIAN_POINT('Ctrl Pts',(0.549828871238885,0.420496474709079,
1.10083460383054));
#38499=CARTESIAN_POINT('Ctrl Pts',(0.281274568338247,0.632466354912828,
1.11275797394528));
#38500=CARTESIAN_POINT('Ctrl Pts',(-0.0559959400653758,0.689922841763325,
1.12468134406002));
#38501=CARTESIAN_POINT('Ctrl Pts',(-0.37958647538221,0.578829146292321,
1.13660471417476));
#38502=CARTESIAN_POINT('Ctrl Pts',(-0.61044291674018,0.326325785515531,
1.1485280842895));
#38503=CARTESIAN_POINT('Ctrl Pts',(-0.692166355557669,-0.00589992581320304,
1.16045145440424));
#38504=CARTESIAN_POINT('Ctrl Pts',(-0.60479151502572,-0.336684267888303,
1.17237482451898));
#38505=CARTESIAN_POINT('Ctrl Pts',(-0.369664326037605,-0.585215651658216,
1.18429819463372));
#38506=CARTESIAN_POINT('Ctrl Pts',(-0.0442270533999247,-0.690777128050826,
1.19622156474846));
#38507=CARTESIAN_POINT('Ctrl Pts',(0.292015018648436,-0.62757971746571,
1.2081449348632));
#38508=CARTESIAN_POINT('Ctrl Pts',(0.556916961548422,-0.411062733448631,
1.22006830497794));
#38509=CARTESIAN_POINT('Ctrl Pts',(0.68576245041507,-0.0941219129178041,
1.23199167509268));
#38510=CARTESIAN_POINT('Ctrl Pts',(0.647074152820491,0.245813168162796,
1.24391504520742));
#38511=CARTESIAN_POINT('Ctrl Pts',(0.450303733818432,0.52569536825025,1.25583841532216));
#38512=CARTESIAN_POINT('Ctrl Pts',(0.143522786332977,0.677148641506285,
1.2677617854369));
#38513=CARTESIAN_POINT('Ctrl Pts',(-0.198321200581474,0.66317250718837,
1.27968515555164));
#38514=CARTESIAN_POINT('Ctrl Pts',(-0.491714734064362,0.487181376075277,
1.29160852566638));
#38515=CARTESIAN_POINT('Ctrl Pts',(-0.664980909733015,0.192170399857104,
1.30353189578112));
#38516=CARTESIAN_POINT('Ctrl Pts',(-0.675790290538415,-0.149788371059279,
1.31545526589586));
#38517=CARTESIAN_POINT('Ctrl Pts',(-0.521502112912168,-0.455153401743555,
1.3273786360106));
#38518=CARTESIAN_POINT('Ctrl Pts',(-0.23980943308429,-0.649323115786262,
1.33930200612534));
#38519=CARTESIAN_POINT('Ctrl Pts',(0.100469397573829,-0.684861280144919,
1.35122537624008));
#38520=CARTESIAN_POINT('Ctrl Pts',(0.416203258485012,-0.553085816593635,
1.36314874635482));
#38521=CARTESIAN_POINT('Ctrl Pts',(0.630257437475308,-0.286189859005598,
1.37507211646956));
#38522=CARTESIAN_POINT('Ctrl Pts',(0.690337868148412,0.050623124072793,
1.3869954865843));
#38523=CARTESIAN_POINT('Ctrl Pts',(0.581766724331738,0.375068728836361,
1.39891885669904));
#38524=CARTESIAN_POINT('Ctrl Pts',(0.33106825624198,0.607883938428571,1.41084222681378));
#38525=CARTESIAN_POINT('Ctrl Pts',(-0.000511161966512498,0.692191311419132,
1.42276559692852));
#38526=CARTESIAN_POINT('Ctrl Pts',(-0.331965701801056,0.607394308269466,
1.43468896704327));
#38527=CARTESIAN_POINT('Ctrl Pts',(-0.582320042923395,0.374209086608647,
1.446612337158));
#38528=CARTESIAN_POINT('Ctrl Pts',(-0.690411882411108,0.0496034829034569,
1.45853570727274));
#38529=CARTESIAN_POINT('Ctrl Pts',(-0.629834065506428,-0.287120397773129,
1.47045907738748));
#38530=CARTESIAN_POINT('Ctrl Pts',(-0.415385931304013,-0.553699919602786,
1.48238244750222));
#38531=CARTESIAN_POINT('Ctrl Pts',(-0.0994577906174278,-0.68500892021158,
1.49430581761697));
#38532=CARTESIAN_POINT('Ctrl Pts',(0.240768181255235,-0.648968224027652,
1.5062291877317));
#38533=CARTESIAN_POINT('Ctrl Pts',(0.522173777299313,-0.454382679221032,
1.51815255784645));
#38534=CARTESIAN_POINT('Ctrl Pts',(0.676010781546336,-0.148790107635931,
1.53007592796118));
#38535=CARTESIAN_POINT('Ctrl Pts',(0.664696360773671,0.193152325647559,
1.54199929807593));
#38536=CARTESIAN_POINT('Ctrl Pts',(0.490994661257499,0.487907076549728,
1.55392266819067));
#38537=CARTESIAN_POINT('Ctrl Pts',(0.197341519892694,0.663464692221476,
1.56584603830541));
#38538=CARTESIAN_POINT('Ctrl Pts',(-0.144522736141398,0.676935928163215,
1.57776940842015));
#38539=CARTESIAN_POINT('Ctrl Pts',(-0.451079661833022,0.525029725557777,
1.58969277853489));
#38540=CARTESIAN_POINT('Ctrl Pts',(-0.647436498000044,0.2448572095516,1.60161614864963));
#38541=CARTESIAN_POINT('Ctrl Pts',(-0.685622689852549,-0.0951346339067004,
1.61353951876436));
#38542=CARTESIAN_POINT('Ctrl Pts',(-0.556309240978042,-0.411884826083155,
1.62546288887911));
#38543=CARTESIAN_POINT('Ctrl Pts',(-0.291087802376595,-0.628010302286368,
1.63738625899384));
#38544=CARTESIAN_POINT('Ctrl Pts',(0.0452472364998361,-0.690711091195774,
1.64930962910859));
#38545=CARTESIAN_POINT('Ctrl Pts',(0.37052825658283,-0.584668968240537,
1.66123299922332));
#38546=CARTESIAN_POINT('Ctrl Pts',(0.605288103654211,-0.335790808710935,
1.67315636933807));
#38547=CARTESIAN_POINT('Ctrl Pts',(0.692174341133415,-0.00487733937857217,
1.6850797394528));
#38548=CARTESIAN_POINT('Ctrl Pts',(0.609960234987991,0.327226431217055,
1.69700310956755));
#38549=CARTESIAN_POINT('Ctrl Pts',(0.378731272670374,0.579390304539825,
1.70892647968229));
#38550=CARTESIAN_POINT('Ctrl Pts',(0.0549766952170021,0.690002473514437,
1.72084984979703));
#38551=CARTESIAN_POINT('Ctrl Pts',(-0.282207954660393,0.632054858148786,
1.73277321991177));
#38552=CARTESIAN_POINT('Ctrl Pts',(-0.550450161225849,0.419674742173595,
1.74469659002651));
#38553=CARTESIAN_POINT('Ctrl Pts',(-0.684212120331845,0.104806164515941,
1.75661996014125));
#38554=CARTESIAN_POINT('Ctrl Pts',(-0.650827289704214,-0.235747648328215,
1.76854333025599));
#38555=CARTESIAN_POINT('Ctrl Pts',(-0.522548005713111,-0.424253791465037,
1.77649224366581));
#38556=CARTESIAN_POINT('Ctrl Pts',(-0.439729916850458,-0.497460754961323,
1.78046670037073));
#38557=CARTESIAN_POINT('Ctrl Pts',(-0.301885354887798,0.623234692956248,
0.7));
#38558=CARTESIAN_POINT('Ctrl Pts',(-0.405642496870893,0.572976320013089,
0.703974456704914));
#38559=CARTESIAN_POINT('Ctrl Pts',(-0.58746282426668,0.419683085918456,
0.711923370114741));
#38560=CARTESIAN_POINT('Ctrl Pts',(-0.71669560441705,0.0870019224206636,
0.72384674022948));
#38561=CARTESIAN_POINT('Ctrl Pts',(-0.670823120167895,-0.26685061117493,
0.735770110344222));
#38562=CARTESIAN_POINT('Ctrl Pts',(-0.461073951589059,-0.555551268807112,
0.747693480458959));
#38563=CARTESIAN_POINT('Ctrl Pts',(-0.138679339471368,-0.708508887673882,
0.759616850573702));
#38564=CARTESIAN_POINT('Ctrl Pts',(0.21759317524568,-0.688385846194311,
0.77154022068844));
#38565=CARTESIAN_POINT('Ctrl Pts',(0.520707974657454,-0.50008302021487,
0.783463590803181));
#38566=CARTESIAN_POINT('Ctrl Pts',(0.696611811031955,-0.189610997599447,
0.795386960917921));
#38567=CARTESIAN_POINT('Ctrl Pts',(0.702331566768025,0.167184834702419,
0.807310331032661));
#38568=CARTESIAN_POINT('Ctrl Pts',(0.536469533324413,0.483136274486699,
0.819233701147402));
#38569=CARTESIAN_POINT('Ctrl Pts',(0.239546472435912,0.681056423258141,
0.831157071262141));
#38570=CARTESIAN_POINT('Ctrl Pts',(-0.1158985271727,0.712592319245645,0.843080441376882));
#38571=CARTESIAN_POINT('Ctrl Pts',(-0.443029160189821,0.57003989444735,
0.855003811491621));
#38572=CARTESIAN_POINT('Ctrl Pts',(-0.661926472038813,0.288225003455751,
0.866927181606362));
#38573=CARTESIAN_POINT('Ctrl Pts',(-0.719113193357913,-0.0640040842220929,
0.878850551721102));
#38574=CARTESIAN_POINT('Ctrl Pts',(-0.600618445388491,-0.400596795946236,
0.890773921835841));
#38575=CARTESIAN_POINT('Ctrl Pts',(-0.335390841210499,-0.639322525323802,
0.902697291950582));
#38576=CARTESIAN_POINT('Ctrl Pts',(0.0117737328456294,-0.721859881329144,
0.914620662065322));
#38577=CARTESIAN_POINT('Ctrl Pts',(0.356061949530601,-0.62804474087189,
0.926544032180063));
#38578=CARTESIAN_POINT('Ctrl Pts',(0.613363183089679,-0.380796421052026,
0.938467402294802));
#38579=CARTESIAN_POINT('Ctrl Pts',(0.720817984498598,-0.0405184136524491,
0.950390772409543));
#38580=CARTESIAN_POINT('Ctrl Pts',(0.652174829187617,0.309658361378493,
0.962314142524283));
#38581=CARTESIAN_POINT('Ctrl Pts',(0.424203442224605,0.584184686749112,
0.974237512639022));
#38582=CARTESIAN_POINT('Ctrl Pts',(0.0925979048819177,0.715992972464522,
0.986160882753764));
#38583=CARTESIAN_POINT('Ctrl Pts',(-0.26162957335474,0.672882066162899,
0.998084252868503));
#38584=CARTESIAN_POINT('Ctrl Pts',(-0.551940176226622,0.465384089199835,
1.01000762298324));
#38585=CARTESIAN_POINT('Ctrl Pts',(-0.707410168376785,0.144191408521745,
1.02193099309798));
#38586=CARTESIAN_POINT('Ctrl Pts',(-0.690057772807605,-0.212227657958053,
1.03385436321272));
#38587=CARTESIAN_POINT('Ctrl Pts',(-0.504122230865138,-0.51679888250818,
1.04577773332746));
#38588=CARTESIAN_POINT('Ctrl Pts',(-0.195028143095452,-0.695114617897793,
1.0577011034422));
#38589=CARTESIAN_POINT('Ctrl Pts',(0.161711894462749,-0.703611804764214,
1.06962447355694));
#38590=CARTESIAN_POINT('Ctrl Pts',(0.478945239902149,-0.540214555329112,
1.08154784367168));
#38591=CARTESIAN_POINT('Ctrl Pts',(0.679170852562056,-0.244841298894746,
1.09347121378642));
#38592=CARTESIAN_POINT('Ctrl Pts',(0.713473025530922,0.110347408008022,
1.10539458390116));
#38593=CARTESIAN_POINT('Ctrl Pts',(0.57347163691984,0.438577918120396,1.1173179540159));
#38594=CARTESIAN_POINT('Ctrl Pts',(0.293369438322519,0.659662551061274,
1.12924132413064));
#38595=CARTESIAN_POINT('Ctrl Pts',(-0.0584037781388241,0.719589679826949,
1.14116469424538));
#38596=CARTESIAN_POINT('Ctrl Pts',(-0.395908779580059,0.603718930352334,
1.15308806436013));
#38597=CARTESIAN_POINT('Ctrl Pts',(-0.636692100071654,0.340357868016426,
1.16501143447486));
#38598=CARTESIAN_POINT('Ctrl Pts',(-0.721929665221305,-0.00615362395608558,
1.17693480458961));
#38599=CARTESIAN_POINT('Ctrl Pts',(-0.630797686806703,-0.35116176747142,
1.18885817470434));
#38600=CARTESIAN_POINT('Ctrl Pts',(-0.385559975572019,-0.610380056891805,
1.20078154481909));
#38601=CARTESIAN_POINT('Ctrl Pts',(-0.0461288266879255,-0.720480700617813,
1.21270491493383));
#38602=CARTESIAN_POINT('Ctrl Pts',(0.304571730422535,-0.654565787099938,
1.22462828504857));
#38603=CARTESIAN_POINT('Ctrl Pts',(0.580864516714032,-0.428738523854473,
1.2365516551633));
#38604=CARTESIAN_POINT('Ctrl Pts',(0.7152503907108,-0.0981691764373513,
1.24847502527805));
#38605=CARTESIAN_POINT('Ctrl Pts',(0.674898487579171,0.25638318992806,1.26039839539278));
#38606=CARTESIAN_POINT('Ctrl Pts',(0.469666896105526,0.548300387850438,
1.27232176550753));
#38607=CARTESIAN_POINT('Ctrl Pts',(0.149694298570053,0.706266186072899,
1.28424513562226));
#38608=CARTESIAN_POINT('Ctrl Pts',(-0.206849057011327,0.691689074821819,
1.29616850573701));
#38609=CARTESIAN_POINT('Ctrl Pts',(-0.51285857871763,0.508130285310836,
1.30809187585175));
#38610=CARTESIAN_POINT('Ctrl Pts',(-0.693575239084438,0.200433770466217,
1.32001524596649));
#38611=CARTESIAN_POINT('Ctrl Pts',(-0.704849425706532,-0.15622930485511,
1.33193861608123));
#38612=CARTESIAN_POINT('Ctrl Pts',(-0.543926821585475,-0.474725100847069,
1.34386198619597));
#38613=CARTESIAN_POINT('Ctrl Pts',(-0.250121292884812,-0.677244156460556,
1.35578535631071));
#38614=CARTESIAN_POINT('Ctrl Pts',(0.104789604367612,-0.71431046991544,
1.36770872642545));
#38615=CARTESIAN_POINT('Ctrl Pts',(0.434100092628769,-0.576868631660655,
1.37963209654019));
#38616=CARTESIAN_POINT('Ctrl Pts',(0.6573586496749,-0.298496087599031,1.39155546665493));
#38617=CARTESIAN_POINT('Ctrl Pts',(0.720022552440358,0.0527999298447306,
1.40347883676967));
#38618=CARTESIAN_POINT('Ctrl Pts',(0.606782824911105,0.391196768912086,
1.41540220688441));
#38619=CARTESIAN_POINT('Ctrl Pts',(0.345304266055534,0.634023085114521,
1.42732557699915));
#38620=CARTESIAN_POINT('Ctrl Pts',(-0.000533142046554097,0.721955694190449,
1.43924894711389));
#38621=CARTESIAN_POINT('Ctrl Pts',(-0.3462403019764,0.633512400747956,1.45117231722863));
#38622=CARTESIAN_POINT('Ctrl Pts',(-0.60735993632721,0.390300161874371,
1.46309568734337));
#38623=CARTESIAN_POINT('Ctrl Pts',(-0.72009974933307,0.0517364438747562,
1.47501905745811));
#38624=CARTESIAN_POINT('Ctrl Pts',(-0.656917072615711,-0.299466639743793,
1.48694242757285));
#38625=CARTESIAN_POINT('Ctrl Pts',(-0.433247620194335,-0.577509141237938,
1.49886579768759));
#38626=CARTESIAN_POINT('Ctrl Pts',(-0.103734498083544,-0.714464458538322,
1.51078916780233));
#38627=CARTESIAN_POINT('Ctrl Pts',(0.251121267443708,-0.676874004276149,
1.52271253791707));
#38628=CARTESIAN_POINT('Ctrl Pts',(0.54462736769301,-0.473921237081957,
1.53463590803181));
#38629=CARTESIAN_POINT('Ctrl Pts',(0.705079397877607,-0.155188115879031,
1.54655927814655));
#38630=CARTESIAN_POINT('Ctrl Pts',(0.693278454455557,0.201457919287497,
1.55848264826129));
#38631=CARTESIAN_POINT('Ctrl Pts',(0.512107542617394,0.508887191069639,
1.57040601837603));
#38632=CARTESIAN_POINT('Ctrl Pts',(0.2058272498316,0.691993823877357,1.58232938849077));
#38633=CARTESIAN_POINT('Ctrl Pts',(-0.150737246446145,0.706044326008023,
1.59425275860551));
#38634=CARTESIAN_POINT('Ctrl Pts',(-0.470476189200041,0.547606122371807,
1.60617612872025));
#38635=CARTESIAN_POINT('Ctrl Pts',(-0.675276413683305,0.255386124880614,
1.61809949883499));
#38636=CARTESIAN_POINT('Ctrl Pts',(-0.715104620412515,-0.0992254446575641,
1.63002286894973));
#38637=CARTESIAN_POINT('Ctrl Pts',(-0.580230664021831,-0.429595966658007,
1.64194623906447));
#38638=CARTESIAN_POINT('Ctrl Pts',(-0.303604643641527,-0.655014887165163,
1.65386960917921));
#38639=CARTESIAN_POINT('Ctrl Pts',(0.0471928778916124,-0.720411824163075,
1.66579297929395));
#38640=CARTESIAN_POINT('Ctrl Pts',(0.386461055325867,-0.60980986596366,
1.67771634940869));
#38641=CARTESIAN_POINT('Ctrl Pts',(0.631315628858409,-0.350229889347576,
1.68963971952343));
#38642=CARTESIAN_POINT('Ctrl Pts',(0.721937994178612,-0.00508706607374287,
1.70156308963817));
#38643=CARTESIAN_POINT('Ctrl Pts',(0.636188662895073,0.341297241686589,
1.71348645975291));
#38644=CARTESIAN_POINT('Ctrl Pts',(0.395016802958407,0.604304218531258,
1.72540982986765));
#38645=CARTESIAN_POINT('Ctrl Pts',(0.0573407055317036,0.719672735761348,
1.73733319998239));
#38646=CARTESIAN_POINT('Ctrl Pts',(-0.294342960467388,0.659233359843414,
1.74925657009713));
#38647=CARTESIAN_POINT('Ctrl Pts',(-0.574119642516605,0.437720850900241,
1.76117994021187));
#38648=CARTESIAN_POINT('Ctrl Pts',(-0.713633396083747,0.109312853268001,
1.77310331032661));
#38649=CARTESIAN_POINT('Ctrl Pts',(-0.678813010196804,-0.245884850466584,
1.78502668044135));
#38650=CARTESIAN_POINT('Ctrl Pts',(-0.545017688013148,-0.442496800345716,
1.79297559385118));
#38651=CARTESIAN_POINT('Ctrl Pts',(-0.458638402619086,-0.518851679811305,
1.79695005055609));
#38652=CARTESIAN_POINT('Ctrl Pts',(-0.692483926679543,-1.76726015421153E-5,
1.62673131746348));
#38653=CARTESIAN_POINT('Ctrl Pts',(-0.692514701573625,-0.0318455918606296,
1.62782850129223));
#38654=CARTESIAN_POINT('Ctrl Pts',(-0.690360629478052,-0.0636693787307131,
1.62892568512098));
#38655=CARTESIAN_POINT('Ctrl Pts',(-0.685987593225867,-0.0951852700679401,
1.63002286894973));
#38656=CARTESIAN_POINT('Ctrl Pts',(-0.670146634948955,-0.209348951991043,
1.63399732565464));
#38657=CARTESIAN_POINT('Ctrl Pts',(-0.625188649485394,-0.319472459324523,
1.63797178235956));
#38658=CARTESIAN_POINT('Ctrl Pts',(-0.556605320023564,-0.412104033075788,
1.64194623906447));
#38659=CARTESIAN_POINT('Ctrl Pts',(-0.488021990561732,-0.504735606827057,
1.64592069576938));
#38660=CARTESIAN_POINT('Ctrl Pts',(-0.39581331710163,-0.57987524699611,
1.6498951524743));
#38661=CARTESIAN_POINT('Ctrl Pts',(-0.291242726782721,-0.628344556580289,
1.65386960917921));
#38662=CARTESIAN_POINT('Ctrl Pts',(-0.186672136463813,-0.676813866164467,
1.65784406588412));
#38663=CARTESIAN_POINT('Ctrl Pts',(-0.0697396292860975,-0.698612845163772,
1.66181852258904));
#38664=CARTESIAN_POINT('Ctrl Pts',(0.0452713205418031,-0.69107867496352,
1.66579297929395));
#38665=CARTESIAN_POINT('Ctrl Pts',(0.160282270369701,-0.683544504763269,
1.66976743599886));
#38666=CARTESIAN_POINT('Ctrl Pts',(0.273371662847784,-0.646677185363464,
1.67374189270378));
#38667=CARTESIAN_POINT('Ctrl Pts',(0.370725454675582,-0.584980196227548,
1.67771634940869));
#38668=CARTESIAN_POINT('Ctrl Pts',(0.468079246503381,-0.523283207091632,
1.6816908061136));
#38669=CARTESIAN_POINT('Ctrl Pts',(0.549697437680895,-0.436756548219604,
1.68566526281852));
#38670=CARTESIAN_POINT('Ctrl Pts',(0.605610260823019,-0.335969414904618,
1.68963971952343));
#38671=CARTESIAN_POINT('Ctrl Pts',(0.661523083965143,-0.235182281589633,
1.69361417622834));
#38672=CARTESIAN_POINT('Ctrl Pts',(0.691730539071877,-0.120134673831689,
1.69758863293326));
#38673=CARTESIAN_POINT('Ctrl Pts',(0.692542711411322,-0.00488015199266319,
1.70156308963817));
#38674=CARTESIAN_POINT('Ctrl Pts',(0.693354883750767,0.110374369846365,
1.70553754634308));
#38675=CARTESIAN_POINT('Ctrl Pts',(0.664771773322921,0.225835805766476,
1.709512003048));
#38676=CARTESIAN_POINT('Ctrl Pts',(0.610284908119553,0.32740101986731,1.71348645975291));
#38677=CARTESIAN_POINT('Ctrl Pts',(0.555798042916185,0.428966233968145,
1.71746091645782));
#38678=CARTESIAN_POINT('Ctrl Pts',(0.475407422937294,0.516635226249703,
1.72143537316274));
#38679=CARTESIAN_POINT('Ctrl Pts',(0.37893276337673,0.579697808595497,1.72540982986765));
#38680=CARTESIAN_POINT('Ctrl Pts',(0.282458103816171,0.642760390941288,
1.72938428657257));
#38681=CARTESIAN_POINT('Ctrl Pts',(0.16989940467394,0.681216563351317,1.73335874327748));
#38682=CARTESIAN_POINT('Ctrl Pts',(0.0550061107696439,0.690371420236677,
1.73733319998239));
#38683=CARTESIAN_POINT('Ctrl Pts',(-0.0429609179519917,0.698177568854695,
1.74072213332159));
#38684=CARTESIAN_POINT('Ctrl Pts',(-0.142625338155946,0.684679890273028,
1.7441110666608));
#38685=CARTESIAN_POINT('Ctrl Pts',(-0.235110047033021,0.651400850437653,
1.7475));
#38686=CARTESIAN_POINT('',(-0.352210602859808,-0.494214587872355,0.7));
#38687=CARTESIAN_POINT('Ctrl Pts',(-0.352210602859807,-0.494214587872356,
0.7));
#38688=CARTESIAN_POINT('Ctrl Pts',(-0.36497036554318,-0.486388617262107,
0.7));
#38689=CARTESIAN_POINT('Ctrl Pts',(-0.377422115114145,-0.478097231538959,
0.7));
#38690=CARTESIAN_POINT('Ctrl Pts',(-0.389538285381734,-0.469355126779466,
0.7));
#38691=CARTESIAN_POINT('Ctrl Pts',(-0.410503962208501,-0.454227892750445,
0.7));
#38692=CARTESIAN_POINT('Ctrl Pts',(-0.430465714824907,-0.437752457865635,
0.7));
#38693=CARTESIAN_POINT('Ctrl Pts',(-0.449338856342161,-0.420064848170144,
0.7));
#38694=CARTESIAN_POINT('Ctrl Pts',(-0.457610580625059,-0.412312719013964,
0.7));
#38695=CARTESIAN_POINT('Ctrl Pts',(-0.465673023775416,-0.404327425803387,
0.7));
#38696=CARTESIAN_POINT('Ctrl Pts',(-0.473518124711072,-0.396119066458196,
0.7));
#38697=CARTESIAN_POINT('Ctrl Pts',(-0.479686699886945,-0.389664862477052,
0.7));
#38698=CARTESIAN_POINT('Ctrl Pts',(-0.485715597961141,-0.383078107397374,
0.7));
#38699=CARTESIAN_POINT('Ctrl Pts',(-0.491596494353867,-0.376370061034681,
0.7));
#38700=CARTESIAN_POINT('Ctrl Pts',(-0.510513872818444,-0.354791947201907,
0.7));
#38701=CARTESIAN_POINT('Ctrl Pts',(-0.52791835675801,-0.331943614932878,
0.7));
#38702=CARTESIAN_POINT('Ctrl Pts',(-0.543691212400513,-0.30799896208282,
0.7));
#38703=CARTESIAN_POINT('Ctrl Pts',(-0.550562789889049,-0.297567272271884,
0.7));
#38704=CARTESIAN_POINT('Ctrl Pts',(-0.557124381433215,-0.286927116134095,
0.7));
#38705=CARTESIAN_POINT('Ctrl Pts',(-0.563364546006299,-0.276091296564536,
0.7));
#38706=CARTESIAN_POINT('Ctrl Pts',(-0.568428809706163,-0.267297386233855,
0.7));
#38707=CARTESIAN_POINT('Ctrl Pts',(-0.573283304388212,-0.258370224031322,
0.7));
#38708=CARTESIAN_POINT('Ctrl Pts',(-0.577908406198614,-0.249343210279803,
0.7));
#38709=CARTESIAN_POINT('Ctrl Pts',(-0.580665693855551,-0.243961691209221,
0.7));
#38710=CARTESIAN_POINT('Ctrl Pts',(-0.58334242566026,-0.238543142886124,
0.7));
#38711=CARTESIAN_POINT('Ctrl Pts',(-0.585937631284055,-0.233089224075231,
0.7));
#38712=CARTESIAN_POINT('Ctrl Pts',(-0.599348617917031,-0.204905548916861,
0.7));
#38713=CARTESIAN_POINT('Ctrl Pts',(-0.610585988612837,-0.175780088337437,
0.7));
#38714=CARTESIAN_POINT('Ctrl Pts',(-0.619650220520174,-0.145982170082658,
0.7));
#38715=CARTESIAN_POINT('Ctrl Pts',(-0.625666313261402,-0.126204759095282,
0.7));
#38716=CARTESIAN_POINT('Ctrl Pts',(-0.630724246458381,-0.106130286941727,
0.7));
#38717=CARTESIAN_POINT('Ctrl Pts',(-0.634813159904227,-0.0858312982855508,
0.7));
#38718=CARTESIAN_POINT('Ctrl Pts',(-0.638007544190021,-0.0699731072918824,
0.7));
#38719=CARTESIAN_POINT('Ctrl Pts',(-0.64061034690479,-0.0539777735229824,
0.7));
#38720=CARTESIAN_POINT('Ctrl Pts',(-0.642612357401729,-0.0378788650432131,
0.7));
#38721=CARTESIAN_POINT('Ctrl Pts',(-0.643611959428883,-0.0298406946260486,
0.7));
#38722=CARTESIAN_POINT('Ctrl Pts',(-0.644461654683445,-0.0217750894774087,
0.7));
#38723=CARTESIAN_POINT('Ctrl Pts',(-0.64515871908081,-0.013707778299405,
0.7));
#38724=CARTESIAN_POINT('Ctrl Pts',(-0.647813160179314,0.0170127726658416,
0.7));
#38725=CARTESIAN_POINT('Ctrl Pts',(-0.648267403763968,0.047826312089933,
0.7));
#38726=CARTESIAN_POINT('Ctrl Pts',(-0.646505170576517,0.0784946399697625,
0.7));
#38727=CARTESIAN_POINT('Ctrl Pts',(-0.644925352961593,0.105988370623497,
0.7));
#38728=CARTESIAN_POINT('Ctrl Pts',(-0.641563835892215,0.133366243242613,
0.7));
#38729=CARTESIAN_POINT('Ctrl Pts',(-0.636488118893852,0.160474361536191,
0.7));
#38730=CARTESIAN_POINT('Ctrl Pts',(-0.633437102007,0.176769069596382,0.7));
#38731=CARTESIAN_POINT('Ctrl Pts',(-0.629766130645052,0.192966361518495,
0.7));
#38732=CARTESIAN_POINT('Ctrl Pts',(-0.625484875914611,0.209032279224361,
0.7));
#38733=CARTESIAN_POINT('Ctrl Pts',(-0.62304510995881,0.218187791226195,
0.7));
#38734=CARTESIAN_POINT('Ctrl Pts',(-0.620405409729918,0.227305241293198,
0.7));
#38735=CARTESIAN_POINT('Ctrl Pts',(-0.617576713553974,0.236349483890122,
0.7));
#38736=CARTESIAN_POINT('Ctrl Pts',(-0.607811223479739,0.26757286590631,
0.7));
#38737=CARTESIAN_POINT('Ctrl Pts',(-0.595783965556306,0.297983461557127,
0.7));
#38738=CARTESIAN_POINT('Ctrl Pts',(-0.581617391728963,0.327334207529254,
0.7));
#38739=CARTESIAN_POINT('Ctrl Pts',(-0.57115026730193,0.349020319772111,
0.7));
#38740=CARTESIAN_POINT('Ctrl Pts',(-0.559514084397962,0.370128096695649,
0.7));
#38741=CARTESIAN_POINT('Ctrl Pts',(-0.546740333913183,0.39055431750125,
0.7));
#38742=CARTESIAN_POINT('Ctrl Pts',(-0.538417752622244,0.403862772470983,
0.7));
#38743=CARTESIAN_POINT('Ctrl Pts',(-0.529611960051848,0.416881820243619,
0.7));
#38744=CARTESIAN_POINT('Ctrl Pts',(-0.520343957444037,0.429592821067772,
0.7));
#38745=CARTESIAN_POINT('Ctrl Pts',(-0.514967230973053,0.436966963857323,
0.7));
#38746=CARTESIAN_POINT('Ctrl Pts',(-0.509434897530512,0.444237402262534,
0.7));
#38747=CARTESIAN_POINT('Ctrl Pts',(-0.503750712659283,0.451400231561865,
0.7));
#38748=CARTESIAN_POINT('Ctrl Pts',(-0.499397667086255,0.456885648218461,
0.7));
#38749=CARTESIAN_POINT('Ctrl Pts',(-0.494961350852985,0.462300618792668,
0.7));
#38750=CARTESIAN_POINT('Ctrl Pts',(-0.490445443674977,0.467642281239387,
0.7));
#38751=CARTESIAN_POINT('Ctrl Pts',(-0.469115242788121,0.492872811577385,
0.7));
#38752=CARTESIAN_POINT('Ctrl Pts',(-0.446004140490849,0.516481055544471,
0.7));
#38753=CARTESIAN_POINT('Ctrl Pts',(-0.421338470315635,0.538318276477707,
0.7));
#38754=CARTESIAN_POINT('Ctrl Pts',(-0.396566506146609,0.560249602513714,
0.7));
#38755=CARTESIAN_POINT('Ctrl Pts',(-0.370225710165849,0.580395556122258,
0.7));
#38756=CARTESIAN_POINT('Ctrl Pts',(-0.342503869424491,0.598574832510096,
0.7));
#38757=CARTESIAN_POINT('Ctrl Pts',(-0.32927347105657,0.607250990449811,
0.7));
#38758=CARTESIAN_POINT('Ctrl Pts',(-0.315727980106861,0.615478656494124,
0.7));
#38759=CARTESIAN_POINT('Ctrl Pts',(-0.301885354887798,0.623234692956248,
0.7));
#38760=CARTESIAN_POINT('Ctrl Pts',(-0.352210602859808,-0.494214587872355,
0.7));
#38761=CARTESIAN_POINT('Ctrl Pts',(-0.282018959374219,-0.544135188072469,
0.703388933339203));
#38762=CARTESIAN_POINT('Ctrl Pts',(-0.106195501050124,-0.620012906324691,
0.71075232338332));
#38763=CARTESIAN_POINT('Ctrl Pts',(0.190680748588941,-0.603244694242624,
0.72209017013235));
#38764=CARTESIAN_POINT('Ctrl Pts',(0.456305609272025,-0.438231596848221,
0.734013540247088));
#38765=CARTESIAN_POINT('Ctrl Pts',(0.61045325274331,-0.166159471325954,
0.74593691036183));
#38766=CARTESIAN_POINT('Ctrl Pts',(0.615465575874622,0.146507028070995,
0.75786028047657));
#38767=CARTESIAN_POINT('Ctrl Pts',(0.470117741946454,0.423380863786649,
0.76978365059131));
#38768=CARTESIAN_POINT('Ctrl Pts',(0.209918811260263,0.596821791269607,
0.78170702070605));
#38769=CARTESIAN_POINT('Ctrl Pts',(-0.101563929551992,0.624457254778657,
0.79363039082079));
#38770=CARTESIAN_POINT('Ctrl Pts',(-0.388234290052265,0.499536043242417,
0.805553760935531));
#38771=CARTESIAN_POINT('Ctrl Pts',(-0.568693105522331,0.267208012438397,
0.816770719631062));
#38772=CARTESIAN_POINT('Ctrl Pts',(-0.606782841646979,0.0830496507577644,
0.824013221621682));
#38773=CARTESIAN_POINT('Ctrl Pts',(-0.606867041669442,-1.46440865504086E-5,
0.827281266907388));
#38774=CARTESIAN_POINT('Origin',(0.,0.,0.422718733092612));
#38775=CARTESIAN_POINT('',(0.352184336898731,-0.494199469185471,0.7));
#38776=CARTESIAN_POINT('Origin',(0.,0.,0.7));
#38777=CARTESIAN_POINT('Ctrl Pts',(0.352184336898731,-0.494199469185471,
0.7));
#38778=CARTESIAN_POINT('Ctrl Pts',(0.434459481514031,-0.435567238565425,
0.703974456704914));
#38779=CARTESIAN_POINT('Ctrl Pts',(0.569074170603496,-0.276472369691842,
0.71192337011474));
#38780=CARTESIAN_POINT('Ctrl Pts',(0.63195675641648,0.0298991715734713,
0.72384674022948));
#38781=CARTESIAN_POINT('Ctrl Pts',(0.540450411763527,0.328891738414737,
0.73577011034422));
#38782=CARTESIAN_POINT('Ctrl Pts',(0.316910788923287,0.547571327639118,
0.747693480458961));
#38783=CARTESIAN_POINT('Ctrl Pts',(0.0159487222523762,0.632459517004967,
0.759616850573701));
#38784=CARTESIAN_POINT('Ctrl Pts',(-0.288909559125321,0.562845076658027,
0.771540220688441));
#38785=CARTESIAN_POINT('Ctrl Pts',(-0.523186437261898,0.355721357715825,
0.783463590803182));
#38786=CARTESIAN_POINT('Ctrl Pts',(-0.601100288213809,0.140537724272643,
0.792189761604571));
#38787=CARTESIAN_POINT('Ctrl Pts',(-0.606881754382541,0.0197715030368324,
0.796941475701048));
#38788=CARTESIAN_POINT('Ctrl Pts',(-0.606861373480359,1.53279143725385E-5,
0.797718733092612));
#38789=CARTESIAN_POINT('Ctrl Pts',(0.401891164706881,-0.563950123442266,
0.650549949443909));
#38790=CARTESIAN_POINT('Ctrl Pts',(0.495778513551069,-0.497042617955932,
0.654524406148822));
#38791=CARTESIAN_POINT('Ctrl Pts',(0.649392540401945,-0.31549331138107,
0.662473319558649));
#38792=CARTESIAN_POINT('Ctrl Pts',(0.721150290546943,0.034119100790357,
0.674396689673389));
#38793=CARTESIAN_POINT('Ctrl Pts',(0.616728862398028,0.375311079924535,
0.686320059788129));
#38794=CARTESIAN_POINT('Ctrl Pts',(0.361639155193832,0.624854814847309,
0.698243429902869));
#38795=CARTESIAN_POINT('Ctrl Pts',(0.0181997036496196,0.721724010094651,
0.710166800017609));
#38796=CARTESIAN_POINT('Ctrl Pts',(-0.329685869150999,0.642284280441105,
0.72209017013235));
#38797=CARTESIAN_POINT('Ctrl Pts',(-0.597028273550075,0.405927395926852,
0.734013540247089));
#38798=CARTESIAN_POINT('Ctrl Pts',(-0.718514881844642,0.0704038725978844,
0.745936910361831));
#38799=CARTESIAN_POINT('Ctrl Pts',(-0.664466203491914,-0.282320840499199,
0.757860280476569));
#38800=CARTESIAN_POINT('Ctrl Pts',(-0.448086466848367,-0.566073079281933,
0.769783650591311));
#38801=CARTESIAN_POINT('Ctrl Pts',(-0.122237890431146,-0.711532329868227,
0.781707020706049));
#38802=CARTESIAN_POINT('Ctrl Pts',(0.233473764593078,-0.683161969529758,
0.79363039082079));
#38803=CARTESIAN_POINT('Ctrl Pts',(0.532147090286164,-0.487893211791223,
0.80555376093553));
#38804=CARTESIAN_POINT('Ctrl Pts',(0.700815314941263,-0.17343066321587,
0.81747713105027));
#38805=CARTESIAN_POINT('Ctrl Pts',(0.698272293749139,0.183401486010904,
0.829400501165011));
#38806=CARTESIAN_POINT('Ctrl Pts',(0.525139294646749,0.495428122667492,
0.841323871279751));
#38807=CARTESIAN_POINT('Ctrl Pts',(0.223713219070008,0.686420204386435,
0.853247241394491));
#38808=CARTESIAN_POINT('Ctrl Pts',(-0.132366654812752,0.70971781110012,
0.865170611509231));
#38809=CARTESIAN_POINT('Ctrl Pts',(-0.456108965071534,0.559629264828852,
0.877093981623971));
#38810=CARTESIAN_POINT('Ctrl Pts',(-0.668422511745348,0.272821641522934,
0.889017351738711));
#38811=CARTESIAN_POINT('Ctrl Pts',(-0.717438470051463,-0.0806371127090915,
0.900940721853451));
#38812=CARTESIAN_POINT('Ctrl Pts',(-0.591182096999562,-0.414395982628671,
0.912864091968191));
#38813=CARTESIAN_POINT('Ctrl Pts',(-0.320498196401073,-0.646916693528293,
0.924787462082932));
#38814=CARTESIAN_POINT('Ctrl Pts',(0.0284843575647898,-0.721393750746014,
0.936710832197671));
#38815=CARTESIAN_POINT('Ctrl Pts',(0.370508099080321,-0.619632189906009,
0.948634202312412));
#38816=CARTESIAN_POINT('Ctrl Pts',(0.622015620706852,-0.366492660014364,
0.960557572427151));
#38817=CARTESIAN_POINT('Ctrl Pts',(0.721562894127873,-0.0238178938298552,
0.972480942541893));
#38818=CARTESIAN_POINT('Ctrl Pts',(0.644830227243077,0.324675653972579,
0.984404312656631));
#38819=CARTESIAN_POINT('Ctrl Pts',(0.410563636578539,0.593849983217877,
0.996327682771373));
#38820=CARTESIAN_POINT('Ctrl Pts',(0.0759951402356486,0.717945012455233,
1.00825105288611));
#38821=CARTESIAN_POINT('Ctrl Pts',(-0.277139192700696,0.666643960535019,
1.02017442300085));
#38822=CARTESIAN_POINT('Ctrl Pts',(-0.562567604582521,0.452479825542494,
1.03209779311559));
#38823=CARTESIAN_POINT('Ctrl Pts',(-0.710559093694536,0.127773536448902,
1.04402116323033));
#38824=CARTESIAN_POINT('Ctrl Pts',(-0.68495890335684,-0.228148203939579,
1.05594453334507));
#38825=CARTESIAN_POINT('Ctrl Pts',(-0.492021235470988,-0.528332666124543,
1.06786790345981));
#38826=CARTESIAN_POINT('Ctrl Pts',(-0.178881330574504,-0.699443901839566,
1.07979127357455));
#38827=CARTESIAN_POINT('Ctrl Pts',(0.177959810253215,-0.699678932213415,
1.09171464368929));
#38828=CARTESIAN_POINT('Ctrl Pts',(0.49132484527841,-0.528980338633497,
1.10363801380403));
#38829=CARTESIAN_POINT('Ctrl Pts',(0.684657773468146,-0.229050290282077,
1.11556138391877));
#38830=CARTESIAN_POINT('Ctrl Pts',(0.710726791028474,0.126837418623334,
1.12748475403351));
#38831=CARTESIAN_POINT('Ctrl Pts',(0.563163160186478,0.451738372575811,
1.13940812414825));
#38832=CARTESIAN_POINT('Ctrl Pts',(0.278017110586494,0.666278311570923,
1.15133149426299));
#38833=CARTESIAN_POINT('Ctrl Pts',(-0.0750493379933025,0.718044496612453,
1.16325486437773));
#38834=CARTESIAN_POINT('Ctrl Pts',(-0.409781012253192,0.594390296224132,
1.17517823449247));
#38835=CARTESIAN_POINT('Ctrl Pts',(-0.644401978262523,0.325524795768324,
1.18710160460721));
#38836=CARTESIAN_POINT('Ctrl Pts',(-0.721593642979431,-0.0228673710849739,
1.19902497472196));
#38837=CARTESIAN_POINT('Ctrl Pts',(-0.622497855355482,-0.365672971829322,
1.21094834483669));
#38838=CARTESIAN_POINT('Ctrl Pts',(-0.371324008181069,-0.619143588513205,
1.22287171495144));
#38839=CARTESIAN_POINT('Ctrl Pts',(-0.0294346121210613,-0.72135560291575,
1.23479508506617));
#38840=CARTESIAN_POINT('Ctrl Pts',(0.319645746375974,-0.647338318866116,
1.24671845518092));
#38841=CARTESIAN_POINT('Ctrl Pts',(0.590635707558052,-0.41517437686599,
1.25864182529565));
#38842=CARTESIAN_POINT('Ctrl Pts',(0.717331625742423,-0.0815821117549382,
1.2705651954104));
#38843=CARTESIAN_POINT('Ctrl Pts',(0.668781314950164,0.271940903547428,
1.28248856552513));
#38844=CARTESIAN_POINT('Ctrl Pts',(0.456845759106501,0.559027955146312,
1.29441193563988));
#38845=CARTESIAN_POINT('Ctrl Pts',(0.133301438732876,0.709542830758235,
1.30633530575461));
#38846=CARTESIAN_POINT('Ctrl Pts',(-0.222808815745382,0.686714302949052,
1.31825867586936));
#38847=CARTESIAN_POINT('Ctrl Pts',(-0.524486220282421,0.496119448301036,
1.33018204598409));
#38848=CARTESIAN_POINT('Ctrl Pts',(-0.698030096397969,0.18432115117724,
1.34210541609884));
#38849=CARTESIAN_POINT('Ctrl Pts',(-0.701043164005901,-0.172507346073306,
1.35402878621357));
#38850=CARTESIAN_POINT('Ctrl Pts',(-0.532789321814994,-0.487191790580056,
1.36595215632832));
#38851=CARTESIAN_POINT('Ctrl Pts',(-0.23437347904248,-0.682853845687445,
1.37787552644306));
#38852=CARTESIAN_POINT('Ctrl Pts',(0.12130049497697,-0.711692695035662,
1.3897988965578));
#38853=CARTESIAN_POINT('Ctrl Pts',(0.44734040079856,-0.566662922787304,
1.40172226667254));
#38854=CARTESIAN_POINT('Ctrl Pts',(0.664093729121677,-0.283195729470173,
1.41364563678728));
#38855=CARTESIAN_POINT('Ctrl Pts',(0.718607003417866,0.0694570146743853,
1.42556900690202));
#38856=CARTESIAN_POINT('Ctrl Pts',(0.597562470215061,0.405141205554568,
1.43749237701676));
#38857=CARTESIAN_POINT('Ctrl Pts',(0.330531665495144,0.641848206632094,
1.4494157471315));
#38858=CARTESIAN_POINT('Ctrl Pts',(-0.0172489986427966,0.721749800337417,
1.46133911724624));
#38859=CARTESIAN_POINT('Ctrl Pts',(-0.360815681609231,0.625325792021076,
1.47326248736098));
#38860=CARTESIAN_POINT('Ctrl Pts',(-0.616234030819248,0.376132850854382,
1.48518585747572));
#38861=CARTESIAN_POINT('Ctrl Pts',(-0.72110459126874,0.0350495464590682,
1.49710922759046));
#38862=CARTESIAN_POINT('Ctrl Pts',(-0.649807176137898,-0.314596465541046,
1.5090325977052));
#38863=CARTESIAN_POINT('Ctrl Pts',(-0.419759953978916,-0.587385634066009,
1.52095596781994));
#38864=CARTESIAN_POINT('Ctrl Pts',(-0.0871641386632488,-0.716674762797015,
1.53287933793468));
#38865=CARTESIAN_POINT('Ctrl Pts',(0.266726132357388,-0.670878134756418,
1.54480270804942));
#38866=CARTESIAN_POINT('Ctrl Pts',(0.555454423837073,-0.461184005090966,
1.55672607816416));
#38867=CARTESIAN_POINT('Ctrl Pts',(0.70848356315327,-0.138821259288117,
1.5686494482789));
#38868=CARTESIAN_POINT('Ctrl Pts',(0.688428082041725,0.217455918420426,
1.58057281839364));
#38869=CARTESIAN_POINT('Ctrl Pts',(0.500187591224132,0.520607995902278,
1.59249618850838));
#38870=CARTESIAN_POINT('Ctrl Pts',(0.189749801791051,0.696573964547411,
1.60441955862312));
#38871=CARTESIAN_POINT('Ctrl Pts',(-0.167044429389013,0.702364945676295,
1.61634292873786));
#38872=CARTESIAN_POINT('Ctrl Pts',(-0.483029201952088,0.536565935297714,
1.6282662988526));
#38873=CARTESIAN_POINT('Ctrl Pts',(-0.681008542672965,0.239682617996334,
1.64018966896734));
#38874=CARTESIAN_POINT('Ctrl Pts',(-0.712615441052988,-0.115756528463215,
1.65211303908208));
#38875=CARTESIAN_POINT('Ctrl Pts',(-0.570128386861848,-0.442914701355064,
1.66403640919682));
#38876=CARTESIAN_POINT('Ctrl Pts',(-0.288357092310038,-0.66187012059323,
1.67595977931156));
#38877=CARTESIAN_POINT('Ctrl Pts',(0.0638602987601055,-0.719123520824002,
1.6878831494263));
#38878=CARTESIAN_POINT('Ctrl Pts',(0.400477207465661,-0.600703274926714,
1.69980651954104));
#38879=CARTESIAN_POINT('Ctrl Pts',(0.639254813111137,-0.335508837950853,
1.71172988965578));
#38880=CARTESIAN_POINT('Ctrl Pts',(0.721863601446102,0.0116101465083443,
1.72365325977052));
#38881=CARTESIAN_POINT('Ctrl Pts',(0.628113563405619,0.355977601151784,
1.73557662988526));
#38882=CARTESIAN_POINT('Ctrl Pts',(0.463312679049696,0.527436308946575,
1.74352554329509));
#38883=CARTESIAN_POINT('Ctrl Pts',(0.365377360036757,0.58826493586867,1.7475));
#38884=CARTESIAN_POINT('Ctrl Pts',(0.385322222104164,-0.540699905356667,
0.667033299629272));
#38885=CARTESIAN_POINT('Ctrl Pts',(0.475338836205389,-0.476550824825763,
0.671007756334186));
#38886=CARTESIAN_POINT('Ctrl Pts',(0.622619750469128,-0.302486330817994,
0.678956669744013));
#38887=CARTESIAN_POINT('Ctrl Pts',(0.691419112503455,0.0327124577180616,
0.690880039858753));
#38888=CARTESIAN_POINT('Ctrl Pts',(0.591302712186528,0.359837966087936,
0.702803409973493));
#38889=CARTESIAN_POINT('Ctrl Pts',(0.346729699770317,0.599093652444579,
0.714726780088233));
#38890=CARTESIAN_POINT('Ctrl Pts',(0.0174493765172051,0.691969179064757,
0.726650150202973));
#38891=CARTESIAN_POINT('Ctrl Pts',(-0.316093765809106,0.615804545846745,
0.738573520317714));
#38892=CARTESIAN_POINT('Ctrl Pts',(-0.572414328120683,0.38919204985651,
0.750496890432453));
#38893=CARTESIAN_POINT('Ctrl Pts',(-0.688892354946931,0.0675013013882525,
0.762420260547194));
#38894=CARTESIAN_POINT('Ctrl Pts',(-0.637071965066363,-0.270681475883673,
0.774343630661933));
#38895=CARTESIAN_POINT('Ctrl Pts',(-0.429613010345087,-0.542735337168578,
0.786267000776674));
#38896=CARTESIAN_POINT('Ctrl Pts',(-0.117198335526006,-0.682197675690988,
0.798190370891414));
#38897=CARTESIAN_POINT('Ctrl Pts',(0.223848239713465,-0.654996952591022,
0.810113741006154));
#38898=CARTESIAN_POINT('Ctrl Pts',(0.510208029740792,-0.467778625225678,
0.822037111120894));
#38899=CARTESIAN_POINT('Ctrl Pts',(0.671922495819859,-0.166280561504948,
0.833960481235634));
#38900=CARTESIAN_POINT('Ctrl Pts',(0.669484316873271,0.175840312833126,
0.845883851350375));
#38901=CARTESIAN_POINT('Ctrl Pts',(0.503489147553371,0.475002891039828,
0.857807221465114));
#38902=CARTESIAN_POINT('Ctrl Pts',(0.214490096464305,0.658120858775991,
0.869730591579855));
#38903=CARTESIAN_POINT('Ctrl Pts',(-0.126909516913974,0.680457964880758,
0.881653961694594));
#38904=CARTESIAN_POINT('Ctrl Pts',(-0.437304761529596,0.53655718466876,
0.893577331809335));
#38905=CARTESIAN_POINT('Ctrl Pts',(-0.640865164871226,0.261573904533071,
0.905500701924074));
#38906=CARTESIAN_POINT('Ctrl Pts',(-0.687860320852951,-0.0773126512392803,
0.917424072038815));
#38907=CARTESIAN_POINT('Ctrl Pts',(-0.566809174444562,-0.3973114984351,
0.929347442153555));
#38908=CARTESIAN_POINT('Ctrl Pts',(-0.307284877257029,-0.620245976416043,
0.941270812268296));
#38909=CARTESIAN_POINT('Ctrl Pts',(0.0273100205128412,-0.69165253546255,
0.953194182383035));
#38910=CARTESIAN_POINT('Ctrl Pts',(0.355232999833039,-0.594086342943096,
0.965117552497776));
#38911=CARTESIAN_POINT('Ctrl Pts',(0.596371511001176,-0.35138310702749,
0.977040922612515));
#38912=CARTESIAN_POINT('Ctrl Pts',(0.691814705496321,-0.0228359431167249,
0.988964292727256));
#38913=CARTESIAN_POINT('Ctrl Pts',(0.618245529787783,0.311290108960425,
1.000887662842));
#38914=CARTESIAN_POINT('Ctrl Pts',(0.393637150189633,0.56936707055236,1.01281103295674));
#38915=CARTESIAN_POINT('Ctrl Pts',(0.0728620553927195,0.688345979811773,
1.02473440307148));
#38916=CARTESIAN_POINT('Ctrl Pts',(-0.265713454142422,0.639159938768556,
1.03665777318622));
#38917=CARTESIAN_POINT('Ctrl Pts',(-0.53937438420587,0.433825242121212,
1.04858114330096));
#38918=CARTESIAN_POINT('Ctrl Pts',(-0.681264563550163,0.122505761047289,
1.0605045134157));
#38919=CARTESIAN_POINT('Ctrl Pts',(-0.656719803442273,-0.218742238275356,
1.07242788353044));
#38920=CARTESIAN_POINT('Ctrl Pts',(-0.471736461069982,-0.506550864510311,
1.08435125364518));
#38921=CARTESIAN_POINT('Ctrl Pts',(-0.17150651181941,-0.67060762256517,
1.09627462375992));
#38922=CARTESIAN_POINT('Ctrl Pts',(0.170622983418949,-0.670832963239128,
1.10819799387466));
#38923=CARTESIAN_POINT('Ctrl Pts',(0.471068781260073,-0.50717183514182,
1.1201213639894));
#38924=CARTESIAN_POINT('Ctrl Pts',(0.656431088367041,-0.219607133910158,
1.13204473410414));
#38925=CARTESIAN_POINT('Ctrl Pts',(0.681425347152859,0.121608236960235,
1.14396810421888));
#38926=CARTESIAN_POINT('Ctrl Pts',(0.53994538657879,0.43311435735987,1.15589147433362));
#38927=CARTESIAN_POINT('Ctrl Pts',(0.266555177724046,0.638809364574028,
1.16781484444836));
#38928=CARTESIAN_POINT('Ctrl Pts',(-0.0719552461525682,0.688441362492184,
1.1797382145631));
#38929=CARTESIAN_POINT('Ctrl Pts',(-0.392886791459217,0.569885107838286,
1.19166158467784));
#38930=CARTESIAN_POINT('Ctrl Pts',(-0.617834936415022,0.312104242816431,
1.20358495479258));
#38931=CARTESIAN_POINT('Ctrl Pts',(-0.691844186651542,-0.0219246079882583,
1.21550832490732));
#38932=CARTESIAN_POINT('Ctrl Pts',(-0.596833864351296,-0.350597212485312,
1.22743169502206));
#38933=CARTESIAN_POINT('Ctrl Pts',(-0.356015271092881,-0.593617885333347,
1.2393550651368));
#38934=CARTESIAN_POINT('Ctrl Pts',(-0.0282210985094273,-0.691615960369548,
1.25127843525154));
#38935=CARTESIAN_POINT('Ctrl Pts',(0.306467571561485,-0.620650219221889,
1.26320180536628));
#38936=CARTESIAN_POINT('Ctrl Pts',(0.566285311239232,-0.398057801473175,
1.27512517548102));
#38937=CARTESIAN_POINT('Ctrl Pts',(0.687757881460913,-0.0782186903966656,
1.28704854559576));
#38938=CARTESIAN_POINT('Ctrl Pts',(0.641209175539583,0.260729477126809,
1.2989719157105));
#38939=CARTESIAN_POINT('Ctrl Pts',(0.438011179435034,0.535980665443169,
1.31089528582524));
#38940=CARTESIAN_POINT('Ctrl Pts',(0.127805762089087,0.680290198529863,
1.32281865593998));
#38941=CARTESIAN_POINT('Ctrl Pts',(-0.213622979370609,0.658402832408697,
1.33474202605472));
#38942=CARTESIAN_POINT('Ctrl Pts',(-0.502862997771139,0.475665715089492,
1.34666539616946));
#38943=CARTESIAN_POINT('Ctrl Pts',(-0.669252104698097,0.176722062561917,
1.3585887662842));
#38944=CARTESIAN_POINT('Ctrl Pts',(-0.672140951251578,-0.165395310361548,
1.37051213639894));
#38945=CARTESIAN_POINT('Ctrl Pts',(-0.510823783709841,-0.467106121813182,
1.38243550651368));
#38946=CARTESIAN_POINT('Ctrl Pts',(-0.224710861242244,-0.654701531904951,
1.39435887662842));
#38947=CARTESIAN_POINT('Ctrl Pts',(0.116299586483697,-0.682351429413614,
1.40628224674316));
#38948=CARTESIAN_POINT('Ctrl Pts',(0.428897702686216,-0.543300862938094,
1.4182056168579));
#38949=CARTESIAN_POINT('Ctrl Pts',(0.636714846859693,-0.271520295424869,
1.43012898697264));
#38950=CARTESIAN_POINT('Ctrl Pts',(0.688980678583815,0.0665934799899764,
1.44205235708738));
#38951=CARTESIAN_POINT('Ctrl Pts',(0.572926501226411,0.388438272098131,
1.45397572720212));
#38952=CARTESIAN_POINT('Ctrl Pts',(0.316904692137907,0.615386450243146,
1.46589909731686));
#38953=CARTESIAN_POINT('Ctrl Pts',(-0.0165378666409895,0.691993906041918,
1.4778224674316));
#38954=CARTESIAN_POINT('Ctrl Pts',(-0.345940175890901,0.599545212436668,
1.48974583754634));
#38955=CARTESIAN_POINT('Ctrl Pts',(-0.5908282812454,0.360625857508688,1.50166920766108));
#38956=CARTESIAN_POINT('Ctrl Pts',(-0.691375297289357,0.0336045434967476,
1.51359257777582));
#38957=CARTESIAN_POINT('Ctrl Pts',(-0.623017291836473,-0.301626459633181,
1.52551594789056));
#38958=CARTESIAN_POINT('Ctrl Pts',(-0.402454326995381,-0.563169229946753,
1.5374393180053));
#38959=CARTESIAN_POINT('Ctrl Pts',(-0.0835705846432688,-0.687128099291087,
1.54936268812004));
#38960=CARTESIAN_POINT('Ctrl Pts',(0.255729697586553,-0.643219548839746,
1.56128605823478));
#38961=CARTESIAN_POINT('Ctrl Pts',(0.532554461670217,-0.442170570657251,
1.57320942834952));
#38962=CARTESIAN_POINT('Ctrl Pts',(0.67927460181316,-0.133098014591112,
1.58513279846426));
#38963=CARTESIAN_POINT('Ctrl Pts',(0.660045956782098,0.208490768281939,
1.597056168579));
#38964=CARTESIAN_POINT('Ctrl Pts',(0.479566138907238,0.499144662641613,
1.60897953869374));
#38965=CARTESIAN_POINT('Ctrl Pts',(0.181926903825513,0.667856005431414,
1.62090290880848));
#38966=CARTESIAN_POINT('Ctrl Pts',(-0.160157615729726,0.673408239251661,
1.63282627892322));
#38967=CARTESIAN_POINT('Ctrl Pts',(-0.463115146044895,0.514444697098797,
1.64474964903796));
#38968=CARTESIAN_POINT('Ctrl Pts',(-0.652932306003921,0.229801118005293,
1.6566730191527));
#38969=CARTESIAN_POINT('Ctrl Pts',(-0.683236132977807,-0.110984183499136,
1.66859638926744));
#38970=CARTESIAN_POINT('Ctrl Pts',(-0.546623454811443,-0.424654463486924,
1.68051975938218));
#38971=CARTESIAN_POINT('Ctrl Pts',(-0.276468868504331,-0.634582912011373,
1.69244312949692));
#38972=CARTESIAN_POINT('Ctrl Pts',(0.0612275023274693,-0.689475901301222,
1.70436649961166));
#38973=CARTESIAN_POINT('Ctrl Pts',(0.383966558695777,-0.575937818610241,
1.7162898697264));
#38974=CARTESIAN_POINT('Ctrl Pts',(0.612899975689733,-0.321676668530641,
1.72821323984114));
#38975=CARTESIAN_POINT('Ctrl Pts',(0.692103015422583,0.0111314899266652,
1.74013660995588));
#38976=CARTESIAN_POINT('Ctrl Pts',(0.602218051152578,0.341301557089859,
1.75205998007063));
#38977=CARTESIAN_POINT('Ctrl Pts',(0.444211484844831,0.505691461841269,
1.76000889348045));
#38978=CARTESIAN_POINT('Ctrl Pts',(0.350313788009248,0.564012280389897,
1.76398335018536));
#38979=CARTESIAN_POINT('Ctrl Pts',(0.368753279501448,-0.517449687271069,
0.683516649814636));
#38980=CARTESIAN_POINT('Ctrl Pts',(0.45489915885971,-0.456059031695594,
0.68749110651955));
#38981=CARTESIAN_POINT('Ctrl Pts',(0.595846960536312,-0.289479350254918,
0.695440019929377));
#38982=CARTESIAN_POINT('Ctrl Pts',(0.661687934459967,0.0313058146457665,
0.707363390044116));
#38983=CARTESIAN_POINT('Ctrl Pts',(0.565876561975028,0.344364852251337,
0.719286760158857));
#38984=CARTESIAN_POINT('Ctrl Pts',(0.331820244346802,0.573332490041849,
0.731210130273597));
#38985=CARTESIAN_POINT('Ctrl Pts',(0.0166990493847907,0.662214348034862,
0.743133500388337));
#38986=CARTESIAN_POINT('Ctrl Pts',(-0.302501662467213,0.589324811252386,
0.755056870503077));
#38987=CARTESIAN_POINT('Ctrl Pts',(-0.54780038269129,0.372456703786168,
0.766980240617817));
#38988=CARTESIAN_POINT('Ctrl Pts',(-0.659269828049221,0.0645987301786208,
0.778903610732558));
#38989=CARTESIAN_POINT('Ctrl Pts',(-0.609677726640811,-0.259042111268147,
0.790826980847297));
#38990=CARTESIAN_POINT('Ctrl Pts',(-0.411139553841808,-0.519397595055222,
0.802750350962038));
#38991=CARTESIAN_POINT('Ctrl Pts',(-0.112158780620866,-0.65286302151375,
0.814673721076777));
#38992=CARTESIAN_POINT('Ctrl Pts',(0.214222714833852,-0.626831935652286,
0.826597091191518));
#38993=CARTESIAN_POINT('Ctrl Pts',(0.48826896919542,-0.447664038660134,
0.838520461306257));
#38994=CARTESIAN_POINT('Ctrl Pts',(0.643029676698454,-0.159130459794026,
0.850443831420999));
#38995=CARTESIAN_POINT('Ctrl Pts',(0.640696339997405,0.168279139655349,
0.862367201535737));
#38996=CARTESIAN_POINT('Ctrl Pts',(0.481839000459992,0.454577659412166,
0.874290571650479));
#38997=CARTESIAN_POINT('Ctrl Pts',(0.205266973858603,0.629821513165547,
0.886213941765218));
#38998=CARTESIAN_POINT('Ctrl Pts',(-0.121452379015197,0.651198118661396,
0.898137311879959));
#38999=CARTESIAN_POINT('Ctrl Pts',(-0.418500557987658,0.513485104508667,
0.910060681994699));
#39000=CARTESIAN_POINT('Ctrl Pts',(-0.613307817997104,0.250326167543209,
0.921984052109438));
#39001=CARTESIAN_POINT('Ctrl Pts',(-0.658282171654439,-0.0739881897694695,
0.933907422224179));
#39002=CARTESIAN_POINT('Ctrl Pts',(-0.542436251889562,-0.380227014241528,
0.945830792338918));
#39003=CARTESIAN_POINT('Ctrl Pts',(-0.294071558112983,-0.593575259303795,
0.957754162453659));
#39004=CARTESIAN_POINT('Ctrl Pts',(0.0261356834608925,-0.661911320179086,
0.969677532568399));
#39005=CARTESIAN_POINT('Ctrl Pts',(0.339957900585757,-0.568540495980184,
0.981600902683139));
#39006=CARTESIAN_POINT('Ctrl Pts',(0.5707274012955,-0.336273554040615,0.993524272797879));
#39007=CARTESIAN_POINT('Ctrl Pts',(0.662066516864767,-0.0218539924035951,
1.00544764291262));
#39008=CARTESIAN_POINT('Ctrl Pts',(0.591660832332492,0.297904563948271,
1.01737101302736));
#39009=CARTESIAN_POINT('Ctrl Pts',(0.376710663800726,0.544884157886843,
1.0292943831421));
#39010=CARTESIAN_POINT('Ctrl Pts',(0.0697289705497912,0.658746947168312,
1.04121775325684));
#39011=CARTESIAN_POINT('Ctrl Pts',(-0.254287715584149,0.611675917002094,
1.05314112337158));
#39012=CARTESIAN_POINT('Ctrl Pts',(-0.516181163829219,0.415170658699929,
1.06506449348632));
#39013=CARTESIAN_POINT('Ctrl Pts',(-0.651970033405789,0.117237985645677,
1.07698786360106));
#39014=CARTESIAN_POINT('Ctrl Pts',(-0.628480703527705,-0.209336272611132,
1.0889112337158));
#39015=CARTESIAN_POINT('Ctrl Pts',(-0.451451686668976,-0.484769062896079,
1.10083460383054));
#39016=CARTESIAN_POINT('Ctrl Pts',(-0.164131693064316,-0.641771343290773,
1.11275797394528));
#39017=CARTESIAN_POINT('Ctrl Pts',(0.163286156584683,-0.641986994264843,
1.12468134406002));
#39018=CARTESIAN_POINT('Ctrl Pts',(0.450812717241737,-0.485363331650142,
1.13660471417476));
#39019=CARTESIAN_POINT('Ctrl Pts',(0.628204403265935,-0.210163977538239,
1.1485280842895));
#39020=CARTESIAN_POINT('Ctrl Pts',(0.652123903277245,0.116379055297137,
1.16045145440424));
#39021=CARTESIAN_POINT('Ctrl Pts',(0.516727612971101,0.414490342143929,
1.17237482451898));
#39022=CARTESIAN_POINT('Ctrl Pts',(0.2550932448616,0.611340417577134,1.18429819463372));
#39023=CARTESIAN_POINT('Ctrl Pts',(-0.0688611543118346,0.658838228371917,
1.19622156474846));
#39024=CARTESIAN_POINT('Ctrl Pts',(-0.37599257066524,0.545379919452438,
1.2081449348632));
#39025=CARTESIAN_POINT('Ctrl Pts',(-0.591267894567521,0.298683689864538,
1.22006830497794));
#39026=CARTESIAN_POINT('Ctrl Pts',(-0.662094730323653,-0.0209818448915428,
1.23199167509268));
#39027=CARTESIAN_POINT('Ctrl Pts',(-0.57116987334711,-0.335521453141302,
1.24391504520742));
#39028=CARTESIAN_POINT('Ctrl Pts',(-0.340706534004693,-0.568092182153489,
1.25583841532216));
#39029=CARTESIAN_POINT('Ctrl Pts',(-0.0270075848977933,-0.661876317823347,
1.2677617854369));
#39030=CARTESIAN_POINT('Ctrl Pts',(0.293289396746996,-0.59396211957766,
1.27968515555164));
#39031=CARTESIAN_POINT('Ctrl Pts',(0.541934914920413,-0.38094122608036,
1.29160852566638));
#39032=CARTESIAN_POINT('Ctrl Pts',(0.658184137179402,-0.0748552690383927,
1.30353189578112));
#39033=CARTESIAN_POINT('Ctrl Pts',(0.613637036129002,0.24951805070619,1.31545526589586));
#39034=CARTESIAN_POINT('Ctrl Pts',(0.419176599763568,0.512933375740025,
1.3273786360106));
#39035=CARTESIAN_POINT('Ctrl Pts',(0.122310085445297,0.651037566301491,
1.33930200612534));
#39036=CARTESIAN_POINT('Ctrl Pts',(-0.204437142995836,0.630091361868343,
1.35122537624008));
#39037=CARTESIAN_POINT('Ctrl Pts',(-0.481239775259857,0.455211981877947,
1.36314874635482));
#39038=CARTESIAN_POINT('Ctrl Pts',(-0.640474112998224,0.169122973946595,
1.37507211646956));
#39039=CARTESIAN_POINT('Ctrl Pts',(-0.643238738497255,-0.15828327464979,
1.3869954865843));
#39040=CARTESIAN_POINT('Ctrl Pts',(-0.488858245604688,-0.447020453046308,
1.39891885669904));
#39041=CARTESIAN_POINT('Ctrl Pts',(-0.215048243442008,-0.626549218122459,
1.41084222681378));
#39042=CARTESIAN_POINT('Ctrl Pts',(0.111298677990423,-0.653010163791566,
1.42276559692852));
#39043=CARTESIAN_POINT('Ctrl Pts',(0.410455004573871,-0.519938803088884,
1.43468896704326));
#39044=CARTESIAN_POINT('Ctrl Pts',(0.60933596459771,-0.259844861379564,
1.44661233715801));
#39045=CARTESIAN_POINT('Ctrl Pts',(0.659354353749764,0.0637299453055676,
1.45853570727274));
#39046=CARTESIAN_POINT('Ctrl Pts',(0.548290532237762,0.371735338641693,
1.47045907738748));
#39047=CARTESIAN_POINT('Ctrl Pts',(0.303277718780669,0.5889246938542,1.48238244750222));
#39048=CARTESIAN_POINT('Ctrl Pts',(-0.0158267346391821,0.662238011746418,
1.49430581761697));
#39049=CARTESIAN_POINT('Ctrl Pts',(-0.331064670172572,0.573764632852262,
1.5062291877317));
#39050=CARTESIAN_POINT('Ctrl Pts',(-0.565422531671553,0.345118864162994,
1.51815255784645));
#39051=CARTESIAN_POINT('Ctrl Pts',(-0.661646003309974,0.032159540534428,
1.53007592796118));
#39052=CARTESIAN_POINT('Ctrl Pts',(-0.596227407535047,-0.288656453725316,
1.54199929807593));
#39053=CARTESIAN_POINT('Ctrl Pts',(-0.385148700011845,-0.538952825827497,
1.55392266819066));
#39054=CARTESIAN_POINT('Ctrl Pts',(-0.0799770306232885,-0.657581435785161,
1.56584603830541));
#39055=CARTESIAN_POINT('Ctrl Pts',(0.244733262815717,-0.615560962923072,
1.57776940842015));
#39056=CARTESIAN_POINT('Ctrl Pts',(0.509654499503361,-0.423157136223537,
1.58969277853489));
#39057=CARTESIAN_POINT('Ctrl Pts',(0.65006564047305,-0.127374769894107,
1.60161614864963));
#39058=CARTESIAN_POINT('Ctrl Pts',(0.631663831522472,0.199525618143451,
1.61353951876437));
#39059=CARTESIAN_POINT('Ctrl Pts',(0.458944686590344,0.477681329380949,
1.62546288887911));
#39060=CARTESIAN_POINT('Ctrl Pts',(0.174104005859975,0.639138046315416,
1.63738625899385));
#39061=CARTESIAN_POINT('Ctrl Pts',(-0.15327080207044,0.644451532827028,
1.64930962910859));
#39062=CARTESIAN_POINT('Ctrl Pts',(-0.4432010901377,0.49232345889988,1.66123299922333));
#39063=CARTESIAN_POINT('Ctrl Pts',(-0.624856069334877,0.219919618014252,
1.67315636933807));
#39064=CARTESIAN_POINT('Ctrl Pts',(-0.653856824902625,-0.106211838535058,
1.68507973945281));
#39065=CARTESIAN_POINT('Ctrl Pts',(-0.523118522761037,-0.406394225618784,
1.69700310956755));
#39066=CARTESIAN_POINT('Ctrl Pts',(-0.264580644698625,-0.607295703429515,
1.70892647968229));
#39067=CARTESIAN_POINT('Ctrl Pts',(0.058594705894833,-0.659828281778441,
1.72084984979703));
#39068=CARTESIAN_POINT('Ctrl Pts',(0.367455909925893,-0.551172362293768,
1.73277321991177));
#39069=CARTESIAN_POINT('Ctrl Pts',(0.586545138268328,-0.307844499110428,
1.74469659002651));
#39070=CARTESIAN_POINT('Ctrl Pts',(0.662342429399066,0.0106528333449858,
1.75661996014125));
#39071=CARTESIAN_POINT('Ctrl Pts',(0.576322538899538,0.326625513027934,
1.76854333025599));
#39072=CARTESIAN_POINT('Ctrl Pts',(0.425110290639966,0.483946614735963,
1.77649224366581));
#39073=CARTESIAN_POINT('Ctrl Pts',(0.33525021598174,0.539759624911124,1.78046670037073));
#39074=CARTESIAN_POINT('Ctrl Pts',(0.352184336898731,-0.494199469185471,
0.7));
#39075=CARTESIAN_POINT('Ctrl Pts',(0.434459481514031,-0.435567238565425,
0.703974456704914));
#39076=CARTESIAN_POINT('Ctrl Pts',(0.569074170603496,-0.276472369691842,
0.71192337011474));
#39077=CARTESIAN_POINT('Ctrl Pts',(0.63195675641648,0.0298991715734713,
0.72384674022948));
#39078=CARTESIAN_POINT('Ctrl Pts',(0.540450411763527,0.328891738414737,
0.73577011034422));
#39079=CARTESIAN_POINT('Ctrl Pts',(0.316910788923287,0.547571327639118,
0.747693480458961));
#39080=CARTESIAN_POINT('Ctrl Pts',(0.0159487222523762,0.632459517004967,
0.759616850573701));
#39081=CARTESIAN_POINT('Ctrl Pts',(-0.288909559125321,0.562845076658027,
0.771540220688441));
#39082=CARTESIAN_POINT('Ctrl Pts',(-0.523186437261898,0.355721357715825,
0.783463590803182));
#39083=CARTESIAN_POINT('Ctrl Pts',(-0.629647301151511,0.0616961589689892,
0.795386960917921));
#39084=CARTESIAN_POINT('Ctrl Pts',(-0.58228348821526,-0.247402746652621,
0.807310331032662));
#39085=CARTESIAN_POINT('Ctrl Pts',(-0.392666097338528,-0.496059852941866,
0.819233701147401));
#39086=CARTESIAN_POINT('Ctrl Pts',(-0.107119225715726,-0.623528367336511,
0.831157071262142));
#39087=CARTESIAN_POINT('Ctrl Pts',(0.204597189954239,-0.59866691871355,
0.843080441376881));
#39088=CARTESIAN_POINT('Ctrl Pts',(0.466329908650049,-0.427549452094589,
0.855003811491622));
#39089=CARTESIAN_POINT('Ctrl Pts',(0.614136857577049,-0.151980358083104,
0.866927181606362));
#39090=CARTESIAN_POINT('Ctrl Pts',(0.611908363121538,0.160717966477571,
0.878850551721102));
#39091=CARTESIAN_POINT('Ctrl Pts',(0.460188853366613,0.434152427784503,
0.890773921835841));
#39092=CARTESIAN_POINT('Ctrl Pts',(0.1960438512529,0.601522167555102,0.902697291950583));
#39093=CARTESIAN_POINT('Ctrl Pts',(-0.115995241116418,0.621938272442033,
0.914620662065322));
#39094=CARTESIAN_POINT('Ctrl Pts',(-0.399696354445721,0.490413024348575,
0.926544032180063));
#39095=CARTESIAN_POINT('Ctrl Pts',(-0.585750471122982,0.239078430553345,
0.938467402294802));
#39096=CARTESIAN_POINT('Ctrl Pts',(-0.628704022455928,-0.070663728299658,
0.950390772409543));
#39097=CARTESIAN_POINT('Ctrl Pts',(-0.518063329334561,-0.363142530047957,
0.962314142524282));
#39098=CARTESIAN_POINT('Ctrl Pts',(-0.280858238968939,-0.566904542191545,
0.974237512639023));
#39099=CARTESIAN_POINT('Ctrl Pts',(0.0249613464089441,-0.632170104895623,
0.986160882753763));
#39100=CARTESIAN_POINT('Ctrl Pts',(0.324682801338475,-0.542994649017271,
0.998084252868503));
#39101=CARTESIAN_POINT('Ctrl Pts',(0.545083291589825,-0.321164001053741,
1.01000762298324));
#39102=CARTESIAN_POINT('Ctrl Pts',(0.632318328233213,-0.0208720416904643,
1.02193099309798));
#39103=CARTESIAN_POINT('Ctrl Pts',(0.565076134877199,0.284519018936116,
1.03385436321272));
#39104=CARTESIAN_POINT('Ctrl Pts',(0.35978417741182,0.520401245221327,1.04577773332746));
#39105=CARTESIAN_POINT('Ctrl Pts',(0.0665958857068623,0.62914791452485,
1.0577011034422));
#39106=CARTESIAN_POINT('Ctrl Pts',(-0.242861977025874,0.584191895235632,
1.06962447355694));
#39107=CARTESIAN_POINT('Ctrl Pts',(-0.492987943452569,0.396516075278645,
1.08154784367169));
#39108=CARTESIAN_POINT('Ctrl Pts',(-0.622675503261414,0.111970210244065,
1.09347121378642));
#39109=CARTESIAN_POINT('Ctrl Pts',(-0.600241603613138,-0.199930306946909,
1.10539458390116));
#39110=CARTESIAN_POINT('Ctrl Pts',(-0.431166912267969,-0.462987261281848,
1.1173179540159));
#39111=CARTESIAN_POINT('Ctrl Pts',(-0.156756874309222,-0.612935064016377,
1.12924132413064));
#39112=CARTESIAN_POINT('Ctrl Pts',(0.155949329750418,-0.613141025290557,
1.14116469424539));
#39113=CARTESIAN_POINT('Ctrl Pts',(0.4305566532234,-0.463554828158465,1.15308806436012));
#39114=CARTESIAN_POINT('Ctrl Pts',(0.59997771816483,-0.200720821166321,
1.16501143447486));
#39115=CARTESIAN_POINT('Ctrl Pts',(0.622822459401631,0.111149873634038,
1.17693480458961));
#39116=CARTESIAN_POINT('Ctrl Pts',(0.493509839363413,0.395866326927988,
1.18885817470434));
#39117=CARTESIAN_POINT('Ctrl Pts',(0.243631311999152,0.583871470580239,
1.20078154481908));
#39118=CARTESIAN_POINT('Ctrl Pts',(-0.0657670624710998,0.629235094251649,
1.21270491493383));
#39119=CARTESIAN_POINT('Ctrl Pts',(-0.359098349871265,0.520874731066591,
1.22462828504856));
#39120=CARTESIAN_POINT('Ctrl Pts',(-0.564700852720018,0.285263136912645,
1.23655165516331));
#39121=CARTESIAN_POINT('Ctrl Pts',(-0.632345273995765,-0.020039081794827,
1.24847502527805));
#39122=CARTESIAN_POINT('Ctrl Pts',(-0.545505882342923,-0.320445693797292,
1.26039839539279));
#39123=CARTESIAN_POINT('Ctrl Pts',(-0.325397796916506,-0.542566478973631,
1.27232176550753));
#39124=CARTESIAN_POINT('Ctrl Pts',(-0.0257940712861588,-0.632136675277145,
1.28424513562227));
#39125=CARTESIAN_POINT('Ctrl Pts',(0.280111221932506,-0.567274019933433,
1.29616850573701));
#39126=CARTESIAN_POINT('Ctrl Pts',(0.517584518601595,-0.363824650687545,
1.30809187585175));
#39127=CARTESIAN_POINT('Ctrl Pts',(0.628610392897891,-0.0714918476801203,
1.32001524596649));
#39128=CARTESIAN_POINT('Ctrl Pts',(0.586064896718421,0.238306624285571,
1.33193861608123));
#39129=CARTESIAN_POINT('Ctrl Pts',(0.4003420200921,0.489886086036881,1.34386198619597));
#39130=CARTESIAN_POINT('Ctrl Pts',(0.116814408801508,0.621784934073119,
1.35578535631071));
#39131=CARTESIAN_POINT('Ctrl Pts',(-0.195251306621063,0.601779891327988,
1.36770872642545));
#39132=CARTESIAN_POINT('Ctrl Pts',(-0.459616552748575,0.434758248666402,
1.37963209654019));
#39133=CARTESIAN_POINT('Ctrl Pts',(-0.611696121298351,0.161523885331273,
1.39155546665493));
#39134=CARTESIAN_POINT('Ctrl Pts',(-0.614336525742933,-0.151171238938032,
1.40347883676967));
#39135=CARTESIAN_POINT('Ctrl Pts',(-0.466892707499535,-0.426934784279433,
1.41540220688441));
#39136=CARTESIAN_POINT('Ctrl Pts',(-0.205385625641773,-0.598396904339966,
1.42732557699915));
#39137=CARTESIAN_POINT('Ctrl Pts',(0.106297769497149,-0.623668898169518,
1.43924894711389));
#39138=CARTESIAN_POINT('Ctrl Pts',(0.392012306461527,-0.496576743239674,
1.45117231722863));
#39139=CARTESIAN_POINT('Ctrl Pts',(0.581957082335726,-0.248169427334259,
1.46309568734337));
#39140=CARTESIAN_POINT('Ctrl Pts',(0.629728028915714,0.0608664106211582,
1.47501905745811));
#39141=CARTESIAN_POINT('Ctrl Pts',(0.523654563249111,0.355032405185257,
1.48694242757285));
#39142=CARTESIAN_POINT('Ctrl Pts',(0.289650745423433,0.562462937465252,
1.49886579768759));
#39143=CARTESIAN_POINT('Ctrl Pts',(-0.0151156026373754,0.632482117450919,
1.51078916780233));
#39144=CARTESIAN_POINT('Ctrl Pts',(-0.316189164454242,0.547984053267855,
1.52271253791707));
#39145=CARTESIAN_POINT('Ctrl Pts',(-0.540016782097706,0.329611870817301,
1.53463590803181));
#39146=CARTESIAN_POINT('Ctrl Pts',(-0.631916709330591,0.0307145375721074,
1.54655927814655));
#39147=CARTESIAN_POINT('Ctrl Pts',(-0.569437523233623,-0.275686447817451,
1.55848264826129));
#39148=CARTESIAN_POINT('Ctrl Pts',(-0.367843073028309,-0.514736421708243,
1.57040601837603));
#39149=CARTESIAN_POINT('Ctrl Pts',(-0.0763834766033089,-0.628034772279233,
1.58232938849077));
#39150=CARTESIAN_POINT('Ctrl Pts',(0.233736828044883,-0.5879023770064,1.59425275860551));
#39151=CARTESIAN_POINT('Ctrl Pts',(0.486754537336504,-0.404143701789823,
1.60617612872025));
#39152=CARTESIAN_POINT('Ctrl Pts',(0.620856679132942,-0.121651525197101,
1.61809949883499));
#39153=CARTESIAN_POINT('Ctrl Pts',(0.603281706262845,0.190560468004963,
1.63002286894973));
#39154=CARTESIAN_POINT('Ctrl Pts',(0.43832323427345,0.456217996120286,1.64194623906447));
#39155=CARTESIAN_POINT('Ctrl Pts',(0.166281107894437,0.610420087199418,
1.65386960917921));
#39156=CARTESIAN_POINT('Ctrl Pts',(-0.146383988411153,0.615494826402396,
1.66579297929395));
#39157=CARTESIAN_POINT('Ctrl Pts',(-0.423287034230507,0.470202220700963,
1.67771634940869));
#39158=CARTESIAN_POINT('Ctrl Pts',(-0.596779832665833,0.210038118023212,
1.68963971952343));
#39159=CARTESIAN_POINT('Ctrl Pts',(-0.624477516827445,-0.101439493570979,
1.70156308963817));
#39160=CARTESIAN_POINT('Ctrl Pts',(-0.499613590710631,-0.388133987750645,
1.71348645975291));
#39161=CARTESIAN_POINT('Ctrl Pts',(-0.252692420892918,-0.580008494847657,
1.72540982986765));
#39162=CARTESIAN_POINT('Ctrl Pts',(0.0559619094621963,-0.630180662255662,
1.73733319998239));
#39163=CARTESIAN_POINT('Ctrl Pts',(0.350945261156011,-0.526406905977294,
1.74925657009713));
#39164=CARTESIAN_POINT('Ctrl Pts',(0.560190300846922,-0.294012329690215,
1.76117994021187));
#39165=CARTESIAN_POINT('Ctrl Pts',(0.632581843375548,0.0101741767633066,
1.77310331032661));
#39166=CARTESIAN_POINT('Ctrl Pts',(0.550427026646497,0.311949468966009,
1.78502668044135));
#39167=CARTESIAN_POINT('Ctrl Pts',(0.406009096435101,0.462201767630657,
1.79297559385118));
#39168=CARTESIAN_POINT('Ctrl Pts',(0.320186643954231,0.515506969432351,
1.79695005055609));
#39169=CARTESIAN_POINT('Ctrl Pts',(0.301912013981581,0.623256720988311,
0.7));
#39170=CARTESIAN_POINT('Ctrl Pts',(0.316742913732564,0.614965173301012,
0.7));
#39171=CARTESIAN_POINT('Ctrl Pts',(0.3312465938099,0.606134971871919,0.7));
#39172=CARTESIAN_POINT('Ctrl Pts',(0.345390045352,0.596775580586543,0.7));
#39173=CARTESIAN_POINT('Ctrl Pts',(0.368996263743943,0.581154228610288,
0.7));
#39174=CARTESIAN_POINT('Ctrl Pts',(0.391600130077927,0.564059572920914,
0.7));
#39175=CARTESIAN_POINT('Ctrl Pts',(0.413087355494181,0.545611767070564,
0.7));
#39176=CARTESIAN_POINT('Ctrl Pts',(0.421816954375618,0.538116990886276,
0.7));
#39177=CARTESIAN_POINT('Ctrl Pts',(0.430362017243965,0.530398662168233,
0.7));
#39178=CARTESIAN_POINT('Ctrl Pts',(0.438713852739663,0.522464087423267,
0.7));
#39179=CARTESIAN_POINT('Ctrl Pts',(0.445012055142894,0.51648054551166,0.7));
#39180=CARTESIAN_POINT('Ctrl Pts',(0.451200223788741,0.510373897616862,
0.7));
#39181=CARTESIAN_POINT('Ctrl Pts',(0.457264688892812,0.504157868673923,
0.7));
#39182=CARTESIAN_POINT('Ctrl Pts',(0.479903218716829,0.480953553998711,
0.7));
#39183=CARTESIAN_POINT('Ctrl Pts',(0.500858312621123,0.456192563010338,
0.7));
#39184=CARTESIAN_POINT('Ctrl Pts',(0.519950046261114,0.430052281971842,
0.7));
#39185=CARTESIAN_POINT('Ctrl Pts',(0.532066948364594,0.413461896191609,
0.7));
#39186=CARTESIAN_POINT('Ctrl Pts',(0.543432537348295,0.396315311298811,
0.7));
#39187=CARTESIAN_POINT('Ctrl Pts',(0.553991354258157,0.378653559125833,
0.7));
#39188=CARTESIAN_POINT('Ctrl Pts',(0.557760895560471,0.372348240560731,
0.7));
#39189=CARTESIAN_POINT('Ctrl Pts',(0.561422494384538,0.365985667439434,
0.7));
#39190=CARTESIAN_POINT('Ctrl Pts',(0.564974116622367,0.359568344749639,
0.7));
#39191=CARTESIAN_POINT('Ctrl Pts',(0.567149078484655,0.355638469562003,
0.7));
#39192=CARTESIAN_POINT('Ctrl Pts',(0.569282819078203,0.351688020934708,
0.7));
#39193=CARTESIAN_POINT('Ctrl Pts',(0.571374893992065,0.347717486836035,
0.7));
#39194=CARTESIAN_POINT('Ctrl Pts',(0.586516887221463,0.318979605586734,
0.7));
#39195=CARTESIAN_POINT('Ctrl Pts',(0.599480260131589,0.289191109124012,
0.7));
#39196=CARTESIAN_POINT('Ctrl Pts',(0.610215113049288,0.258612759249907,
0.7));
#39197=CARTESIAN_POINT('Ctrl Pts',(0.620862381399234,0.228283895007034,
0.7));
#39198=CARTESIAN_POINT('Ctrl Pts',(0.62931749648762,0.197176730970088,0.7));
#39199=CARTESIAN_POINT('Ctrl Pts',(0.635481674913492,0.165538333607963,
0.7));
#39200=CARTESIAN_POINT('Ctrl Pts',(0.637058860844219,0.157443234514,0.7));
#39201=CARTESIAN_POINT('Ctrl Pts',(0.638485804480818,0.149313374621512,
0.7));
#39202=CARTESIAN_POINT('Ctrl Pts',(0.639760298594453,0.141152968773294,
0.7));
#39203=CARTESIAN_POINT('Ctrl Pts',(0.640724273662108,0.134980772530509,
0.7));
#39204=CARTESIAN_POINT('Ctrl Pts',(0.641600510210609,0.128793923527105,
0.7));
#39205=CARTESIAN_POINT('Ctrl Pts',(0.642387398557739,0.122602557207706,
0.7));
#39206=CARTESIAN_POINT('Ctrl Pts',(0.646272029071298,0.0920376484596141,
0.7));
#39207=CARTESIAN_POINT('Ctrl Pts',(0.647992252287009,0.0613038392021154,
0.7));
#39208=CARTESIAN_POINT('Ctrl Pts',(0.647486512817817,0.0306206514007389,
0.7));
#39209=CARTESIAN_POINT('Ctrl Pts',(0.647048570692616,0.00405072500145474,
0.7));
#39210=CARTESIAN_POINT('Ctrl Pts',(0.644940626982976,-0.022481795837132,
0.7));
#39211=CARTESIAN_POINT('Ctrl Pts',(0.641195095628098,-0.0488246644619669,
0.7));
#39212=CARTESIAN_POINT('Ctrl Pts',(0.639088886165721,-0.0636379429815907,
0.7));
#39213=CARTESIAN_POINT('Ctrl Pts',(0.636464411497198,-0.0783911345254818,
0.7));
#39214=CARTESIAN_POINT('Ctrl Pts',(0.633324220155005,-0.0930556586801398,
0.7));
#39215=CARTESIAN_POINT('Ctrl Pts',(0.631822561842711,-0.100068321984061,
0.7));
#39216=CARTESIAN_POINT('Ctrl Pts',(0.630202465201574,-0.107062563306399,
0.7));
#39217=CARTESIAN_POINT('Ctrl Pts',(0.628465525090794,-0.114029195569243,
0.7));
#39218=CARTESIAN_POINT('Ctrl Pts',(0.620900031829999,-0.144373367546085,
0.7));
#39219=CARTESIAN_POINT('Ctrl Pts',(0.61115833403686,-0.174053594627863,
0.7));
#39220=CARTESIAN_POINT('Ctrl Pts',(0.599311626004954,-0.202827697227785,
0.7));
#39221=CARTESIAN_POINT('Ctrl Pts',(0.589222460913586,-0.227332958158054,
0.7));
#39222=CARTESIAN_POINT('Ctrl Pts',(0.577605524722755,-0.251181291846326,
0.7));
#39223=CARTESIAN_POINT('Ctrl Pts',(0.564478637188341,-0.274208720129379,
0.7));
#39224=CARTESIAN_POINT('Ctrl Pts',(0.556929094299622,-0.28745226754182,
0.7));
#39225=CARTESIAN_POINT('Ctrl Pts',(0.548879654511669,-0.300423975832763,
0.7));
#39226=CARTESIAN_POINT('Ctrl Pts',(0.540348752462322,-0.313098885409112,
0.7));
#39227=CARTESIAN_POINT('Ctrl Pts',(0.536443758105698,-0.318900786553921,
0.7));
#39228=CARTESIAN_POINT('Ctrl Pts',(0.532437857208379,-0.324640465844469,
0.7));
#39229=CARTESIAN_POINT('Ctrl Pts',(0.528332704252445,-0.330315351774545,
0.7));
#39230=CARTESIAN_POINT('Ctrl Pts',(0.524569485757922,-0.335517553961799,
0.7));
#39231=CARTESIAN_POINT('Ctrl Pts',(0.520725138073348,-0.340662013706015,
0.7));
#39232=CARTESIAN_POINT('Ctrl Pts',(0.516806355023409,-0.345740598709291,
0.7));
#39233=CARTESIAN_POINT('Ctrl Pts',(0.498042718044497,-0.37005751652629,
0.7));
#39234=CARTESIAN_POINT('Ctrl Pts',(0.477542558449122,-0.392913064495779,
0.7));
#39235=CARTESIAN_POINT('Ctrl Pts',(0.455486881988334,-0.414130436631542,
0.7));
#39236=CARTESIAN_POINT('Ctrl Pts',(0.433826821014111,-0.434967230052523,
0.7));
#39237=CARTESIAN_POINT('Ctrl Pts',(0.410665525050054,-0.454224782213852,
0.7));
#39238=CARTESIAN_POINT('Ctrl Pts',(0.386146686004952,-0.471694960933986,
0.7));
#39239=CARTESIAN_POINT('Ctrl Pts',(0.375097833815722,-0.479567496091263,
0.7));
#39240=CARTESIAN_POINT('Ctrl Pts',(0.363773025729378,-0.487076461755432,
0.7));
#39241=CARTESIAN_POINT('Ctrl Pts',(0.352184336898733,-0.494199469185469,
0.7));
#39242=CARTESIAN_POINT('Ctrl Pts',(0.365377360036757,0.58826493586867,1.7475));
#39243=CARTESIAN_POINT('Ctrl Pts',(0.463312679049696,0.527436308946575,
1.74352554329509));
#39244=CARTESIAN_POINT('Ctrl Pts',(0.545713121227658,0.441706955049179,
1.73955108659017));
#39245=CARTESIAN_POINT('Ctrl Pts',(0.602538348656719,0.341447702326575,
1.73557662988526));
#39246=CARTESIAN_POINT('Ctrl Pts',(0.65936357608578,0.241188449603971,1.73160217318035));
#39247=CARTESIAN_POINT('Ctrl Pts',(0.690613588765941,0.126399298056159,
1.72762771647543));
#39248=CARTESIAN_POINT('Ctrl Pts',(0.69247046371686,0.0111515582057199,
1.72365325977052));
#39249=CARTESIAN_POINT('Ctrl Pts',(0.69432733866778,-0.10409618164472,1.71967880306561));
#39250=CARTESIAN_POINT('Ctrl Pts',(0.666791075889459,-0.219802509797787,
1.71570434636069));
#39251=CARTESIAN_POINT('Ctrl Pts',(0.613226676892718,-0.32185474670363,
1.71172988965578));
#39252=CARTESIAN_POINT('Ctrl Pts',(0.559662277895978,-0.423906983609474,
1.70775543295087));
#39253=CARTESIAN_POINT('Ctrl Pts',(0.480069742680819,-0.512305129268094,
1.70378097624595));
#39254=CARTESIAN_POINT('Ctrl Pts',(0.384170656955648,-0.576240909746952,
1.69980651954104));
#39255=CARTESIAN_POINT('Ctrl Pts',(0.288271571230476,-0.64017669022581,
1.69583206283613));
#39256=CARTESIAN_POINT('Ctrl Pts',(0.176065934995291,-0.679650105524906,
1.69185760613121));
#39257=CARTESIAN_POINT('Ctrl Pts',(0.0612602183660074,-0.689844579802659,
1.6878831494263));
#39258=CARTESIAN_POINT('Ctrl Pts',(-0.0535454982632758,-0.700039054080412,
1.68390869272139));
#39259=CARTESIAN_POINT('Ctrl Pts',(-0.170951295286657,-0.680954587336821,
1.67993423601647));
#39260=CARTESIAN_POINT('Ctrl Pts',(-0.276616076223649,-0.634919784091998,
1.67595977931156));
#39261=CARTESIAN_POINT('Ctrl Pts',(-0.382280857160642,-0.588884980847175,
1.67198532260665));
#39262=CARTESIAN_POINT('Ctrl Pts',(-0.476204622011245,-0.515899841101119,
1.66801086590173));
#39263=CARTESIAN_POINT('Ctrl Pts',(-0.546914346801737,-0.42488090907945,
1.66403640919682));
#39264=CARTESIAN_POINT('Ctrl Pts',(-0.617624071592228,-0.333861977057781,
1.66006195249191));
#39265=CARTESIAN_POINT('Ctrl Pts',(-0.665119756322608,-0.224809252760498,
1.65608749578699));
#39266=CARTESIAN_POINT('Ctrl Pts',(-0.683599782291128,-0.111043032868598,
1.65211303908208));
#39267=CARTESIAN_POINT('Ctrl Pts',(-0.689558148768936,-0.0743623035197568,
1.65083158690023));
#39268=CARTESIAN_POINT('Ctrl Pts',(-0.692500165449594,-0.0371915783518519,
1.64955013471837));
#39269=CARTESIAN_POINT('Ctrl Pts',(-0.692468966846601,-1.59520066716212E-5,
1.64826868253652));
#39270=CARTESIAN_POINT('Origin',(0.,0.,0.895));
#39271=CARTESIAN_POINT('Origin',(0.,0.,1.7475));
#39272=CARTESIAN_POINT('Ctrl Pts',(0.6516,1.70379184550113E-15,-0.72625));
#39273=CARTESIAN_POINT('Ctrl Pts',(0.6516,0.10591743302354,-0.722791509249761));
#39274=CARTESIAN_POINT('Ctrl Pts',(0.598993916001074,0.317654812761972,
-0.715874527749282));
#39275=CARTESIAN_POINT('Ctrl Pts',(0.380287460438119,0.561300167265437,
-0.705499055498563));
#39276=CARTESIAN_POINT('Ctrl Pts',(0.0729856334338192,0.674050219639796,
-0.695123583247845));
#39277=CARTESIAN_POINT('Ctrl Pts',(-0.251359967211615,0.629681615150501,
-0.684748110997127));
#39278=CARTESIAN_POINT('Ctrl Pts',(-0.517092446119555,0.438507275576915,
-0.674372638746409));
#39279=CARTESIAN_POINT('Ctrl Pts',(-0.662284183342424,0.145110368978899,
-0.66399716649569));
#39280=CARTESIAN_POINT('Ctrl Pts',(-0.653076224636751,-0.182118205164697,
-0.653621694244972));
#39281=CARTESIAN_POINT('Ctrl Pts',(-0.491620673403516,-0.4668888850725,
-0.643246221994254));
#39282=CARTESIAN_POINT('Ctrl Pts',(-0.215554351760434,-0.64281600898939,
-0.632870749743535));
#39283=CARTESIAN_POINT('Ctrl Pts',(0.110762954559402,-0.668885305138704,
-0.622495277492817));
#39284=CARTESIAN_POINT('Ctrl Pts',(0.411258705600379,-0.539019822036371,
-0.612119805242099));
#39285=CARTESIAN_POINT('Ctrl Pts',(0.615879002840427,-0.283494407102116,
-0.60174433299138));
#39286=CARTESIAN_POINT('Ctrl Pts',(0.676921592558105,0.0381210480060534,
-0.591368860740662));
#39287=CARTESIAN_POINT('Ctrl Pts',(0.580155735567945,0.350849494573475,
-0.580993388489943));
#39288=CARTESIAN_POINT('Ctrl Pts',(0.348140170063391,0.581785587179681,
-0.570617916239225));
#39289=CARTESIAN_POINT('Ctrl Pts',(0.0349638692286564,0.677091999899065,
-0.560242443988507));
#39290=CARTESIAN_POINT('Ctrl Pts',(-0.286363435133131,0.614550266504086,
-0.549866971737789));
#39291=CARTESIAN_POINT('Ctrl Pts',(-0.540931812645454,0.408740531547555,
-0.53949149948707));
#39292=CARTESIAN_POINT('Ctrl Pts',(-0.669394604785241,0.107642512990995,
-0.529116027236352));
#39293=CARTESIAN_POINT('Ctrl Pts',(-0.641803721387148,-0.218549836322835,
-0.518740554985634));
#39294=CARTESIAN_POINT('Ctrl Pts',(-0.464591330058565,-0.493792409536047,
-0.508365082734915));
#39295=CARTESIAN_POINT('Ctrl Pts',(-0.179070350189228,-0.653918846159451,
-0.497989610484197));
#39296=CARTESIAN_POINT('Ctrl Pts',(0.148196688364544,-0.661599417513598,
-0.487614138233479));
#39297=CARTESIAN_POINT('Ctrl Pts',(0.440915139510084,-0.51504357818782,
-0.477238665982761));
#39298=CARTESIAN_POINT('Ctrl Pts',(0.630844551378487,-0.248417390064856,
-0.466863193732042));
#39299=CARTESIAN_POINT('Ctrl Pts',(0.673707329393678,0.0761214950437051,
-0.456487721481324));
#39300=CARTESIAN_POINT('Ctrl Pts',(0.559511020646667,0.382914436216214,
-0.446112249230605));
#39301=CARTESIAN_POINT('Ctrl Pts',(0.31487782023221,0.600439843792433,-0.435736776979887));
#39302=CARTESIAN_POINT('Ctrl Pts',(-0.00316177006436105,0.677986763069525,
-0.425361304729169));
#39303=CARTESIAN_POINT('Ctrl Pts',(-0.320464267714219,0.597476945836541,
-0.414985832478451));
#39304=CARTESIAN_POINT('Ctrl Pts',(-0.56305802607539,0.377679370577104,
-0.404610360227732));
#39305=CARTESIAN_POINT('Ctrl Pts',(-0.674387991520381,0.0698346946780471,
-0.394234887977014));
#39306=CARTESIAN_POINT('Ctrl Pts',(-0.628500189764246,-0.254290304876461,
-0.383859415726295));
#39307=CARTESIAN_POINT('Ctrl Pts',(-0.436092287172216,-0.519133474893842,
-0.373483943475578));
#39308=CARTESIAN_POINT('Ctrl Pts',(-0.142019680366899,-0.662952832469283,
-0.363108471224859));
#39309=CARTESIAN_POINT('Ctrl Pts',(0.185161489055837,-0.652220262374863,
-0.352732998974141));
#39310=CARTESIAN_POINT('Ctrl Pts',(0.469176593473532,-0.489437812018158,
-0.342357526723422));
#39311=CARTESIAN_POINT('Ctrl Pts',(0.643814162441103,-0.212554397554274,
-0.331982054472704));
#39312=CARTESIAN_POINT('Ctrl Pts',(0.668361536472565,0.113881096960973,
-0.321606582221986));
#39313=CARTESIAN_POINT('Ctrl Pts',(0.537096070163569,0.413767880771309,
-0.311231109971268));
#39314=CARTESIAN_POINT('Ctrl Pts',(0.280619232983065,0.617194372623894,
-0.300855637720549));
#39315=CARTESIAN_POINT('Ctrl Pts',(-0.0412774067590903,0.676736450734642,
-0.290480165469831));
#39316=CARTESIAN_POINT('Ctrl Pts',(-0.353551185726935,0.578513272200878,
-0.280104693219112));
#39317=CARTESIAN_POINT('Ctrl Pts',(-0.583402785381157,0.345423274387037,
-0.269729220968394));
#39318=CARTESIAN_POINT('Ctrl Pts',(-0.677247687787472,0.031805924735722,
-0.259353748717676));
#39319=CARTESIAN_POINT('Ctrl Pts',(-0.613208152053947,-0.289226222202328,
-0.248978276466957));
#39320=CARTESIAN_POINT('Ctrl Pts',(-0.406213495413166,-0.542832066956897,
-0.238602804216239));
#39321=CARTESIAN_POINT('Ctrl Pts',(-0.104519676240231,-0.669889291059751,
-0.228227331965521));
#39322=CARTESIAN_POINT('Ctrl Pts',(0.221540459947147,-0.640777587066391,
-0.217851859714803));
#39323=CARTESIAN_POINT('Ctrl Pts',(0.49595362168121,-0.462283450573905,
-0.207476387464084));
#39324=CARTESIAN_POINT('Ctrl Pts',(0.654746819495382,-0.176019039699093,
-0.197100915213366));
#39325=CARTESIAN_POINT('Ctrl Pts',(0.66090111234246,0.151280657145806,-0.186725442962648));
#39326=CARTESIAN_POINT('Ctrl Pts',(0.51298182194067,0.443311680645382,-0.176349970711929));
#39327=CARTESIAN_POINT('Ctrl Pts',(0.245472765512694,0.631997215248837,
-0.165974498461211));
#39328=CARTESIAN_POINT('Ctrl Pts',(-0.0792623836862046,0.673342931276607,
-0.155599026210492));
#39329=CARTESIAN_POINT('Ctrl Pts',(-0.385519630244667,0.557723394050477,
-0.145223553959774));
#39330=CARTESIAN_POINT('Ctrl Pts',(-0.601901478794571,0.312066036455591,
-0.134848081709056));
#39331=CARTESIAN_POINT('Ctrl Pts',(-0.677965082858782,-0.00630688219070944,
-0.124472609458338));
#39332=CARTESIAN_POINT('Ctrl Pts',(-0.595975637420361,-0.323282123041996,
-0.114097137207619));
#39333=CARTESIAN_POINT('Ctrl Pts',(-0.448685015420264,-0.484234261030354,
-0.10718015570714));
#39334=CARTESIAN_POINT('Ctrl Pts',(-0.360448909728228,-0.542825150002956,
-0.103721664956901));
#39335=CARTESIAN_POINT('Ctrl Pts',(0.6516,1.70379184550113E-15,-0.729109831226506));
#39336=CARTESIAN_POINT('Ctrl Pts',(0.6516,0.105917843960459,-0.725651340476266));
#39337=CARTESIAN_POINT('Ctrl Pts',(0.598993966183392,0.317654580582479,
-0.718734358975788));
#39338=CARTESIAN_POINT('Ctrl Pts',(0.380287471156537,0.561300312828727,
-0.708358886725069));
#39339=CARTESIAN_POINT('Ctrl Pts',(0.0729856416697512,0.674050196632246,
-0.697983414474351));
#39340=CARTESIAN_POINT('Ctrl Pts',(-0.251359982464231,0.629681676831451,
-0.687607942223633));
#39341=CARTESIAN_POINT('Ctrl Pts',(-0.517092471768115,0.438507283657801,
-0.677232469972914));
#39342=CARTESIAN_POINT('Ctrl Pts',(-0.662284218200291,0.145110383849344,
-0.666856997722196));
#39343=CARTESIAN_POINT('Ctrl Pts',(-0.653076258166858,-0.182118218295592,
-0.656481525471477));
#39344=CARTESIAN_POINT('Ctrl Pts',(-0.491620699001913,-0.466888907385001,
-0.64610605322076));
#39345=CARTESIAN_POINT('Ctrl Pts',(-0.215554362849302,-0.642816043209853,
-0.635730580970041));
#39346=CARTESIAN_POINT('Ctrl Pts',(0.11076296025821,-0.668885339300916,
-0.625355108719322));
#39347=CARTESIAN_POINT('Ctrl Pts',(0.411258726912751,-0.539019850182803,
-0.614979636468604));
#39348=CARTESIAN_POINT('Ctrl Pts',(0.615879034720188,-0.283494421661586,
-0.604604164217886));
#39349=CARTESIAN_POINT('Ctrl Pts',(0.676921627612323,0.0381210499198712,
-0.594228691967168));
#39350=CARTESIAN_POINT('Ctrl Pts',(0.580155765604886,0.350849512769928,
-0.583853219716449));
#39351=CARTESIAN_POINT('Ctrl Pts',(0.348140188090538,0.581785617288146,
-0.573477747465732));
#39352=CARTESIAN_POINT('Ctrl Pts',(0.0349638710384253,0.677092034965131,
-0.563102275215012));
#39353=CARTESIAN_POINT('Ctrl Pts',(-0.286363449960142,0.614550298320383,
-0.552726802964295));
#39354=CARTESIAN_POINT('Ctrl Pts',(-0.540931840653934,0.408740552713229,
-0.542351330713575));
#39355=CARTESIAN_POINT('Ctrl Pts',(-0.669394639445035,0.107642518563529,
-0.531975858462859));
#39356=CARTESIAN_POINT('Ctrl Pts',(-0.641803754618455,-0.218549847638404,
-0.521600386212139));
#39357=CARTESIAN_POINT('Ctrl Pts',(-0.464591354114125,-0.493792435103844,
-0.511224913961421));
#39358=CARTESIAN_POINT('Ctrl Pts',(-0.17907035946113,-0.653918880017893,
-0.500849441710703));
#39359=CARTESIAN_POINT('Ctrl Pts',(0.148196696037867,-0.66159945176991,
-0.490473969459984));
#39360=CARTESIAN_POINT('Ctrl Pts',(0.440915162339756,-0.51504360485568,
-0.480098497209267));
#39361=CARTESIAN_POINT('Ctrl Pts',(0.630844584042316,-0.248417402927411,
-0.469723024958547));
#39362=CARTESIAN_POINT('Ctrl Pts',(0.67370736427685,0.0761214989851266,
-0.45934755270783));
#39363=CARTESIAN_POINT('Ctrl Pts',(0.559511049616991,0.382914456042728,
-0.448972080457111));
#39364=CARTESIAN_POINT('Ctrl Pts',(0.314877836535932,0.600439874881969,
-0.438596608206393));
#39365=CARTESIAN_POINT('Ctrl Pts',(-0.00316177022807097,0.677986798174277,
-0.428221135955674));
#39366=CARTESIAN_POINT('Ctrl Pts',(-0.320464284307196,0.597476976772663,
-0.417845663704957));
#39367=CARTESIAN_POINT('Ctrl Pts',(-0.563058055229369,0.37767939013256,
-0.407470191454237));
#39368=CARTESIAN_POINT('Ctrl Pts',(-0.674388026438798,0.0698346982939447,
-0.39709471920352));
#39369=CARTESIAN_POINT('Ctrl Pts',(-0.628500222306683,-0.25429031804309,
-0.386719246952801));
#39370=CARTESIAN_POINT('Ctrl Pts',(-0.436092309752179,-0.519133501773496,
-0.376343774702083));
#39371=CARTESIAN_POINT('Ctrl Pts',(-0.142019687720371,-0.662952866795619,
-0.365968302451365));
#39372=CARTESIAN_POINT('Ctrl Pts',(0.185161498643091,-0.652220296145461,
-0.355592830200646));
#39373=CARTESIAN_POINT('Ctrl Pts',(0.469176617766576,-0.489437837360274,
-0.345217357949928));
#39374=CARTESIAN_POINT('Ctrl Pts',(0.643814195776372,-0.212554408559825,
-0.33484188569921));
#39375=CARTESIAN_POINT('Ctrl Pts',(0.668361571079138,0.113881102857349,
-0.324466413448491));
#39376=CARTESIAN_POINT('Ctrl Pts',(0.537096097972906,0.413767902195657,
-0.314090941197774));
#39377=CARTESIAN_POINT('Ctrl Pts',(0.280619247513718,0.617194404580342,
-0.303715468947054));
#39378=CARTESIAN_POINT('Ctrl Pts',(-0.0412774088978781,0.67673648577585,
-0.293339996696337));
#39379=CARTESIAN_POINT('Ctrl Pts',(-0.353551204030045,0.578513302152726,
-0.282964524445618));
#39380=CARTESIAN_POINT('Ctrl Pts',(-0.583402815594588,0.345423292277057,
-0.2725890521949));
#39381=CARTESIAN_POINT('Ctrl Pts',(-0.67724772284195,0.0318059263731912,
-0.262213579944181));
#39382=CARTESIAN_POINT('Ctrl Pts',(-0.613208183828464,-0.289226237159228,
-0.251838107693463));
#39383=CARTESIAN_POINT('Ctrl Pts',(-0.406213516398622,-0.542832095100663,
-0.241462635442745));
#39384=CARTESIAN_POINT('Ctrl Pts',(-0.104519681746337,-0.669889325671602,
-0.231087163192027));
#39385=CARTESIAN_POINT('Ctrl Pts',(0.221540471605481,-0.640777620390888,
-0.220711690941308));
#39386=CARTESIAN_POINT('Ctrl Pts',(0.495953646988114,-0.462283474219069,
-0.21033621869059));
#39387=CARTESIAN_POINT('Ctrl Pts',(0.654746854137338,-0.176019049391254,
-0.199960746439871));
#39388=CARTESIAN_POINT('Ctrl Pts',(0.66090114509062,0.151280666128215,-0.189585274189154));
#39389=CARTESIAN_POINT('Ctrl Pts',(0.51298185142758,0.443311701314457,-0.179209801938435));
#39390=CARTESIAN_POINT('Ctrl Pts',(0.245472772407152,0.631997252513665,
-0.168834329687717));
#39391=CARTESIAN_POINT('Ctrl Pts',(-0.0792623762299619,0.67334295711367,
-0.158458857436998));
#39392=CARTESIAN_POINT('Ctrl Pts',(-0.38551967319154,0.557723440877264,
-0.14808338518628));
#39393=CARTESIAN_POINT('Ctrl Pts',(-0.601901464183699,0.31206601686732,
-0.137707912935562));
#39394=CARTESIAN_POINT('Ctrl Pts',(-0.677965210051624,-0.00630681059785788,
-0.127332440684844));
#39395=CARTESIAN_POINT('Ctrl Pts',(-0.595975471759363,-0.323282293283048,
-0.116956968434125));
#39396=CARTESIAN_POINT('Ctrl Pts',(-0.448685357757425,-0.484234033710274,
-0.110039986933646));
#39397=CARTESIAN_POINT('Ctrl Pts',(-0.360448909728228,-0.542825150002956,
-0.106581496183407));
#39398=CARTESIAN_POINT('Ctrl Pts',(0.650016727545913,1.69965193344392E-15,
-0.735787069985478));
#39399=CARTESIAN_POINT('Ctrl Pts',(0.650016727545912,0.10565929404003,-0.732328579235239));
#39400=CARTESIAN_POINT('Ctrl Pts',(0.597538371946512,0.316883407693635,
-0.72541159773476));
#39401=CARTESIAN_POINT('Ctrl Pts',(0.379363409041282,0.559936031664057,
-0.715036125484042));
#39402=CARTESIAN_POINT('Ctrl Pts',(0.0728082756862247,0.672412440714268,
-0.704660653233323));
#39403=CARTESIAN_POINT('Ctrl Pts',(-0.250749178172313,0.628151483647856,
-0.694285180982604));
#39404=CARTESIAN_POINT('Ctrl Pts',(-0.515835954585742,0.437441765349259,
-0.683909708731887));
#39405=CARTESIAN_POINT('Ctrl Pts',(-0.660674884189079,0.144757748346355,
-0.673534236481169));
#39406=CARTESIAN_POINT('Ctrl Pts',(-0.651489301705309,-0.181675665347773,
-0.66315876423045));
#39407=CARTESIAN_POINT('Ctrl Pts',(-0.490426073855602,-0.465754385608829,
-0.652783291979732));
#39408=CARTESIAN_POINT('Ctrl Pts',(-0.215030571904435,-0.64125401525488,
-0.642407819729013));
#39409=CARTESIAN_POINT('Ctrl Pts',(0.110493809426251,-0.66725996774767,
-0.632032347478296));
#39410=CARTESIAN_POINT('Ctrl Pts',(0.410259379502582,-0.537710046135872,
-0.621656875227576));
#39411=CARTESIAN_POINT('Ctrl Pts',(0.614382465688009,-0.282805538385134,
-0.611281402976859));
#39412=CARTESIAN_POINT('Ctrl Pts',(0.675276726724032,0.0380284169940838,
-0.60090593072614));
#39413=CARTESIAN_POINT('Ctrl Pts',(0.57874600311102,0.349996958048548,-0.590530458475422));
#39414=CARTESIAN_POINT('Ctrl Pts',(0.347294217037289,0.580371894336871,
-0.580154986224702));
#39415=CARTESIAN_POINT('Ctrl Pts',(0.0348789097983566,0.675446719982932,
-0.569779513973986));
#39416=CARTESIAN_POINT('Ctrl Pts',(-0.285667594680009,0.613056958065561,
-0.559404041723266));
#39417=CARTESIAN_POINT('Ctrl Pts',(-0.539617391208136,0.407747324444045,
-0.549028569472549));
#39418=CARTESIAN_POINT('Ctrl Pts',(-0.667768028943849,0.10738095021671,
-0.538653097221829));
#39419=CARTESIAN_POINT('Ctrl Pts',(-0.640244189205681,-0.218018777541106,
-0.528277624971112));
#39420=CARTESIAN_POINT('Ctrl Pts',(-0.463462409944431,-0.492592533112403,
-0.517902152720393));
#39421=CARTESIAN_POINT('Ctrl Pts',(-0.178635223429194,-0.652329875185191,
-0.507526680469676));
#39422=CARTESIAN_POINT('Ctrl Pts',(0.14783658215608,-0.659991783359264,
-0.497151208218956));
#39423=CARTESIAN_POINT('Ctrl Pts',(0.439843750662663,-0.513792063108988,
-0.486775735968239));
#39424=CARTESIAN_POINT('Ctrl Pts',(0.629311649111721,-0.247813755493517,
-0.476400263717519));
#39425=CARTESIAN_POINT('Ctrl Pts',(0.672070273973121,0.0759365258431999,
-0.466024791466803));
#39426=CARTESIAN_POINT('Ctrl Pts',(0.55815145320655,0.381983984481368,-0.455649319216083));
#39427=CARTESIAN_POINT('Ctrl Pts',(0.314112692082441,0.59898082255559,-0.445273846965366));
#39428=CARTESIAN_POINT('Ctrl Pts',(-0.00315408721366853,0.676339308964272,
-0.434898374714647));
#39429=CARTESIAN_POINT('Ctrl Pts',(-0.319685564939782,0.59602512420693,
-0.424522902463929));
#39430=CARTESIAN_POINT('Ctrl Pts',(-0.561689839693175,0.376761639636888,
-0.41414743021321));
#39431=CARTESIAN_POINT('Ctrl Pts',(-0.672749282144793,0.0696650019042273,
-0.403771957962492));
#39432=CARTESIAN_POINT('Ctrl Pts',(-0.626972984110423,-0.25367239958757,
-0.393396485711774));
#39433=CARTESIAN_POINT('Ctrl Pts',(-0.435032617473759,-0.51787202169008,
-0.383021013461055));
#39434=CARTESIAN_POINT('Ctrl Pts',(-0.141674583798387,-0.661341909623961,
-0.372645541210337));
#39435=CARTESIAN_POINT('Ctrl Pts',(0.184711561311131,-0.650635418824393,
-0.362270068959619));
#39436=CARTESIAN_POINT('Ctrl Pts',(0.468036531532543,-0.488248516921783,
-0.3518945967089));
#39437=CARTESIAN_POINT('Ctrl Pts',(0.642249745047455,-0.212037907212844,
-0.341519124458182));
#39438=CARTESIAN_POINT('Ctrl Pts',(0.666737470904793,0.113604374920479,
-0.331143652207463));
#39439=CARTESIAN_POINT('Ctrl Pts',(0.535790969277522,0.412762457610684,
-0.320768179956746));
#39440=CARTESIAN_POINT('Ctrl Pts',(0.279937350483935,0.615694639210893,
-0.310392707706027));
#39441=CARTESIAN_POINT('Ctrl Pts',(-0.0411771059289157,0.675092034787015,
-0.300017235455309));
#39442=CARTESIAN_POINT('Ctrl Pts',(-0.352692084369553,0.577107530799868,
-0.28964176320459));
#39443=CARTESIAN_POINT('Ctrl Pts',(-0.581985162834664,0.344583923195399,
-0.279266290953873));
#39444=CARTESIAN_POINT('Ctrl Pts',(-0.675602029599326,0.0317286388769256,
-0.268890818703154));
#39445=CARTESIAN_POINT('Ctrl Pts',(-0.611718104794686,-0.288523425438239,
-0.258515346452436));
#39446=CARTESIAN_POINT('Ctrl Pts',(-0.405226428900723,-0.541513027982306,
-0.248139874201717));
#39447=CARTESIAN_POINT('Ctrl Pts',(-0.104265701531316,-0.668261513309247,
-0.237764401950999));
#39448=CARTESIAN_POINT('Ctrl Pts',(0.221002133831056,-0.639220548032841,
-0.22738892970028));
#39449=CARTESIAN_POINT('Ctrl Pts',(0.49474849438948,-0.46116013897505,-0.217013457449562));
#39450=CARTESIAN_POINT('Ctrl Pts',(0.653155835208594,-0.175591326286409,
-0.206637985198844));
#39451=CARTESIAN_POINT('Ctrl Pts',(0.659295177802631,0.150913054960382,
-0.196262512948126));
#39452=CARTESIAN_POINT('Ctrl Pts',(0.511735311224025,0.44223447272061,-0.185887040697407));
#39453=CARTESIAN_POINT('Ctrl Pts',(0.24487629716172,0.630461503497974,-0.175511568446689));
#39454=CARTESIAN_POINT('Ctrl Pts',(-0.0790698042728978,0.671706778414142,
-0.165136096195971));
#39455=CARTESIAN_POINT('Ctrl Pts',(-0.384582804555352,0.556368136401998,
-0.154760623945252));
#39456=CARTESIAN_POINT('Ctrl Pts',(-0.600438992610296,0.31130780842898,
-0.144385151694534));
#39457=CARTESIAN_POINT('Ctrl Pts',(-0.676317506997876,-0.00629169319767802,
-0.134009679443816));
#39458=CARTESIAN_POINT('Ctrl Pts',(-0.594527836101359,-0.322496282336175,
-0.123634207193097));
#39459=CARTESIAN_POINT('Ctrl Pts',(-0.447594141936034,-0.483058088236891,
-0.116717225692618));
#39460=CARTESIAN_POINT('Ctrl Pts',(-0.359573082794713,-0.541506181145704,
-0.113258734942379));
#39461=CARTESIAN_POINT('Ctrl Pts',(0.64510433218061,1.6868070912627E-15,
-0.740767637572532));
#39462=CARTESIAN_POINT('Ctrl Pts',(0.64510433218061,0.104863177208467,-0.737309146822293));
#39463=CARTESIAN_POINT('Ctrl Pts',(0.593022864567773,0.31448726492509,-0.730392165321814));
#39464=CARTESIAN_POINT('Ctrl Pts',(0.376496494207187,0.555705251652495,
-0.720016693071096));
#39465=CARTESIAN_POINT('Ctrl Pts',(0.0722580868424411,0.667330659810722,
-0.709641220820377));
#39466=CARTESIAN_POINT('Ctrl Pts',(-0.248854270731179,0.623404689437203,
-0.699265748569659));
#39467=CARTESIAN_POINT('Ctrl Pts',(-0.511937757444461,0.434135917498669,
-0.688890276318941));
#39468=CARTESIAN_POINT('Ctrl Pts',(-0.655682143940912,0.143663851624133,
-0.678514804068223));
#39469=CARTESIAN_POINT('Ctrl Pts',(-0.646565972288657,-0.180302757390696,
-0.668139331817503));
#39470=CARTESIAN_POINT('Ctrl Pts',(-0.486719907450942,-0.462234652383724,
-0.657763859566787));
#39471=CARTESIAN_POINT('Ctrl Pts',(-0.213405577826331,-0.636408041354094,
-0.647388387316067));
#39472=CARTESIAN_POINT('Ctrl Pts',(0.109658803578356,-0.662217457765674,
-0.637012915065349));
#39473=CARTESIAN_POINT('Ctrl Pts',(0.407159034924769,-0.533646553620086,
-0.626637442814631));
#39474=CARTESIAN_POINT('Ctrl Pts',(0.609739555547925,-0.28066836620718,
-0.616261970563912));
#39475=CARTESIAN_POINT('Ctrl Pts',(0.670173636573352,0.0377410345494586,
-0.605886498313194));
#39476=CARTESIAN_POINT('Ctrl Pts',(0.574372399022548,0.347352018796665,
-0.595511026062475));
#39477=CARTESIAN_POINT('Ctrl Pts',(0.344669702326589,0.57598600325603,-0.585135553811758));
#39478=CARTESIAN_POINT('Ctrl Pts',(0.0346153286363597,0.670342345204718,
-0.574760081561039));
#39479=CARTESIAN_POINT('Ctrl Pts',(-0.283508794531998,0.608424064864576,
-0.564384609310321));
#39480=CARTESIAN_POINT('Ctrl Pts',(-0.535539483442152,0.404665963460704,
-0.554009137059603));
#39481=CARTESIAN_POINT('Ctrl Pts',(-0.662721682261395,0.106569468561219,
-0.543633664808884));
#39482=CARTESIAN_POINT('Ctrl Pts',(-0.635405841157117,-0.21637120190275,
-0.533258192558166));
#39483=CARTESIAN_POINT('Ctrl Pts',(-0.459960008072277,-0.488869993867697,
-0.522882720307447));
#39484=CARTESIAN_POINT('Ctrl Pts',(-0.177285270709187,-0.647400195178034,
-0.512507248056729));
#39485=CARTESIAN_POINT('Ctrl Pts',(0.146719375860646,-0.655004202041331,
-0.502131775806011));
#39486=CARTESIAN_POINT('Ctrl Pts',(0.436519835836607,-0.509909318262488,
-0.491756303555293));
#39487=CARTESIAN_POINT('Ctrl Pts',(0.624555918656237,-0.245941018152811,
-0.481380831304573));
#39488=CARTESIAN_POINT('Ctrl Pts',(0.666991415072802,0.0753626708238029,
-0.471005359053856));
#39489=CARTESIAN_POINT('Ctrl Pts',(0.553933482875735,0.379097317960756,
-0.460629886803137));
#39490=CARTESIAN_POINT('Ctrl Pts',(0.311738931326063,0.594454303232302,
-0.450254414552419));
#39491=CARTESIAN_POINT('Ctrl Pts',(-0.00313025166471084,0.671228188815089,
-0.439878942301701));
#39492=CARTESIAN_POINT('Ctrl Pts',(-0.317269689785541,0.591520941200901,
-0.429503470050982));
#39493=CARTESIAN_POINT('Ctrl Pts',(-0.55744512965016,0.373914438561531,
-0.419127997800264));
#39494=CARTESIAN_POINT('Ctrl Pts',(-0.667665291955647,0.0691385410136651,
-0.408752525549546));
#39495=CARTESIAN_POINT('Ctrl Pts',(-0.622234927029288,-0.25175538826555,
-0.398377053298828));
#39496=CARTESIAN_POINT('Ctrl Pts',(-0.431745060551924,-0.513958444452011,
-0.388001581048109));
#39497=CARTESIAN_POINT('Ctrl Pts',(-0.140603943943023,-0.656344125353648,
-0.377626108797391));
#39498=CARTESIAN_POINT('Ctrl Pts',(0.183315689490009,-0.645718543884668,
-0.367250636546673));
#39499=CARTESIAN_POINT('Ctrl Pts',(0.464499562861689,-0.484558805560314,
-0.356875164295954));
#39500=CARTESIAN_POINT('Ctrl Pts',(0.637396240941466,-0.210435529226114,
-0.346499692045237));
#39501=CARTESIAN_POINT('Ctrl Pts',(0.661698912187562,0.112745862628511,
-0.336124219794517));
#39502=CARTESIAN_POINT('Ctrl Pts',(0.531741977914689,0.409643197078627,
-0.3257487475438));
#39503=CARTESIAN_POINT('Ctrl Pts',(0.277821854000763,0.611041812978763,
-0.315373275293081));
#39504=CARTESIAN_POINT('Ctrl Pts',(-0.0408659290876403,0.669990340339972,
-0.304997803042363));
#39505=CARTESIAN_POINT('Ctrl Pts',(-0.350026777759515,0.572746308704483,
-0.294622330791644));
#39506=CARTESIAN_POINT('Ctrl Pts',(-0.577587080349824,0.341979890292003,
-0.284246858540926));
#39507=CARTESIAN_POINT('Ctrl Pts',(-0.670496481026748,0.0314888643730044,
-0.273871386290208));
#39508=CARTESIAN_POINT('Ctrl Pts',(-0.607095329516257,-0.286343043569393,
-0.263495914039489));
#39509=CARTESIAN_POINT('Ctrl Pts',(-0.40216411812775,-0.537420795036202,
-0.253120441788771));
#39510=CARTESIAN_POINT('Ctrl Pts',(-0.103477762473797,-0.663211436920841,
-0.242744969538053));
#39511=CARTESIAN_POINT('Ctrl Pts',(0.219332013954502,-0.634389936526523,
-0.232369497287335));
#39512=CARTESIAN_POINT('Ctrl Pts',(0.491009660304339,-0.457675133757216,
-0.221994025036616));
#39513=CARTESIAN_POINT('Ctrl Pts',(0.648219917692676,-0.174264379762606,
-0.211618552785898));
#39514=CARTESIAN_POINT('Ctrl Pts',(0.654312852210673,0.149772606324681,
-0.20124308053518));
#39515=CARTESIAN_POINT('Ctrl Pts',(0.507868126312722,0.43889247785747,-0.190867608284461));
#39516=CARTESIAN_POINT('Ctrl Pts',(0.243025724530227,0.625697109920598,
-0.180492136033743));
#39517=CARTESIAN_POINT('Ctrl Pts',(-0.078472203834126,0.666630614047307,
-0.170116663783025));
#39518=CARTESIAN_POINT('Ctrl Pts',(-0.381676632120979,0.552163746877889,
-0.159741191532307));
#39519=CARTESIAN_POINT('Ctrl Pts',(-0.595901188052075,0.308955036721638,
-0.149365719281588));
#39520=CARTESIAN_POINT('Ctrl Pts',(-0.671207086309358,-0.00624372905956324,
-0.13899024703087));
#39521=CARTESIAN_POINT('Ctrl Pts',(-0.590033827093839,-0.32006005777858,
-0.128614774780151));
#39522=CARTESIAN_POINT('Ctrl Pts',(-0.444213509965361,-0.47940613564774,
-0.121697793279673));
#39523=CARTESIAN_POINT('Ctrl Pts',(-0.356855667887442,-0.537413836530842,
-0.118239302529433));
#39524=CARTESIAN_POINT('Ctrl Pts',(0.641722063808648,1.67796319735318E-15,
-0.742528335043099));
#39525=CARTESIAN_POINT('Ctrl Pts',(0.641722063808647,0.104311776723727,
-0.73906984429286));
#39526=CARTESIAN_POINT('Ctrl Pts',(0.589913462223807,0.312839321707124,
-0.73215286279238));
#39527=CARTESIAN_POINT('Ctrl Pts',(0.374522489184928,0.552791132218716,
-0.721777390541664));
#39528=CARTESIAN_POINT('Ctrl Pts',(0.0718792070526885,0.663831949137389,
-0.711401918290943));
#39529=CARTESIAN_POINT('Ctrl Pts',(-0.247549473477458,0.62013595091581,
-0.701026446040226));
#39530=CARTESIAN_POINT('Ctrl Pts',(-0.509253578428028,0.431859720500806,
-0.690650973789508));
#39531=CARTESIAN_POINT('Ctrl Pts',(-0.652244280175453,0.142910567006098,
-0.680275501538789));
#39532=CARTESIAN_POINT('Ctrl Pts',(-0.643175909604444,-0.179357382558957,
-0.669900029288072));
#39533=CARTESIAN_POINT('Ctrl Pts',(-0.484167945284686,-0.459811078726279,
-0.659524557037352));
#39534=CARTESIAN_POINT('Ctrl Pts',(-0.212286653582936,-0.633071233790531,
-0.649149084786634));
#39535=CARTESIAN_POINT('Ctrl Pts',(0.109083842531312,-0.658745332205166,
-0.638773612535916));
#39536=CARTESIAN_POINT('Ctrl Pts',(0.405024225471376,-0.530848546088013,
-0.628398140285198));
#39537=CARTESIAN_POINT('Ctrl Pts',(0.606542579433963,-0.279196771030968,
-0.618022668034478));
#39538=CARTESIAN_POINT('Ctrl Pts',(0.66665979345154,0.0375431516282889,
-0.607647195783762));
#39539=CARTESIAN_POINT('Ctrl Pts',(0.571360859360168,0.345530788434487,
-0.597271723533042));
#39540=CARTESIAN_POINT('Ctrl Pts',(0.342862535954226,0.572966003221409,
-0.586896251282324));
#39541=CARTESIAN_POINT('Ctrl Pts',(0.0344338341315972,0.666827617500848,
-0.576520779031606));
#39542=CARTESIAN_POINT('Ctrl Pts',(-0.282022306005166,0.60523398608833,
-0.566145306780888));
#39543=CARTESIAN_POINT('Ctrl Pts',(-0.532731551857879,0.40254422570126,
-0.555769834530169));
#39544=CARTESIAN_POINT('Ctrl Pts',(-0.659246911119028,0.106010705325554,
-0.545394362279451));
#39545=CARTESIAN_POINT('Ctrl Pts',(-0.632074291971503,-0.21523672806957,
-0.535018890028733));
#39546=CARTESIAN_POINT('Ctrl Pts',(-0.457548353518703,-0.486306758963348,
-0.524643417778014));
#39547=CARTESIAN_POINT('Ctrl Pts',(-0.176355731569013,-0.644005757398423,
-0.514267945527297));
#39548=CARTESIAN_POINT('Ctrl Pts',(0.145950099304638,-0.651569895060505,
-0.503892473276577));
#39549=CARTESIAN_POINT('Ctrl Pts',(0.43423108239854,-0.507235770328543,
-0.493517001025861));
#39550=CARTESIAN_POINT('Ctrl Pts',(0.621281257601356,-0.244651504356012,
-0.48314152877514));
#39551=CARTESIAN_POINT('Ctrl Pts',(0.663494256939109,0.0749675305396655,
-0.472766056524424));
#39552=CARTESIAN_POINT('Ctrl Pts',(0.551029108184565,0.377109641299561,
-0.462390584273704));
#39553=CARTESIAN_POINT('Ctrl Pts',(0.310104427021151,0.591337470459519,
-0.452015112022986));
#39554=CARTESIAN_POINT('Ctrl Pts',(-0.00311383918199809,0.667708816500798,
-0.441639639772268));
#39555=CARTESIAN_POINT('Ctrl Pts',(-0.31560618670119,0.588419488582432,
-0.431264167521549));
#39556=CARTESIAN_POINT('Ctrl Pts',(-0.554522342751875,0.371953936686142,
-0.420888695270832));
#39557=CARTESIAN_POINT('Ctrl Pts',(-0.664164600562044,0.0687760349819571,
-0.410513223020113));
#39558=CARTESIAN_POINT('Ctrl Pts',(-0.61897243535856,-0.25043538866153,
-0.400137750769395));
#39559=CARTESIAN_POINT('Ctrl Pts',(-0.429481342135034,-0.511263666207844,
-0.389762278518676));
#39560=CARTESIAN_POINT('Ctrl Pts',(-0.139866731716529,-0.652902792909725,
-0.379386806267958));
#39561=CARTESIAN_POINT('Ctrl Pts',(0.182354531759966,-0.642332923310336,
-0.369011334017239));
#39562=CARTESIAN_POINT('Ctrl Pts',(0.462064106590771,-0.48201817500657,
-0.358635861766521));
#39563=CARTESIAN_POINT('Ctrl Pts',(0.634054255725814,-0.209332177210148,
-0.348260389515803));
#39564=CARTESIAN_POINT('Ctrl Pts',(0.658229503614937,0.112154715424475,
-0.337884917265084));
#39565=CARTESIAN_POINT('Ctrl Pts',(0.528953957349416,0.407495362778231,
-0.327509445014367));
#39566=CARTESIAN_POINT('Ctrl Pts',(0.276365183140412,0.607838008857103,
-0.317133972763648));
#39567=CARTESIAN_POINT('Ctrl Pts',(-0.040651661531787,0.666477458287253,
-0.30675850051293));
#39568=CARTESIAN_POINT('Ctrl Pts',(-0.348191523276064,0.569743294931616,
-0.296383028262211));
#39569=CARTESIAN_POINT('Ctrl Pts',(-0.574558685491881,0.340186827082857,
-0.286007556011493));
#39570=CARTESIAN_POINT('Ctrl Pts',(-0.666980945237279,0.0313237625272405,
-0.275632083760775));
#39571=CARTESIAN_POINT('Ctrl Pts',(-0.60391221743454,-0.284841694627466,
-0.265256611510056));
#39572=CARTESIAN_POINT('Ctrl Pts',(-0.400055498194385,-0.534602999246615,
-0.254881139259338));
#39573=CARTESIAN_POINT('Ctrl Pts',(-0.102935209247226,-0.659734098192411,
-0.24450566700862));
#39574=CARTESIAN_POINT('Ctrl Pts',(0.218182015307551,-0.631063713343416,
-0.234130194757901));
#39575=CARTESIAN_POINT('Ctrl Pts',(0.488435208193123,-0.455275460354312,
-0.223754722507183));
#39576=CARTESIAN_POINT('Ctrl Pts',(0.644821179064956,-0.173350677448309,
-0.213379250256465));
#39577=CARTESIAN_POINT('Ctrl Pts',(0.65088217585303,0.148987316632804,-0.203003778005747));
#39578=CARTESIAN_POINT('Ctrl Pts',(0.505205269294179,0.436591293146462,
-0.192628305755028));
#39579=CARTESIAN_POINT('Ctrl Pts',(0.241751518866823,0.622416447653164,
-0.18225283350431));
#39580=CARTESIAN_POINT('Ctrl Pts',(-0.0780608048519096,0.663135382918645,
-0.171877361253591));
#39581=CARTESIAN_POINT('Ctrl Pts',(-0.379675341865185,0.549268581130195,
-0.161501889002874));
#39582=CARTESIAN_POINT('Ctrl Pts',(-0.592776947792401,0.307335268506549,
-0.151126416752155));
#39583=CARTESIAN_POINT('Ctrl Pts',(-0.667687464951409,-0.00621127295214926,
-0.140750944501437));
#39584=CARTESIAN_POINT('Ctrl Pts',(-0.586940939264991,-0.318381324725216,
-0.130375472250718));
#39585=CARTESIAN_POINT('Ctrl Pts',(-0.441883170803417,-0.476893507297812,
-0.12345849075024));
#39586=CARTESIAN_POINT('Ctrl Pts',(-0.354984681166936,-0.5345961871503,
-0.12));
#39587=CARTESIAN_POINT('',(-0.635960060745576,-0.14190617018468,-0.12));
#39588=CARTESIAN_POINT('',(-0.354984681166936,-0.5345961871503,-0.12));
#39589=CARTESIAN_POINT('Ctrl Pts',(-0.635960060745577,-0.141906170184675,
-0.12));
#39590=CARTESIAN_POINT('Ctrl Pts',(-0.618732434913983,-0.219112693030753,
-0.12));
#39591=CARTESIAN_POINT('Ctrl Pts',(-0.587040279218795,-0.292493231368224,
-0.12));
#39592=CARTESIAN_POINT('Ctrl Pts',(-0.514176950918451,-0.399397075481082,
-0.12));
#39593=CARTESIAN_POINT('Ctrl Pts',(-0.480780442117076,-0.437485150144931,
-0.12));
#39594=CARTESIAN_POINT('Ctrl Pts',(-0.411075652466351,-0.499087766122273,
-0.12));
#39595=CARTESIAN_POINT('Ctrl Pts',(-0.380549980087873,-0.519871240387648,
-0.12));
#39596=CARTESIAN_POINT('Ctrl Pts',(-0.354984681166936,-0.5345961871503,
-0.12));
#39597=CARTESIAN_POINT('',(0.651577129589243,7.55905383458807E-9,-0.726249999720643));
#39598=CARTESIAN_POINT('Ctrl Pts',(0.6516,1.70379184550113E-15,-0.72625));
#39599=CARTESIAN_POINT('Ctrl Pts',(0.6516,0.10591743302354,-0.722791509249761));
#39600=CARTESIAN_POINT('Ctrl Pts',(0.625296958000537,0.211786122892756,
-0.719333018499521));
#39601=CARTESIAN_POINT('Ctrl Pts',(0.575694361073646,0.305328026911275,
-0.715874527749282));
#39602=CARTESIAN_POINT('Ctrl Pts',(0.526091764146756,0.398869930929794,
-0.712416036999042));
#39603=CARTESIAN_POINT('Ctrl Pts',(0.453189612292437,0.480085049097615,
-0.708957546248803));
#39604=CARTESIAN_POINT('Ctrl Pts',(0.365521565197895,0.539484283577253,
-0.705499055498563));
#39605=CARTESIAN_POINT('Ctrl Pts',(0.277853518103352,0.59888351805689,-0.702040564748324));
#39606=CARTESIAN_POINT('Ctrl Pts',(0.175419575768586,0.636466868848343,
-0.698582073998084));
#39607=CARTESIAN_POINT('Ctrl Pts',(0.0701450044936301,0.647863776829187,
-0.695123583247845));
#39608=CARTESIAN_POINT('Ctrl Pts',(-0.0351295667813255,0.659260684810031,
-0.691665092497606));
#39609=CARTESIAN_POINT('Ctrl Pts',(-0.14324476699647,0.644471149980266,
-0.688206601747366));
#39610=CARTESIAN_POINT('Ctrl Pts',(-0.241591113588699,0.605213992636453,
-0.684748110997127));
#39611=CARTESIAN_POINT('Ctrl Pts',(-0.339937460180928,0.565956835292639,
-0.681289620246888));
#39612=CARTESIAN_POINT('Ctrl Pts',(-0.428514953150241,0.502232055434778,
-0.677831129496648));
#39613=CARTESIAN_POINT('Ctrl Pts',(-0.497002322505376,0.421470181072845,
-0.674372638746409));
#39614=CARTESIAN_POINT('Ctrl Pts',(-0.565489691860511,0.340708306710911,
-0.670914147996169));
#39615=CARTESIAN_POINT('Ctrl Pts',(-0.613886937601468,0.242909337844905,
-0.667455657245929));
#39616=CARTESIAN_POINT('Ctrl Pts',(-0.636550900687667,0.139471757721302,
-0.66399716649569));
#39617=CARTESIAN_POINT('Ctrl Pts',(-0.659214863773866,0.0360341775977008,
-0.660538675745451));
#39618=CARTESIAN_POINT('Ctrl Pts',(-0.656145544205308,-0.0730420137834978,
-0.657080184995211));
#39619=CARTESIAN_POINT('Ctrl Pts',(-0.627701625882157,-0.175041889458731,
-0.653621694244972));
#39620=CARTESIAN_POINT('Ctrl Pts',(-0.599257707559006,-0.277041765133964,
-0.650163203494733));
#39621=CARTESIAN_POINT('Ctrl Pts',(-0.545439190481261,-0.371965325103232,
-0.646704712744493));
#39622=CARTESIAN_POINT('Ctrl Pts',(-0.472518878335208,-0.448748292407348,
-0.643246221994254));
#39623=CARTESIAN_POINT('Ctrl Pts',(-0.399598566189156,-0.525531259711463,
-0.639787731244014));
#39624=CARTESIAN_POINT('Ctrl Pts',(-0.307576458974796,-0.584173634350426,
-0.636329240493775));
#39625=CARTESIAN_POINT('Ctrl Pts',(-0.207179187647643,-0.617839704361461,
-0.632870749743535));
#39626=CARTESIAN_POINT('Ctrl Pts',(-0.10678191632049,-0.651505774372495,
-0.629412258993296));
#39627=CARTESIAN_POINT('Ctrl Pts',(0.00199051911945597,-0.6601955397556,
-0.625953768243056));
#39628=CARTESIAN_POINT('Ctrl Pts',(0.106459362012925,-0.64289617526343,
-0.622495277492817));
#39629=CARTESIAN_POINT('Ctrl Pts',(0.210928204906394,-0.62559681077126,
-0.619036786742578));
#39630=CARTESIAN_POINT('Ctrl Pts',(0.311093455253387,-0.582308316403815,
-0.615578295992338));
#39631=CARTESIAN_POINT('Ctrl Pts',(0.395279463300225,-0.518076500064383,
-0.612119805242099));
#39632=CARTESIAN_POINT('Ctrl Pts',(0.479465471347062,-0.453844683724952,
-0.608661314491859));
#39633=CARTESIAN_POINT('Ctrl Pts',(0.547672237093744,-0.368669545413534,
-0.60520282374162));
#39634=CARTESIAN_POINT('Ctrl Pts',(0.591949384920031,-0.272479400406464,
-0.60174433299138));
#39635=CARTESIAN_POINT('Ctrl Pts',(0.636226532746319,-0.176289255399394,
-0.598285842241141));
#39636=CARTESIAN_POINT('Ctrl Pts',(0.656574062652212,-0.0690841036966703,
-0.594827351490901));
#39637=CARTESIAN_POINT('Ctrl Pts',(0.650620184773465,0.0366398799159285,
-0.591368860740662));
#39638=CARTESIAN_POINT('Ctrl Pts',(0.644666306894718,0.142363863528527,
-0.587910369990422));
#39639=CARTESIAN_POINT('Ctrl Pts',(0.612411021231331,0.246606679051001,
-0.584451879240183));
#39640=CARTESIAN_POINT('Ctrl Pts',(0.557614117482213,0.337217435579939,
-0.580993388489944));
#39641=CARTESIAN_POINT('Ctrl Pts',(0.502817213733094,0.427828192108876,
-0.577534897739704));
#39642=CARTESIAN_POINT('Ctrl Pts',(0.425478691898243,0.504806889644278,
-0.574076406989465));
#39643=CARTESIAN_POINT('Ctrl Pts',(0.334613380841695,0.559180640531877,
-0.570617916239225));
#39644=CARTESIAN_POINT('Ctrl Pts',(0.243748069785148,0.613554391419475,
-0.567159425488986));
#39645=CARTESIAN_POINT('Ctrl Pts',(0.139355969506901,0.64532319565927,-0.563700934738746));
#39646=CARTESIAN_POINT('Ctrl Pts',(0.0336053686408143,0.650783975546671,
-0.560242443988507));
#39647=CARTESIAN_POINT('Ctrl Pts',(-0.0721452322252732,0.656244755434072,
-0.556783953238268));
#39648=CARTESIAN_POINT('Ctrl Pts',(-0.179254333679203,0.635397510969078,
-0.553325462488028));
#39649=CARTESIAN_POINT('Ctrl Pts',(-0.275236947324888,0.590672266243827,
-0.549866971737789));
#39650=CARTESIAN_POINT('Ctrl Pts',(-0.371219560970573,0.545947021518575,
-0.546408480987549));
#39651=CARTESIAN_POINT('Ctrl Pts',(-0.456075686808014,0.477343776533065,
-0.54294999023731));
#39652=CARTESIAN_POINT('Ctrl Pts',(-0.519914215083365,0.39285915094755,
-0.53949149948707));
#39653=CARTESIAN_POINT('Ctrl Pts',(-0.583752743358716,0.308374525362036,
-0.536033008736831));
#39654=CARTESIAN_POINT('Ctrl Pts',(-0.626573674071979,0.208008519176516,
-0.532574517986592));
#39655=CARTESIAN_POINT('Ctrl Pts',(-0.643385658862261,0.103460124531451,
-0.529116027236352));
#39656=CARTESIAN_POINT('Ctrl Pts',(-0.660197643652543,-0.00108827011361441,
-0.525657536486113));
#39657=CARTESIAN_POINT('Ctrl Pts',(-0.651000682519846,-0.109819053218224,
-0.522199045735874));
#39658=CARTESIAN_POINT('Ctrl Pts',(-0.616866803398733,-0.210058206972732,
-0.518740554985634));
#39659=CARTESIAN_POINT('Ctrl Pts',(-0.58273292427762,-0.310297360727239,
-0.515282064235395));
#39660=CARTESIAN_POINT('Ctrl Pts',(-0.523662127168093,-0.402044885131643,
-0.511823573485155));
#39661=CARTESIAN_POINT('Ctrl Pts',(-0.446539898635107,-0.474606386771079,
-0.508365082734915));
#39662=CARTESIAN_POINT('Ctrl Pts',(-0.36941767010212,-0.547167888410515,
-0.504906591984676));
#39663=CARTESIAN_POINT('Ctrl Pts',(-0.274244010145674,-0.600543367284983,
-0.501448101234437));
#39664=CARTESIAN_POINT('Ctrl Pts',(-0.172112673741822,-0.628511201947908,
-0.497989610484197));
#39665=CARTESIAN_POINT('Ctrl Pts',(-0.0699813373379707,-0.656479036610833,
-0.494531119733958));
#39666=CARTESIAN_POINT('Ctrl Pts',(0.039107675513287,-0.659039227062215,
-0.491072628983718));
#39667=CARTESIAN_POINT('Ctrl Pts',(0.142438590463173,-0.635893349066943,
-0.487614138233479));
#39668=CARTESIAN_POINT('Ctrl Pts',(0.245769505413058,-0.612747471071672,
-0.484155647483239));
#39669=CARTESIAN_POINT('Ctrl Pts',(0.343342322461571,-0.563895524629746,
-0.480697156733));
#39670=CARTESIAN_POINT('Ctrl Pts',(0.423783632963894,-0.495031853388289,
-0.477238665982761));
#39671=CARTESIAN_POINT('Ctrl Pts',(0.504224943466218,-0.426168182146832,
-0.473780175232521));
#39672=CARTESIAN_POINT('Ctrl Pts',(0.567534747422353,-0.337292786105845,
-0.470321684482282));
#39673=CARTESIAN_POINT('Ctrl Pts',(0.606333445736285,-0.238765273900591,
-0.466863193732042));
#39674=CARTESIAN_POINT('Ctrl Pts',(0.645132144050218,-0.140237761695336,
-0.463404702981803));
#39675=CARTESIAN_POINT('Ctrl Pts',(0.659419736721948,-0.0320581333258157,
-0.459946212231564));
#39676=CARTESIAN_POINT('Ctrl Pts',(0.647530814933311,0.0731638377210296,
-0.456487721481324));
#39677=CARTESIAN_POINT('Ctrl Pts',(0.635641893144675,0.178385808767874,
-0.453029230731085));
#39678=CARTESIAN_POINT('Ctrl Pts',(0.597576456895672,0.280650122492043,
-0.449570739980845));
#39679=CARTESIAN_POINT('Ctrl Pts',(0.537771538702094,0.368036513950164,
-0.446112249230605));
#39680=CARTESIAN_POINT('Ctrl Pts',(0.477966620508516,0.455422905408286,
-0.442653758480366));
#39681=CARTESIAN_POINT('Ctrl Pts',(0.396422220370362,0.527931374600361,
-0.439195267730127));
#39682=CARTESIAN_POINT('Ctrl Pts',(0.302643421918522,0.57711009574258,-0.435736776979887));
#39683=CARTESIAN_POINT('Ctrl Pts',(0.208864623466684,0.626288816884798,
-0.432278286229648));
#39684=CARTESIAN_POINT('Ctrl Pts',(0.102851426701161,0.652137789977161,
-0.428819795479408));
#39685=CARTESIAN_POINT('Ctrl Pts',(-0.00303892128990968,0.651643973651179,
-0.425361304729169));
#39686=CARTESIAN_POINT('Ctrl Pts',(-0.108929269280981,0.651150157325197,
-0.421902813978929));
#39687=CARTESIAN_POINT('Ctrl Pts',(-0.2146967684976,0.624313551580869,-0.41844432322869));
#39688=CARTESIAN_POINT('Ctrl Pts',(-0.308012811166104,0.574262319498799,
-0.414985832478451));
#39689=CARTESIAN_POINT('Ctrl Pts',(-0.401328853834608,0.524211087416729,
-0.411527341728211));
#39690=CARTESIAN_POINT('Ctrl Pts',(-0.482193439954999,0.450945228996916,
-0.408068850977972));
#39691=CARTESIAN_POINT('Ctrl Pts',(-0.541180727256026,0.363004853803835,
-0.404610360227732));
#39692=CARTESIAN_POINT('Ctrl Pts',(-0.600168014557053,0.275064478610752,
-0.401151869477493));
#39693=CARTESIAN_POINT('Ctrl Pts',(-0.637278003038717,0.1724495866444,-0.397693378727254));
#39694=CARTESIAN_POINT('Ctrl Pts',(-0.648185030320193,0.0671213074021386,
-0.394234887977014));
#39695=CARTESIAN_POINT('Ctrl Pts',(-0.659092057601669,-0.0382069718401229,
-0.390776397226775));
#39696=CARTESIAN_POINT('Ctrl Pts',(-0.643796123682957,-0.146248638358292,
-0.387317906476535));
#39697=CARTESIAN_POINT('Ctrl Pts',(-0.604080172958263,-0.244409999953607,
-0.383859415726295));
#39698=CARTESIAN_POINT('Ctrl Pts',(-0.564364222233568,-0.342571361548922,
-0.380400924976056));
#39699=CARTESIAN_POINT('Ctrl Pts',(-0.50022825470289,-0.430852418221385,
-0.376942434225817));
#39700=CARTESIAN_POINT('Ctrl Pts',(-0.419148169803331,-0.498962839486855,
-0.373483943475577));
#39701=CARTESIAN_POINT('Ctrl Pts',(-0.338068084903774,-0.567073260752324,
-0.370025452725338));
#39702=CARTESIAN_POINT('Ctrl Pts',(-0.240043882635337,-0.615013046610803,
-0.366566961975098));
#39703=CARTESIAN_POINT('Ctrl Pts',(-0.13650158659733,-0.637194177857639,
-0.363108471224859));
#39704=CARTESIAN_POINT('Ctrl Pts',(-0.0329592905593207,-0.659375309104476,
-0.359649980474619));
#39705=CARTESIAN_POINT('Ctrl Pts',(0.0761010992482581,-0.65579778573967,
-0.35619148972438));
#39706=CARTESIAN_POINT('Ctrl Pts',(0.17796714488833,-0.626878615664482,
-0.352732998974141));
#39707=CARTESIAN_POINT('Ctrl Pts',(0.279833190528402,-0.597959445589294,
-0.349274508223901));
#39708=CARTESIAN_POINT('Ctrl Pts',(0.374504892000968,-0.543698628803726,
-0.345816017473662));
#39709=CARTESIAN_POINT('Ctrl Pts',(0.450947004231846,-0.470420984666961,
-0.342357526723422));
#39710=CARTESIAN_POINT('Ctrl Pts',(0.527389116462723,-0.397143340530196,
-0.338899035973183));
#39711=CARTESIAN_POINT('Ctrl Pts',(0.585601639451913,-0.304848869042235,
-0.335440545222943));
#39712=CARTESIAN_POINT('Ctrl Pts',(0.618799129951752,-0.204295717545714,
-0.331982054472704));
#39713=CARTESIAN_POINT('Ctrl Pts',(0.651996620451591,-0.103742566049191,
-0.328523563722465));
#39714=CARTESIAN_POINT('Ctrl Pts',(0.660179078462078,0.00506926545589149,
-0.325065072972225));
#39715=CARTESIAN_POINT('Ctrl Pts',(0.642392729749155,0.109456311843489,
-0.321606582221986));
#39716=CARTESIAN_POINT('Ctrl Pts',(0.624606381036232,0.213843358231086,
-0.318148091471746));
#39717=CARTESIAN_POINT('Ctrl Pts',(0.580851225599901,0.313805619501198,
-0.314689600721507));
#39718=CARTESIAN_POINT('Ctrl Pts',(0.516227508351651,0.397691165445017,
-0.311231109971267));
#39719=CARTESIAN_POINT('Ctrl Pts',(0.451603791103401,0.481576711388838,
-0.307772619221028));
#39720=CARTESIAN_POINT('Ctrl Pts',(0.366111512043233,0.549385542006366,
-0.304314128470789));
#39721=CARTESIAN_POINT('Ctrl Pts',(0.269715932556123,0.593213637000255,
-0.300855637720549));
#39722=CARTESIAN_POINT('Ctrl Pts',(0.173320353069013,0.637041731994143,
-0.29739714697031));
#39723=CARTESIAN_POINT('Ctrl Pts',(0.0660214731549615,0.656889091364393,
-0.29393865622007));
#39724=CARTESIAN_POINT('Ctrl Pts',(-0.0396735966300387,0.65044224129389,
-0.290480165469831));
#39725=CARTESIAN_POINT('Ctrl Pts',(-0.145368666415039,0.643995391223387,
-0.287021674719591));
#39726=CARTESIAN_POINT('Ctrl Pts',(-0.249459926070987,0.611254331712133,
-0.283563183969352));
#39727=CARTESIAN_POINT('Ctrl Pts',(-0.339814155841332,0.556035468987531,
-0.280104693219112));
#39728=CARTESIAN_POINT('Ctrl Pts',(-0.430168385611676,0.500816606262931,
-0.276646202468873));
#39729=CARTESIAN_POINT('Ctrl Pts',(-0.506785585496417,0.423119940324984,
-0.273187711718634));
#39730=CARTESIAN_POINT('Ctrl Pts',(-0.560735002506506,0.332002049080791,
-0.269729220968394));
#39731=CARTESIAN_POINT('Ctrl Pts',(-0.614684419516595,0.240884157836599,
-0.266270730218155));
#39732=CARTESIAN_POINT('Ctrl Pts',(-0.645966053652034,0.136345041286161,
-0.262812239467915));
#39733=CARTESIAN_POINT('Ctrl Pts',(-0.650933614764165,0.0305701251879336,
-0.259353748717676));
#39734=CARTESIAN_POINT('Ctrl Pts',(-0.655901175876297,-0.075204790910295,
-0.255895257967436));
#39735=CARTESIAN_POINT('Ctrl Pts',(-0.634554663965122,-0.182215506556313,
-0.252436767217197));
#39736=CARTESIAN_POINT('Ctrl Pts',(-0.589382298569403,-0.27798850517175,
-0.248978276466957));
#39737=CARTESIAN_POINT('Ctrl Pts',(-0.544209933173686,-0.373761503787186,
-0.245519785716718));
#39738=CARTESIAN_POINT('Ctrl Pts',(-0.475211714293426,-0.458296785372042,
-0.242061294966479));
#39739=CARTESIAN_POINT('Ctrl Pts',(-0.390430301657806,-0.521740630181612,
-0.238602804216239));
#39740=CARTESIAN_POINT('Ctrl Pts',(-0.305648889022187,-0.585184474991182,
-0.235144313466));
#39741=CARTESIAN_POINT('Ctrl Pts',(-0.205084282631209,-0.627536883025467,
-0.23168582271576));
#39742=CARTESIAN_POINT('Ctrl Pts',(-0.100458623404491,-0.643861136377049,
-0.228227331965521));
#39743=CARTESIAN_POINT('Ctrl Pts',(0.00416703582222801,-0.660185389728631,
-0.224768841215281));
#39744=CARTESIAN_POINT('Ctrl Pts',(0.112853747884687,-0.650481488397511,
-0.221310350465042));
#39745=CARTESIAN_POINT('Ctrl Pts',(0.212932630871593,-0.615880514983204,
-0.217851859714803));
#39746=CARTESIAN_POINT('Ctrl Pts',(0.3130115138585,-0.581279541568896,-0.214393368964563));
#39747=CARTESIAN_POINT('Ctrl Pts',(0.404482567769854,-0.521781496071402,
-0.210934878214324));
#39748=CARTESIAN_POINT('Ctrl Pts',(0.47668362769456,-0.444321738176853,
-0.207476387464084));
#39749=CARTESIAN_POINT('Ctrl Pts',(0.548884687619267,-0.366861980282302,
-0.204017896713845));
#39750=CARTESIAN_POINT('Ctrl Pts',(0.601815753557325,-0.271440509990697,
-0.200559405963605));
#39751=CARTESIAN_POINT('Ctrl Pts',(0.629307002000867,-0.169179825370744,
-0.197100915213366));
#39752=CARTESIAN_POINT('Ctrl Pts',(0.656798250444408,-0.0669191407507926,
-0.193642424463126));
#39753=CARTESIAN_POINT('Ctrl Pts',(0.658849681393434,0.0421807581975068,
-0.190183933712887));
#39754=CARTESIAN_POINT('Ctrl Pts',(0.635222181800982,0.145402544921586,
-0.186725442962648));
#39755=CARTESIAN_POINT('Ctrl Pts',(0.61159468220853,0.248624331645664,-0.183266952212408));
#39756=CARTESIAN_POINT('Ctrl Pts',(0.5622882520746,0.345968006145523,-0.179808461462169));
#39757=CARTESIAN_POINT('Ctrl Pts',(0.493050194269639,0.426087432496028,
-0.176349970711929));
#39758=CARTESIAN_POINT('Ctrl Pts',(0.423812136464678,0.506206858846533,
-0.17289147996169));
#39759=CARTESIAN_POINT('Ctrl Pts',(0.334642450988686,0.569102037047685,
-0.16943298921145));
#39760=CARTESIAN_POINT('Ctrl Pts',(0.235935083384207,0.607440578819556,
-0.165974498461211));
#39761=CARTESIAN_POINT('Ctrl Pts',(0.137227715779728,0.645779120591427,
-0.162516007710972));
#39762=CARTESIAN_POINT('Ctrl Pts',(0.0289826660467615,0.659561025934017,
-0.159057516960732));
#39763=CARTESIAN_POINT('Ctrl Pts',(-0.0761827332461323,0.64718205573429,
-0.155599026210493));
#39764=CARTESIAN_POINT('Ctrl Pts',(-0.181348132539026,0.634803085534563,
-0.152140535460253));
#39765=CARTESIAN_POINT('Ctrl Pts',(-0.283433881391847,0.59626323979252,
-0.148682044710014));
#39766=CARTESIAN_POINT('Ctrl Pts',(-0.370540397243242,0.536050423989017,
-0.145223553959774));
#39767=CARTESIAN_POINT('Ctrl Pts',(-0.457646913094635,0.475837608185515,
-0.141765063209535));
#39768=CARTESIAN_POINT('Ctrl Pts',(-0.529774195944603,0.393951822320553,
-0.138306572459295));
#39769=CARTESIAN_POINT('Ctrl Pts',(-0.578515104713621,0.299946776280357,
-0.134848081709056));
#39770=CARTESIAN_POINT('Ctrl Pts',(-0.627256013482641,0.205941730240159,
-0.131389590958817));
#39771=CARTESIAN_POINT('Ctrl Pts',(-0.652610548170711,0.0998174240247245,
-0.127931100208577));
#39772=CARTESIAN_POINT('Ctrl Pts',(-0.651622907941676,-0.00607393589154021,
-0.124472609458338));
#39773=CARTESIAN_POINT('Ctrl Pts',(-0.651197160667425,-0.0517210820139664,
-0.122981739638892));
#39774=CARTESIAN_POINT('Ctrl Pts',(-0.645876355431924,-0.097324940684241,
-0.121490869819446));
#39775=CARTESIAN_POINT('Ctrl Pts',(-0.635915580576687,-0.141895556916034,
-0.12));
#39776=CARTESIAN_POINT('',(0.462889160393651,0.44445565849575,-0.72625));
#39777=CARTESIAN_POINT('Ctrl Pts',(0.46288916039365,0.444455658495751,-0.72625));
#39778=CARTESIAN_POINT('Ctrl Pts',(0.484632932366815,0.424517500232759,
-0.72625));
#39779=CARTESIAN_POINT('Ctrl Pts',(0.509898268129295,0.397586621949268,
-0.72625));
#39780=CARTESIAN_POINT('Ctrl Pts',(0.564515398139937,0.322282107413605,
-0.72625));
#39781=CARTESIAN_POINT('Ctrl Pts',(0.588817231863487,0.277831998563094,
-0.72625));
#39782=CARTESIAN_POINT('Ctrl Pts',(0.636649969955028,0.157623573436602,
-0.72625));
#39783=CARTESIAN_POINT('Ctrl Pts',(0.6516,0.079103795955392,-0.72625));
#39784=CARTESIAN_POINT('Ctrl Pts',(0.6516,2.83106871279415E-15,-0.72625));
#39785=CARTESIAN_POINT('Ctrl Pts',(0.462856220566271,0.444424947352554,
-0.72625));
#39786=CARTESIAN_POINT('Ctrl Pts',(0.431715399494611,0.476878719990873,
-0.724759130180555));
#39787=CARTESIAN_POINT('Ctrl Pts',(0.317128739570665,0.573849087968775,
-0.71980976961087));
#39788=CARTESIAN_POINT('Ctrl Pts',(0.0718792070526885,0.663831949137389,
-0.711401918290943));
#39789=CARTESIAN_POINT('Ctrl Pts',(-0.247549473477458,0.62013595091581,
-0.701026446040226));
#39790=CARTESIAN_POINT('Ctrl Pts',(-0.509253578428028,0.431859720500806,
-0.690650973789508));
#39791=CARTESIAN_POINT('Ctrl Pts',(-0.652244280175453,0.142910567006098,
-0.680275501538789));
#39792=CARTESIAN_POINT('Ctrl Pts',(-0.643175909604444,-0.179357382558957,
-0.669900029288072));
#39793=CARTESIAN_POINT('Ctrl Pts',(-0.484167945284686,-0.459811078726279,
-0.659524557037352));
#39794=CARTESIAN_POINT('Ctrl Pts',(-0.212286653582936,-0.633071233790531,
-0.649149084786634));
#39795=CARTESIAN_POINT('Ctrl Pts',(0.109083842531312,-0.658745332205166,
-0.638773612535916));
#39796=CARTESIAN_POINT('Ctrl Pts',(0.405024225471376,-0.530848546088013,
-0.628398140285198));
#39797=CARTESIAN_POINT('Ctrl Pts',(0.606542579433963,-0.279196771030968,
-0.618022668034478));
#39798=CARTESIAN_POINT('Ctrl Pts',(0.66665979345154,0.0375431516282889,
-0.607647195783762));
#39799=CARTESIAN_POINT('Ctrl Pts',(0.571360859360168,0.345530788434487,
-0.597271723533042));
#39800=CARTESIAN_POINT('Ctrl Pts',(0.342862535954226,0.572966003221409,
-0.586896251282324));
#39801=CARTESIAN_POINT('Ctrl Pts',(0.0344338341315972,0.666827617500848,
-0.576520779031606));
#39802=CARTESIAN_POINT('Ctrl Pts',(-0.282022306005166,0.60523398608833,
-0.566145306780888));
#39803=CARTESIAN_POINT('Ctrl Pts',(-0.532731551857879,0.40254422570126,
-0.555769834530169));
#39804=CARTESIAN_POINT('Ctrl Pts',(-0.659246911119028,0.106010705325554,
-0.545394362279451));
#39805=CARTESIAN_POINT('Ctrl Pts',(-0.632074291971503,-0.21523672806957,
-0.535018890028733));
#39806=CARTESIAN_POINT('Ctrl Pts',(-0.457548353518703,-0.486306758963348,
-0.524643417778014));
#39807=CARTESIAN_POINT('Ctrl Pts',(-0.176355731569013,-0.644005757398423,
-0.514267945527297));
#39808=CARTESIAN_POINT('Ctrl Pts',(0.145950099304638,-0.651569895060505,
-0.503892473276577));
#39809=CARTESIAN_POINT('Ctrl Pts',(0.43423108239854,-0.507235770328543,
-0.493517001025861));
#39810=CARTESIAN_POINT('Ctrl Pts',(0.621281257601356,-0.244651504356012,
-0.48314152877514));
#39811=CARTESIAN_POINT('Ctrl Pts',(0.663494256939109,0.0749675305396655,
-0.472766056524424));
#39812=CARTESIAN_POINT('Ctrl Pts',(0.551029108184565,0.377109641299561,
-0.462390584273704));
#39813=CARTESIAN_POINT('Ctrl Pts',(0.310104427021151,0.591337470459519,
-0.452015112022986));
#39814=CARTESIAN_POINT('Ctrl Pts',(-0.00311383918199809,0.667708816500798,
-0.441639639772268));
#39815=CARTESIAN_POINT('Ctrl Pts',(-0.31560618670119,0.588419488582432,
-0.431264167521549));
#39816=CARTESIAN_POINT('Ctrl Pts',(-0.554522342751875,0.371953936686142,
-0.420888695270832));
#39817=CARTESIAN_POINT('Ctrl Pts',(-0.664164600562044,0.0687760349819571,
-0.410513223020113));
#39818=CARTESIAN_POINT('Ctrl Pts',(-0.61897243535856,-0.25043538866153,
-0.400137750769395));
#39819=CARTESIAN_POINT('Ctrl Pts',(-0.429481342135034,-0.511263666207844,
-0.389762278518676));
#39820=CARTESIAN_POINT('Ctrl Pts',(-0.139866731716529,-0.652902792909725,
-0.379386806267958));
#39821=CARTESIAN_POINT('Ctrl Pts',(0.182354531759966,-0.642332923310336,
-0.369011334017239));
#39822=CARTESIAN_POINT('Ctrl Pts',(0.462064106590771,-0.48201817500657,
-0.358635861766521));
#39823=CARTESIAN_POINT('Ctrl Pts',(0.634054255725814,-0.209332177210148,
-0.348260389515803));
#39824=CARTESIAN_POINT('Ctrl Pts',(0.658229503614937,0.112154715424475,
-0.337884917265084));
#39825=CARTESIAN_POINT('Ctrl Pts',(0.528953957349416,0.407495362778231,
-0.327509445014367));
#39826=CARTESIAN_POINT('Ctrl Pts',(0.276365183140412,0.607838008857103,
-0.317133972763648));
#39827=CARTESIAN_POINT('Ctrl Pts',(-0.040651661531787,0.666477458287253,
-0.30675850051293));
#39828=CARTESIAN_POINT('Ctrl Pts',(-0.348191523276064,0.569743294931616,
-0.296383028262211));
#39829=CARTESIAN_POINT('Ctrl Pts',(-0.574558685491881,0.340186827082857,
-0.286007556011493));
#39830=CARTESIAN_POINT('Ctrl Pts',(-0.666980945237279,0.0313237625272405,
-0.275632083760775));
#39831=CARTESIAN_POINT('Ctrl Pts',(-0.60391221743454,-0.284841694627466,
-0.265256611510056));
#39832=CARTESIAN_POINT('Ctrl Pts',(-0.400055498194385,-0.534602999246615,
-0.254881139259338));
#39833=CARTESIAN_POINT('Ctrl Pts',(-0.102935209247226,-0.659734098192411,
-0.24450566700862));
#39834=CARTESIAN_POINT('Ctrl Pts',(0.218182015307551,-0.631063713343416,
-0.234130194757901));
#39835=CARTESIAN_POINT('Ctrl Pts',(0.488435208193123,-0.455275460354312,
-0.223754722507183));
#39836=CARTESIAN_POINT('Ctrl Pts',(0.644821179064956,-0.173350677448309,
-0.213379250256465));
#39837=CARTESIAN_POINT('Ctrl Pts',(0.65088217585303,0.148987316632804,-0.203003778005747));
#39838=CARTESIAN_POINT('Ctrl Pts',(0.505205269294179,0.436591293146462,
-0.192628305755028));
#39839=CARTESIAN_POINT('Ctrl Pts',(0.241751518866823,0.622416447653164,
-0.18225283350431));
#39840=CARTESIAN_POINT('Ctrl Pts',(-0.0780608048519096,0.663135382918645,
-0.171877361253591));
#39841=CARTESIAN_POINT('Ctrl Pts',(-0.379675341865185,0.549268581130195,
-0.161501889002874));
#39842=CARTESIAN_POINT('Ctrl Pts',(-0.592776947792401,0.307335268506549,
-0.151126416752155));
#39843=CARTESIAN_POINT('Ctrl Pts',(-0.667687464951409,-0.00621127295214926,
-0.140750944501437));
#39844=CARTESIAN_POINT('Ctrl Pts',(-0.586940939264991,-0.318381324725216,
-0.130375472250718));
#39845=CARTESIAN_POINT('Ctrl Pts',(-0.441883170803417,-0.476893507297812,
-0.12345849075024));
#39846=CARTESIAN_POINT('Ctrl Pts',(-0.354984681166936,-0.5345961871503,
-0.12));
#39847=CARTESIAN_POINT('Ctrl Pts',(0.419902519832407,0.403180862557734,
-0.75727273924394));
#39848=CARTESIAN_POINT('Ctrl Pts',(0.352813337597515,0.473052523864309,
-0.753732335137029));
#39849=CARTESIAN_POINT('Ctrl Pts',(0.183146826434185,0.578585044749363,
-0.746651526923207));
#39850=CARTESIAN_POINT('Ctrl Pts',(-0.116229043222437,0.595630586916603,
-0.736030314602476));
#39851=CARTESIAN_POINT('Ctrl Pts',(-0.38716554463002,0.467313281319197,
-0.725409102281742));
#39852=CARTESIAN_POINT('Ctrl Pts',(-0.5636424333859,0.224934817531868,-0.714787889961011));
#39853=CARTESIAN_POINT('Ctrl Pts',(-0.602534986633661,-0.0723403849529277,
-0.704166677640278));
#39854=CARTESIAN_POINT('Ctrl Pts',(-0.494377117526733,-0.351960929022743,
-0.693545465319546));
#39855=CARTESIAN_POINT('Ctrl Pts',(-0.265553394359715,-0.545678585605523,
-0.682924252998813));
#39856=CARTESIAN_POINT('Ctrl Pts',(0.0280810564139534,-0.606214132210099,
-0.672303040678082));
#39857=CARTESIAN_POINT('Ctrl Pts',(0.314862960821169,-0.518792316784799,
-0.661681828357348));
#39858=CARTESIAN_POINT('Ctrl Pts',(0.524796465182481,-0.30475021433233,
-0.651060616036617));
#39859=CARTESIAN_POINT('Ctrl Pts',(0.60664446863493,-0.0163284320554081,
-0.640439403715884));
#39860=CARTESIAN_POINT('Ctrl Pts',(0.540430098503603,0.27607856963071,-0.629818191395151));
#39861=CARTESIAN_POINT('Ctrl Pts',(0.342314351095128,0.501103761813076,
-0.619196979074419));
#39862=CARTESIAN_POINT('Ctrl Pts',(0.0606507420151454,0.603825781241362,
-0.608575766753688));
#39863=CARTESIAN_POINT('Ctrl Pts',(-0.235815726583716,0.55917352432788,
-0.597954554432955));
#39864=CARTESIAN_POINT('Ctrl Pts',(-0.474727237871055,0.378045153975223,
-0.587333342112222));
#39865=CARTESIAN_POINT('Ctrl Pts',(-0.597773230616621,0.104648229800698,
-0.576712129791491));
#39866=CARTESIAN_POINT('Ctrl Pts',(-0.574922177901191,-0.194289931772878,
-0.566090917470757));
#39867=CARTESIAN_POINT('Ctrl Pts',(-0.41175127661568,-0.445808225543571,
-0.555469705150026));
#39868=CARTESIAN_POINT('Ctrl Pts',(-0.148085250655247,-0.588519198041721,
-0.544848492829293));
#39869=CARTESIAN_POINT('Ctrl Pts',(0.151723579920602,-0.587591731726026,
-0.53422728050856));
#39870=CARTESIAN_POINT('Ctrl Pts',(0.414501607921562,-0.443252191094065,
-0.523606068187829));
#39871=CARTESIAN_POINT('Ctrl Pts',(0.576113244100042,-0.190729174156685,
-0.512984855867096));
#39872=CARTESIAN_POINT('Ctrl Pts',(0.597114332253383,0.108344645017158,
-0.502363643546364));
#39873=CARTESIAN_POINT('Ctrl Pts',(0.472379188307862,0.38097505213334,-0.491742431225632));
#39874=CARTESIAN_POINT('Ctrl Pts',(0.232351613210618,0.560621811678453,
-0.481121218904899));
#39875=CARTESIAN_POINT('Ctrl Pts',(-0.0643854508469475,0.603438979194421,
-0.470500006584167));
#39876=CARTESIAN_POINT('Ctrl Pts',(-0.345408115665845,0.498976273508361,
-0.459878794263435));
#39877=CARTESIAN_POINT('Ctrl Pts',(-0.542127867956924,0.272729651259685,
-0.449257581942702));
#39878=CARTESIAN_POINT('Ctrl Pts',(-0.606531799752129,-0.0200814287731599,
-0.43863636962197));
#39879=CARTESIAN_POINT('Ctrl Pts',(-0.522901001209041,-0.307991283685645,
-0.428015157301237));
#39880=CARTESIAN_POINT('Ctrl Pts',(-0.311647036430625,-0.52073046058026,
-0.417393944980506));
#39881=CARTESIAN_POINT('Ctrl Pts',(-0.0243301430172896,-0.606376229772182,
-0.406772732659772));
#39882=CARTESIAN_POINT('Ctrl Pts',(0.268924948789863,-0.54402523821012,
-0.396151520339041));
#39883=CARTESIAN_POINT('Ctrl Pts',(0.49654418722808,-0.348895339642708,
-0.385530308018308));
#39884=CARTESIAN_POINT('Ctrl Pts',(0.602973102433286,-0.0686114103358565,
-0.374909095697576));
#39885=CARTESIAN_POINT('Ctrl Pts',(0.562235849856194,0.22841833778935,-0.364287883376844));
#39886=CARTESIAN_POINT('Ctrl Pts',(0.384275070866584,0.469698581847689,
-0.353666671056111));
#39887=CARTESIAN_POINT('Ctrl Pts',(0.112525216897816,0.596340643809236,
-0.343045458735379));
#39888=CARTESIAN_POINT('Ctrl Pts',(-0.186688391221607,0.577435305907412,
-0.332424246414646));
#39889=CARTESIAN_POINT('Ctrl Pts',(-0.440337420784613,0.417596747609107,
-0.321803034093914));
#39890=CARTESIAN_POINT('Ctrl Pts',(-0.58651437550708,0.155836374298491,
-0.311181821773182));
#39891=CARTESIAN_POINT('Ctrl Pts',(-0.589542202382296,-0.14395860117576,
-0.30056060945245));
#39892=CARTESIAN_POINT('Ctrl Pts',(-0.44868191070889,-0.408617953378765,
-0.289939397131717));
#39893=CARTESIAN_POINT('Ctrl Pts',(-0.198312919647183,-0.573546923201999,
-0.279318184810985));
#39894=CARTESIAN_POINT('Ctrl Pts',(0.100457810451271,-0.598491699957539,
-0.268696972490252));
#39895=CARTESIAN_POINT('Ctrl Pts',(0.374710067503894,-0.477364075292773,
-0.25807576016952));
#39896=CARTESIAN_POINT('Ctrl Pts',(0.557507719479534,-0.239727367437853,
-0.247454547848788));
#39897=CARTESIAN_POINT('Ctrl Pts',(0.604235901607852,0.0564190059013063,
-0.236833335528056));
#39898=CARTESIAN_POINT('Ctrl Pts',(0.503489562133039,0.338795342097125,
-0.226212123207323));
#39899=CARTESIAN_POINT('Ctrl Pts',(0.279858047502047,0.538482706593586,
-0.215590910886591));
#39900=CARTESIAN_POINT('Ctrl Pts',(-0.0120783079673112,0.606743961071895,
-0.204969698565858));
#39901=CARTESIAN_POINT('Ctrl Pts',(-0.301065603751776,0.526918614476648,
-0.194348486245126));
#39902=CARTESIAN_POINT('Ctrl Pts',(-0.516574810615386,0.318489709300428,
-0.183727273924394));
#39903=CARTESIAN_POINT('Ctrl Pts',(-0.606000393860149,0.0323274504734039,
-0.173106061603662));
#39904=CARTESIAN_POINT('Ctrl Pts',(-0.54752982679742,-0.261724193796561,
-0.162484849282929));
#39905=CARTESIAN_POINT('Ctrl Pts',(-0.355407358238332,-0.491898842808179,
-0.151863636962197));
#39906=CARTESIAN_POINT('Ctrl Pts',(-0.076576683950909,-0.602014117802982,
-0.141242424641464));
#39907=CARTESIAN_POINT('Ctrl Pts',(0.221016091685922,-0.565203769676402,
-0.130621212320732));
#39908=CARTESIAN_POINT('Ctrl Pts',(0.383330620179427,-0.448679815853072,
-0.123540404106911));
#39909=CARTESIAN_POINT('Ctrl Pts',(0.44565123783516,-0.374523575106285,
-0.12));
#39910=CARTESIAN_POINT('Ctrl Pts',(0.434231400019489,0.416939127870406,
-0.746931826162627));
#39911=CARTESIAN_POINT('Ctrl Pts',(0.36485284630267,0.489195110813665,-0.743391422055716));
#39912=CARTESIAN_POINT('Ctrl Pts',(0.189396583958067,0.598328855259381,
-0.736310613841894));
#39913=CARTESIAN_POINT('Ctrl Pts',(-0.120195278136336,0.615956064646757,
-0.725689401521163));
#39914=CARTESIAN_POINT('Ctrl Pts',(-0.40037729840512,0.483260020625564,
-0.715068189200429));
#39915=CARTESIAN_POINT('Ctrl Pts',(-0.582876337720566,0.232610561063019,
-0.704446976879698));
#39916=CARTESIAN_POINT('Ctrl Pts',(-0.623096072181431,-0.0748089500596382,
-0.693825764558965));
#39917=CARTESIAN_POINT('Ctrl Pts',(-0.511247391339576,-0.363971349880692,
-0.683204552238233));
#39918=CARTESIAN_POINT('Ctrl Pts',(-0.274615218453011,-0.564299486182443,
-0.6725833399175));
#39919=CARTESIAN_POINT('Ctrl Pts',(0.0290393028494424,-0.62690076603078,
-0.661962127596768));
#39920=CARTESIAN_POINT('Ctrl Pts',(0.325607439427196,-0.536495742218289,
-0.651340915276035));
#39921=CARTESIAN_POINT('Ctrl Pts',(0.54270477798614,-0.315149602528186,
-0.640719702955303));
#39922=CARTESIAN_POINT('Ctrl Pts',(0.627345787385518,-0.0168856283938771,
-0.630098490634571));
#39923=CARTESIAN_POINT('Ctrl Pts',(0.558871898124242,0.285499557978287,
-0.619477278313838));
#39924=CARTESIAN_POINT('Ctrl Pts',(0.353995589219439,0.518203577663625,
-0.608856065993106));
#39925=CARTESIAN_POINT('Ctrl Pts',(0.0627204062218264,0.624430914253499,
-0.598234853672375));
#39926=CARTESIAN_POINT('Ctrl Pts',(-0.243862773535938,0.578254930262477,
-0.587613641351641));
#39927=CARTESIAN_POINT('Ctrl Pts',(-0.490926973266102,0.390945680789826,
-0.576992429030909));
#39928=CARTESIAN_POINT('Ctrl Pts',(-0.618171824566399,0.108219277545785,
-0.566371216710177));
#39929=CARTESIAN_POINT('Ctrl Pts',(-0.594540995638531,-0.200919939982977,
-0.555750004389445));
#39930=CARTESIAN_POINT('Ctrl Pts',(-0.425802001321639,-0.461021119842892,
-0.545128792068712));
#39931=CARTESIAN_POINT('Ctrl Pts',(-0.153138556396207,-0.60860200459383,
-0.53450757974798));
#39932=CARTESIAN_POINT('Ctrl Pts',(0.156901041106368,-0.607642889137947,
-0.523886367427247));
#39933=CARTESIAN_POINT('Ctrl Pts',(0.428646185762228,-0.458377862503188,
-0.513265155106516));
#39934=CARTESIAN_POINT('Ctrl Pts',(0.595772706139457,-0.197237674000322,
-0.502643942785783));
#39935=CARTESIAN_POINT('Ctrl Pts',(0.617490441756758,0.112041830349559,
-0.492022730465051));
#39936=CARTESIAN_POINT('Ctrl Pts',(0.488498798151678,0.393975559676054,
-0.481401518144319));
#39937=CARTESIAN_POINT('Ctrl Pts',(0.240280449713669,0.579752639407259,
-0.470780305823586));
#39938=CARTESIAN_POINT('Ctrl Pts',(-0.0665825593838184,0.624030912856886,
-0.460159093502854));
#39939=CARTESIAN_POINT('Ctrl Pts',(-0.357194926345134,0.516003490306564,
-0.449537881182121));
#39940=CARTESIAN_POINT('Ctrl Pts',(-0.560627602774265,0.282036360107072,
-0.438916668861389));
#39941=CARTESIAN_POINT('Ctrl Pts',(-0.627229273755788,-0.0207666935031524,
-0.428295456540656));
#39942=CARTESIAN_POINT('Ctrl Pts',(-0.540744632628591,-0.318501271109293,
-0.417674244219924));
#39943=CARTESIAN_POINT('Ctrl Pts',(-0.322281773863149,-0.538500023816976,
-0.407053031899192));
#39944=CARTESIAN_POINT('Ctrl Pts',(-0.0251603921531334,-0.627068395058943,
-0.39643181957846));
#39945=CARTESIAN_POINT('Ctrl Pts',(0.278101824823055,-0.562589719462036,
-0.385810607257727));
#39946=CARTESIAN_POINT('Ctrl Pts',(0.513488410780781,-0.36080114940438,
-0.375189394936995));
#39947=CARTESIAN_POINT('Ctrl Pts',(0.623549138376695,-0.0709527267884497,
-0.364568182616262));
#39948=CARTESIAN_POINT('Ctrl Pts',(0.581421755510406,0.236212954016045,
-0.35394697029553));
#39949=CARTESIAN_POINT('Ctrl Pts',(0.397388189243505,0.485726717868459,
-0.343325757974798));
#39950=CARTESIAN_POINT('Ctrl Pts',(0.116365061325512,0.616690351734874,
-0.332704545654065));
#39951=CARTESIAN_POINT('Ctrl Pts',(-0.193059002170075,0.597139882382544,
-0.322083333333333));
#39952=CARTESIAN_POINT('Ctrl Pts',(-0.455363627692896,0.431846944929651,
-0.311462121012601));
#39953=CARTESIAN_POINT('Ctrl Pts',(-0.606528768890564,0.161154181719611,
-0.300840908691869));
#39954=CARTESIAN_POINT('Ctrl Pts',(-0.609659918242957,-0.148871087885701,
-0.290219696371136));
#39955=CARTESIAN_POINT('Ctrl Pts',(-0.463992867507207,-0.422561755617893,
-0.279598484050404));
#39956=CARTESIAN_POINT('Ctrl Pts',(-0.205080209508431,-0.593118811333345,
-0.268977271729672));
#39957=CARTESIAN_POINT('Ctrl Pts',(0.10388586306307,-0.618914811171724,
-0.258356059408939));
#39958=CARTESIAN_POINT('Ctrl Pts',(0.387496786822224,-0.493653790923003,
-0.247734847088207));
#39959=CARTESIAN_POINT('Ctrl Pts',(0.576532280987245,-0.247907896401938,
-0.237113634767475));
#39960=CARTESIAN_POINT('Ctrl Pts',(0.624855029691027,0.058344265068974,
-0.226492422446742));
#39961=CARTESIAN_POINT('Ctrl Pts',(0.520670791753022,0.35035649649741,-0.21587121012601));
#39962=CARTESIAN_POINT('Ctrl Pts',(0.289408007892015,0.55685805282555,-0.205249997805277));
#39963=CARTESIAN_POINT('Ctrl Pts',(-0.0124904717899899,0.627448674932399,
-0.194628785484545));
#39964=CARTESIAN_POINT('Ctrl Pts',(-0.311339257185273,0.544899344142648,
-0.184007573163813));
#39965=CARTESIAN_POINT('Ctrl Pts',(-0.534202565199775,0.329357948165023,
-0.17338636084308));
#39966=CARTESIAN_POINT('Ctrl Pts',(-0.626679734008933,0.0334306021400623,
-0.162765148522348));
#39967=CARTESIAN_POINT('Ctrl Pts',(-0.566213899686921,-0.270655349095339,
-0.152143936201616));
#39968=CARTESIAN_POINT('Ctrl Pts',(-0.36753538608593,-0.508684547227327,
-0.141522723880884));
#39969=CARTESIAN_POINT('Ctrl Pts',(-0.0791898098018671,-0.622557429065733,
-0.130901511560151));
#39970=CARTESIAN_POINT('Ctrl Pts',(0.228558111434812,-0.584490953521386,
-0.120280299239419));
#39971=CARTESIAN_POINT('Ctrl Pts',(0.396411509836348,-0.463990701165897,
-0.113199491025597));
#39972=CARTESIAN_POINT('Ctrl Pts',(0.460858775038588,-0.387303930501811,
-0.109659086918687));
#39973=CARTESIAN_POINT('Ctrl Pts',(0.44856028020657,0.430697393183078,-0.736590913081313));
#39974=CARTESIAN_POINT('Ctrl Pts',(0.376892355007826,0.505337697763021,
-0.733050508974403));
#39975=CARTESIAN_POINT('Ctrl Pts',(0.195646341481949,0.618072665769401,
-0.725969700760581));
#39976=CARTESIAN_POINT('Ctrl Pts',(-0.124161513050235,0.63628154237691,
-0.715348488439849));
#39977=CARTESIAN_POINT('Ctrl Pts',(-0.41358905218022,0.499206759931933,
-0.704727276119116));
#39978=CARTESIAN_POINT('Ctrl Pts',(-0.60211024205523,0.240286304594168,
-0.694106063798384));
#39979=CARTESIAN_POINT('Ctrl Pts',(-0.643657157729202,-0.0772775151663482,
-0.683484851477652));
#39980=CARTESIAN_POINT('Ctrl Pts',(-0.528117665152417,-0.375981770738642,
-0.672863639156919));
#39981=CARTESIAN_POINT('Ctrl Pts',(-0.283677042546308,-0.582920386759363,
-0.662242426836187));
#39982=CARTESIAN_POINT('Ctrl Pts',(0.0299975492849321,-0.647587399851459,
-0.651621214515455));
#39983=CARTESIAN_POINT('Ctrl Pts',(0.336351918033223,-0.55419916765178,
-0.641000002194723));
#39984=CARTESIAN_POINT('Ctrl Pts',(0.5606130907898,-0.325548990724041,-0.63037878987399));
#39985=CARTESIAN_POINT('Ctrl Pts',(0.648047106136105,-0.0174428247323467,
-0.619757577553258));
#39986=CARTESIAN_POINT('Ctrl Pts',(0.577313697744881,0.294920546325864,
-0.609136365232525));
#39987=CARTESIAN_POINT('Ctrl Pts',(0.36567682734375,0.535303393514173,-0.598515152911793));
#39988=CARTESIAN_POINT('Ctrl Pts',(0.0647900704285079,0.645036047265636,
-0.587893940591061));
#39989=CARTESIAN_POINT('Ctrl Pts',(-0.25190982048816,0.597336336197074,
-0.577272728270329));
#39990=CARTESIAN_POINT('Ctrl Pts',(-0.507126708661149,0.40384620760443,
-0.566651515949596));
#39991=CARTESIAN_POINT('Ctrl Pts',(-0.638570418516177,0.111790325290873,
-0.556030303628864));
#39992=CARTESIAN_POINT('Ctrl Pts',(-0.614159813375872,-0.207549948193075,
-0.545409091308131));
#39993=CARTESIAN_POINT('Ctrl Pts',(-0.439852726027598,-0.476234014142214,
-0.534787878987399));
#39994=CARTESIAN_POINT('Ctrl Pts',(-0.158191862137167,-0.628684811145938,
-0.524166666666666));
#39995=CARTESIAN_POINT('Ctrl Pts',(0.162078502292133,-0.627694046549866,
-0.513545454345935));
#39996=CARTESIAN_POINT('Ctrl Pts',(0.442790763602892,-0.473503533912313,
-0.502924242025202));
#39997=CARTESIAN_POINT('Ctrl Pts',(0.615432168178873,-0.203746173843959,
-0.49230302970447));
#39998=CARTESIAN_POINT('Ctrl Pts',(0.637866551260131,0.11573901568196,-0.481681817383737));
#39999=CARTESIAN_POINT('Ctrl Pts',(0.504618407995495,0.406976067218768,
-0.471060605063006));
#40000=CARTESIAN_POINT('Ctrl Pts',(0.248209286216719,0.598883467136063,
-0.460439392742272));
#40001=CARTESIAN_POINT('Ctrl Pts',(-0.0687796679206887,0.644622846519354,
-0.449818180421541));
#40002=CARTESIAN_POINT('Ctrl Pts',(-0.368981737024425,0.533030707104764,
-0.439196968100808));
#40003=CARTESIAN_POINT('Ctrl Pts',(-0.579127337591605,0.291343068954459,
-0.428575755780076));
#40004=CARTESIAN_POINT('Ctrl Pts',(-0.64792674775945,-0.021451958233145,
-0.417954543459343));
#40005=CARTESIAN_POINT('Ctrl Pts',(-0.558588264048139,-0.329011258532942,
-0.407333331138611));
#40006=CARTESIAN_POINT('Ctrl Pts',(-0.332916511295674,-0.556269587053691,
-0.396712118817879));
#40007=CARTESIAN_POINT('Ctrl Pts',(-0.0259906412889762,-0.647760560345705,
-0.386090906497146));
#40008=CARTESIAN_POINT('Ctrl Pts',(0.287278700856247,-0.581154200713952,
-0.375469694176414));
#40009=CARTESIAN_POINT('Ctrl Pts',(0.530432634333482,-0.372706959166052,
-0.364848481855682));
#40010=CARTESIAN_POINT('Ctrl Pts',(0.644125174320103,-0.0732940432410428,
-0.354227269534949));
#40011=CARTESIAN_POINT('Ctrl Pts',(0.600607661164621,0.24400757024274,-0.343606057214217));
#40012=CARTESIAN_POINT('Ctrl Pts',(0.410501307620425,0.501754853889229,
-0.332984844893485));
#40013=CARTESIAN_POINT('Ctrl Pts',(0.120204905753208,0.637040059660513,
-0.322363632572752));
#40014=CARTESIAN_POINT('Ctrl Pts',(-0.199429613118542,0.616844458857675,
-0.31174242025202));
#40015=CARTESIAN_POINT('Ctrl Pts',(-0.470389834601179,0.446097142250195,
-0.301121207931288));
#40016=CARTESIAN_POINT('Ctrl Pts',(-0.626543162274047,0.166471989140732,
-0.290499995610555));
#40017=CARTESIAN_POINT('Ctrl Pts',(-0.629777634103618,-0.153783574595641,
-0.279878783289823));
#40018=CARTESIAN_POINT('Ctrl Pts',(-0.479303824305524,-0.436505557857022,
-0.269257570969091));
#40019=CARTESIAN_POINT('Ctrl Pts',(-0.211847499369681,-0.612690699464692,
-0.258636358648358));
#40020=CARTESIAN_POINT('Ctrl Pts',(0.107313915674871,-0.639337922385911,
-0.248015146327626));
#40021=CARTESIAN_POINT('Ctrl Pts',(0.400283506140554,-0.509943506553232,
-0.237393934006894));
#40022=CARTESIAN_POINT('Ctrl Pts',(0.595556842494959,-0.256088425366023,
-0.226772721686161));
#40023=CARTESIAN_POINT('Ctrl Pts',(0.6454741577742,0.0602695242366418,-0.216151509365429));
#40024=CARTESIAN_POINT('Ctrl Pts',(0.537852021373006,0.361917650897694,
-0.205530297044696));
#40025=CARTESIAN_POINT('Ctrl Pts',(0.298957968281983,0.575233399057514,
-0.194909084723964));
#40026=CARTESIAN_POINT('Ctrl Pts',(-0.0129026356126682,0.648153388792901,
-0.184287872403232));
#40027=CARTESIAN_POINT('Ctrl Pts',(-0.321612910618771,0.562880073808648,
-0.1736666600825));
#40028=CARTESIAN_POINT('Ctrl Pts',(-0.551830319784164,0.340226187029618,
-0.163045447761767));
#40029=CARTESIAN_POINT('Ctrl Pts',(-0.647359074157716,0.0345337538067202,
-0.152424235441035));
#40030=CARTESIAN_POINT('Ctrl Pts',(-0.584897972576422,-0.279586504394117,
-0.141803023120302));
#40031=CARTESIAN_POINT('Ctrl Pts',(-0.379663413933528,-0.525470251646476,
-0.131181810799571));
#40032=CARTESIAN_POINT('Ctrl Pts',(-0.0818029356528252,-0.643100740328482,
-0.120560598478838));
#40033=CARTESIAN_POINT('Ctrl Pts',(0.236100131183702,-0.603778137366371,
-0.109939386158106));
#40034=CARTESIAN_POINT('Ctrl Pts',(0.409492399493268,-0.479301586478722,
-0.102858577944284));
#40035=CARTESIAN_POINT('Ctrl Pts',(0.476066312242016,-0.400084285897338,
-0.0993181738373734));
#40036=CARTESIAN_POINT('Ctrl Pts',(0.462889160393651,0.44445565849575,-0.72625));
#40037=CARTESIAN_POINT('Ctrl Pts',(0.388931863712981,0.521480284712376,
-0.722709595893089));
#40038=CARTESIAN_POINT('Ctrl Pts',(0.20189609900583,0.63781647627942,-0.715628787679269));
#40039=CARTESIAN_POINT('Ctrl Pts',(-0.128127747964134,0.656607020107064,
-0.705007575358535));
#40040=CARTESIAN_POINT('Ctrl Pts',(-0.42680080595532,0.515153499238301,
-0.694386363037804));
#40041=CARTESIAN_POINT('Ctrl Pts',(-0.621344146389896,0.247962048125318,
-0.68376515071707));
#40042=CARTESIAN_POINT('Ctrl Pts',(-0.664218243276972,-0.0797460802730583,
-0.673143938396339));
#40043=CARTESIAN_POINT('Ctrl Pts',(-0.544987938965259,-0.387992191596592,
-0.662522726075605));
#40044=CARTESIAN_POINT('Ctrl Pts',(-0.292738866639604,-0.601541287336283,
-0.651901513754874));
#40045=CARTESIAN_POINT('Ctrl Pts',(0.0309557957204211,-0.66827403367214,
-0.641280301434142));
#40046=CARTESIAN_POINT('Ctrl Pts',(0.34709639663925,-0.571902593085269,
-0.630659089113409));
#40047=CARTESIAN_POINT('Ctrl Pts',(0.578521403593459,-0.335948378919897,
-0.620037876792677));
#40048=CARTESIAN_POINT('Ctrl Pts',(0.668748424886692,-0.018000021070816,
-0.609416664471945));
#40049=CARTESIAN_POINT('Ctrl Pts',(0.59575549736552,0.30434153467344,-0.598795452151212));
#40050=CARTESIAN_POINT('Ctrl Pts',(0.377358065468061,0.552403209364722,
-0.58817423983048));
#40051=CARTESIAN_POINT('Ctrl Pts',(0.0668597346351892,0.665641180277773,
-0.577553027509748));
#40052=CARTESIAN_POINT('Ctrl Pts',(-0.259956867440381,0.61641774213167,
-0.566931815189015));
#40053=CARTESIAN_POINT('Ctrl Pts',(-0.523326444056197,0.416746734419033,
-0.556310602868283));
#40054=CARTESIAN_POINT('Ctrl Pts',(-0.658969012465955,0.115361373035961,
-0.54568939054755));
#40055=CARTESIAN_POINT('Ctrl Pts',(-0.633778631113213,-0.214179956403173,
-0.535068178226818));
#40056=CARTESIAN_POINT('Ctrl Pts',(-0.453903450733557,-0.491446908441536,
-0.524446965906085));
#40057=CARTESIAN_POINT('Ctrl Pts',(-0.163245167878128,-0.648767617698046,
-0.513825753585354));
#40058=CARTESIAN_POINT('Ctrl Pts',(0.167255963477899,-0.647745203961788,
-0.50320454126462));
#40059=CARTESIAN_POINT('Ctrl Pts',(0.456935341443556,-0.488629205321436,
-0.492583328943889));
#40060=CARTESIAN_POINT('Ctrl Pts',(0.635091630218289,-0.210254673687596,
-0.481962116623156));
#40061=CARTESIAN_POINT('Ctrl Pts',(0.658242660763504,0.119436201014362,
-0.471340904302425));
#40062=CARTESIAN_POINT('Ctrl Pts',(0.520738017839312,0.419976574761482,
-0.460719691981691));
#40063=CARTESIAN_POINT('Ctrl Pts',(0.256138122719768,0.618014294864869,
-0.45009847966096));
#40064=CARTESIAN_POINT('Ctrl Pts',(-0.0709767764575589,0.66521478018182,
-0.439477267340227));
#40065=CARTESIAN_POINT('Ctrl Pts',(-0.380768547703715,0.550057923902966,
-0.428856055019495));
#40066=CARTESIAN_POINT('Ctrl Pts',(-0.597627072408945,0.300649777801846,
-0.418234842698762));
#40067=CARTESIAN_POINT('Ctrl Pts',(-0.668624221763112,-0.0221372229631371,
-0.40761363037803));
#40068=CARTESIAN_POINT('Ctrl Pts',(-0.576431895467687,-0.339521245956591,
-0.396992418057298));
#40069=CARTESIAN_POINT('Ctrl Pts',(-0.343551248728199,-0.574039150290406,
-0.386371205736565));
#40070=CARTESIAN_POINT('Ctrl Pts',(-0.0268208904248193,-0.668452725632466,
-0.375749993415833));
#40071=CARTESIAN_POINT('Ctrl Pts',(0.296455576889439,-0.599718681965868,
-0.365128781095101));
#40072=CARTESIAN_POINT('Ctrl Pts',(0.547376857886183,-0.384612768927724,
-0.354507568774369));
#40073=CARTESIAN_POINT('Ctrl Pts',(0.664701210263511,-0.0756353596936366,
-0.343886356453636));
#40074=CARTESIAN_POINT('Ctrl Pts',(0.619793566818835,0.251802186469436,
-0.333265144132904));
#40075=CARTESIAN_POINT('Ctrl Pts',(0.423614425997345,0.517782989909997,
-0.322643931812171));
#40076=CARTESIAN_POINT('Ctrl Pts',(0.124044750180905,0.657389767586153,
-0.312022719491439));
#40077=CARTESIAN_POINT('Ctrl Pts',(-0.20580022406701,0.636549035332806,
-0.301401507170707));
#40078=CARTESIAN_POINT('Ctrl Pts',(-0.485416041509462,0.46034733957074,
-0.290780294849974));
#40079=CARTESIAN_POINT('Ctrl Pts',(-0.64655755565753,0.171789796561853,
-0.280159082529243));
#40080=CARTESIAN_POINT('Ctrl Pts',(-0.649895349964279,-0.158696061305582,
-0.26953787020851));
#40081=CARTESIAN_POINT('Ctrl Pts',(-0.49461478110384,-0.45044936009615,
-0.258916657887777));
#40082=CARTESIAN_POINT('Ctrl Pts',(-0.218614789230929,-0.632262587596038,
-0.248295445567045));
#40083=CARTESIAN_POINT('Ctrl Pts',(0.11074196828667,-0.659761033600097,
-0.237674233246313));
#40084=CARTESIAN_POINT('Ctrl Pts',(0.413070225458884,-0.526233222183462,
-0.22705302092558));
#40085=CARTESIAN_POINT('Ctrl Pts',(0.614581404002671,-0.264268954330109,
-0.216431808604848));
#40086=CARTESIAN_POINT('Ctrl Pts',(0.666093285857374,0.0621947834043098,
-0.205810596284116));
#40087=CARTESIAN_POINT('Ctrl Pts',(0.555033250992989,0.373478805297979,
-0.195189383963383));
#40088=CARTESIAN_POINT('Ctrl Pts',(0.308507928671951,0.593608745289479,
-0.184568171642651));
#40089=CARTESIAN_POINT('Ctrl Pts',(-0.0133147994353463,0.668858102653405,
-0.173946959321918));
#40090=CARTESIAN_POINT('Ctrl Pts',(-0.331886564052269,0.580860803474647,
-0.163325747001187));
#40091=CARTESIAN_POINT('Ctrl Pts',(-0.569458074368552,0.351094425894214,
-0.152704534680454));
#40092=CARTESIAN_POINT('Ctrl Pts',(-0.668038414306502,0.0356369054733784,
-0.142083322359722));
#40093=CARTESIAN_POINT('Ctrl Pts',(-0.603582045465921,-0.288517659692895,
-0.131462110038989));
#40094=CARTESIAN_POINT('Ctrl Pts',(-0.391791441781126,-0.542255956065624,
-0.120840897718257));
#40095=CARTESIAN_POINT('Ctrl Pts',(-0.084416061503783,-0.663644051591233,
-0.110219685397525));
#40096=CARTESIAN_POINT('Ctrl Pts',(0.243642150932592,-0.623065321211354,
-0.0995984730767924));
#40097=CARTESIAN_POINT('Ctrl Pts',(0.422573289150189,-0.494612471791547,
-0.0925176648629709));
#40098=CARTESIAN_POINT('Ctrl Pts',(0.491273849445444,-0.412864641292864,
-0.0889772607560602));
#40099=CARTESIAN_POINT('',(0.445651237835157,-0.374523575106288,-0.12));
#40100=CARTESIAN_POINT('Ctrl Pts',(-0.355015686975108,-0.534630012137314,
-0.12));
#40101=CARTESIAN_POINT('Ctrl Pts',(-0.327773074693179,-0.55029714351302,
-0.12));
#40102=CARTESIAN_POINT('Ctrl Pts',(-0.299464346019529,-0.563882057522015,
-0.12));
#40103=CARTESIAN_POINT('Ctrl Pts',(-0.270342974496624,-0.575326154153575,
-0.12));
#40104=CARTESIAN_POINT('Ctrl Pts',(-0.239781266261733,-0.587336273319513,
-0.12));
#40105=CARTESIAN_POINT('Ctrl Pts',(-0.208323126958149,-0.596989401715483,
-0.12));
#40106=CARTESIAN_POINT('Ctrl Pts',(-0.176246299508229,-0.604158357140015,
-0.12));
#40107=CARTESIAN_POINT('Ctrl Pts',(-0.161891963957468,-0.607366454694951,
-0.12));
#40108=CARTESIAN_POINT('Ctrl Pts',(-0.147413669750131,-0.610076237005704,
-0.12));
#40109=CARTESIAN_POINT('Ctrl Pts',(-0.132836594213696,-0.612272034267081,
-0.12));
#40110=CARTESIAN_POINT('Ctrl Pts',(-0.124920402928789,-0.613464478602056,
-0.12));
#40111=CARTESIAN_POINT('Ctrl Pts',(-0.116973279753054,-0.61450528464571,
-0.12));
#40112=CARTESIAN_POINT('Ctrl Pts',(-0.10902091463483,-0.615389836202277,
-0.12));
#40113=CARTESIAN_POINT('Ctrl Pts',(-0.0988935419311309,-0.616516316583374,
-0.12));
#40114=CARTESIAN_POINT('Ctrl Pts',(-0.0887499005304207,-0.617390725698137,
-0.12));
#40115=CARTESIAN_POINT('Ctrl Pts',(-0.0785983814394652,-0.61801027904089,
-0.12));
#40116=CARTESIAN_POINT('Ctrl Pts',(-0.0478707602737524,-0.61988560432349,
-0.12));
#40117=CARTESIAN_POINT('Ctrl Pts',(-0.0170704984466291,-0.619429816208118,
-0.12));
#40118=CARTESIAN_POINT('Ctrl Pts',(0.0135460552793042,-0.616696753535392,
-0.12));
#40119=CARTESIAN_POINT('Ctrl Pts',(0.0363940854309653,-0.614657167404575,
-0.12));
#40120=CARTESIAN_POINT('Ctrl Pts',(0.0591399790301594,-0.611348192348154,
-0.12));
#40121=CARTESIAN_POINT('Ctrl Pts',(0.0816716129165091,-0.606774115783264,
-0.12));
#40122=CARTESIAN_POINT('Ctrl Pts',(0.0917546790591232,-0.604727184043747,
-0.12));
#40123=CARTESIAN_POINT('Ctrl Pts',(0.101794739333339,-0.602426702231052,
-0.12));
#40124=CARTESIAN_POINT('Ctrl Pts',(0.111781158534424,-0.599872121726624,
-0.12));
#40125=CARTESIAN_POINT('Ctrl Pts',(0.118182233540509,-0.598234691824207,
-0.12));
#40126=CARTESIAN_POINT('Ctrl Pts',(0.124557115310639,-0.59649382554347,
-0.12));
#40127=CARTESIAN_POINT('Ctrl Pts',(0.130895502574684,-0.594652107438951,
-0.12));
#40128=CARTESIAN_POINT('Ctrl Pts',(0.16128528154991,-0.585821879212206,
-0.12));
#40129=CARTESIAN_POINT('Ctrl Pts',(0.190892183977264,-0.574664264569325,
-0.12));
#40130=CARTESIAN_POINT('Ctrl Pts',(0.21942623032083,-0.561211828032157,
-0.12));
#40131=CARTESIAN_POINT('Ctrl Pts',(0.241737226557842,-0.550693261637977,
-0.12));
#40132=CARTESIAN_POINT('Ctrl Pts',(0.263392112795318,-0.53877018802294,
-0.12));
#40133=CARTESIAN_POINT('Ctrl Pts',(0.284272054715151,-0.525522446725764,
-0.12));
#40134=CARTESIAN_POINT('Ctrl Pts',(0.29057737878399,-0.521521894311416,
-0.12));
#40135=CARTESIAN_POINT('Ctrl Pts',(0.296813196360162,-0.517399549803865,
-0.12));
#40136=CARTESIAN_POINT('Ctrl Pts',(0.302971897916213,-0.513160117534818,
-0.12));
#40137=CARTESIAN_POINT('Ctrl Pts',(0.327487947260565,-0.496284136493344,
-0.12));
#40138=CARTESIAN_POINT('Ctrl Pts',(0.350669698473764,-0.477636222421621,
-0.12));
#40139=CARTESIAN_POINT('Ctrl Pts',(0.372326859018955,-0.457378924688331,
-0.12));
#40140=CARTESIAN_POINT('Ctrl Pts',(0.393597599384017,-0.43748306993473,
-0.12));
#40141=CARTESIAN_POINT('Ctrl Pts',(0.413398440600423,-0.416033780451133,
-0.12));
#40142=CARTESIAN_POINT('Ctrl Pts',(0.431509449154427,-0.393155467378397,
-0.12));
#40143=CARTESIAN_POINT('Ctrl Pts',(0.43634572983353,-0.387046147560331,
-0.12));
#40144=CARTESIAN_POINT('Ctrl Pts',(0.441061254550602,-0.380834805043548,
-0.12));
#40145=CARTESIAN_POINT('Ctrl Pts',(0.44565123783516,-0.374523575106285,
-0.12));
#40146=CARTESIAN_POINT('',(-0.353390396098499,0.46258854508056,-0.72625));
#40147=CARTESIAN_POINT('Ctrl Pts',(-0.353420490498553,0.462617301267147,
-0.72625));
#40148=CARTESIAN_POINT('Ctrl Pts',(-0.331343914475331,0.482052117168188,
-0.72625));
#40149=CARTESIAN_POINT('Ctrl Pts',(-0.307843201132015,0.499732456588995,
-0.72625));
#40150=CARTESIAN_POINT('Ctrl Pts',(-0.283172855491956,0.515579930268511,
-0.72625));
#40151=CARTESIAN_POINT('Ctrl Pts',(-0.257338168972133,0.53217534083206,
-0.72625));
#40152=CARTESIAN_POINT('Ctrl Pts',(-0.230219925034403,0.546761932985982,
-0.72625));
#40153=CARTESIAN_POINT('Ctrl Pts',(-0.202067218313667,0.559208190060778,
-0.72625));
#40154=CARTESIAN_POINT('Ctrl Pts',(-0.195896923741982,0.561936065331465,
-0.72625));
#40155=CARTESIAN_POINT('Ctrl Pts',(-0.189676811570407,0.564560935846749,
-0.72625));
#40156=CARTESIAN_POINT('Ctrl Pts',(-0.183409317371435,0.567081079046547,
-0.72625));
#40157=CARTESIAN_POINT('Ctrl Pts',(-0.176798752551787,0.569739170055198,
-0.72625));
#40158=CARTESIAN_POINT('Ctrl Pts',(-0.17014384257185,0.572277351670826,
-0.72625));
#40159=CARTESIAN_POINT('Ctrl Pts',(-0.163450714977005,0.574693394083012,
-0.72625));
#40160=CARTESIAN_POINT('Ctrl Pts',(-0.147536270437225,0.580438088537081,
-0.72625));
#40161=CARTESIAN_POINT('Ctrl Pts',(-0.131400896704278,0.585494582417171,
-0.72625));
#40162=CARTESIAN_POINT('Ctrl Pts',(-0.115087389998091,0.589845129045876,
-0.72625));
#40163=CARTESIAN_POINT('Ctrl Pts',(-0.0904845801913842,0.59640629784845,
-0.72625));
#40164=CARTESIAN_POINT('Ctrl Pts',(-0.065476953188039,0.601363175763682,
-0.72625));
#40165=CARTESIAN_POINT('Ctrl Pts',(-0.040220969016932,0.604734997002558,
-0.72625));
#40166=CARTESIAN_POINT('Ctrl Pts',(-0.0232728051723021,0.60699767575719,
-0.72625));
#40167=CARTESIAN_POINT('Ctrl Pts',(-0.00621251576441358,0.608546060010427,
-0.72625));
#40168=CARTESIAN_POINT('Ctrl Pts',(0.0109143171267901,0.609379421018909,
-0.72625));
#40169=CARTESIAN_POINT('Ctrl Pts',(0.0179713338528023,0.60972280281127,
-0.72625));
#40170=CARTESIAN_POINT('Ctrl Pts',(0.0250400715171394,0.609944566997145,
-0.72625));
#40171=CARTESIAN_POINT('Ctrl Pts',(0.0321018300265921,0.610044668541972,
-0.72625));
#40172=CARTESIAN_POINT('Ctrl Pts',(0.0629203426176338,0.610481525836862,
-0.72625));
#40173=CARTESIAN_POINT('Ctrl Pts',(0.0936755695308824,0.608609614963221,
-0.72625));
#40174=CARTESIAN_POINT('Ctrl Pts',(0.124099989476803,0.60446798569458,-0.72625));
#40175=CARTESIAN_POINT('Ctrl Pts',(0.14542332482861,0.601565273006711,-0.72625));
#40176=CARTESIAN_POINT('Ctrl Pts',(0.166584716115012,0.597546610890188,
-0.72625));
#40177=CARTESIAN_POINT('Ctrl Pts',(0.187494048945749,0.592410339560903,
-0.72625));
#40178=CARTESIAN_POINT('Ctrl Pts',(0.202188505813513,0.588800720922169,
-0.72625));
#40179=CARTESIAN_POINT('Ctrl Pts',(0.216758501690732,0.584638862439533,
-0.72625));
#40180=CARTESIAN_POINT('Ctrl Pts',(0.231178697027477,0.579939611265494,
-0.72625));
#40181=CARTESIAN_POINT('Ctrl Pts',(0.238102595557612,0.577683252212315,
-0.72625));
#40182=CARTESIAN_POINT('Ctrl Pts',(0.244991946660547,0.575302954377583,
-0.72625));
#40183=CARTESIAN_POINT('Ctrl Pts',(0.251843864110581,0.572800121359829,
-0.72625));
#40184=CARTESIAN_POINT('Ctrl Pts',(0.258582145288071,0.570338796812808,
-0.72625));
#40185=CARTESIAN_POINT('Ctrl Pts',(0.265277205063595,0.567761447216236,
-0.72625));
#40186=CARTESIAN_POINT('Ctrl Pts',(0.271920132877671,0.565072819537037,
-0.72625));
#40187=CARTESIAN_POINT('Ctrl Pts',(0.30080227087538,0.553383197456466,-0.72625));
#40188=CARTESIAN_POINT('Ctrl Pts',(0.328737399818583,0.539580421272658,
-0.72625));
#40189=CARTESIAN_POINT('Ctrl Pts',(0.355518167806567,0.523830055574735,
-0.72625));
#40190=CARTESIAN_POINT('Ctrl Pts',(0.382426618369393,0.508004596912789,
-0.72625));
#40191=CARTESIAN_POINT('Ctrl Pts',(0.408170864031784,0.490212434749928,
-0.72625));
#40192=CARTESIAN_POINT('Ctrl Pts',(0.432524619771516,0.470572470283676,
-0.72625));
#40193=CARTESIAN_POINT('Ctrl Pts',(0.442905486761684,0.462200872038434,
-0.72625));
#40194=CARTESIAN_POINT('Ctrl Pts',(0.45303341106848,0.453492981462904,-0.72625));
#40195=CARTESIAN_POINT('Ctrl Pts',(0.46288916039365,0.444455658495751,-0.72625));
#40196=CARTESIAN_POINT('Ctrl Pts',(-0.353420490498551,0.462617301267149,
-0.72625));
#40197=CARTESIAN_POINT('Ctrl Pts',(-0.359516126172293,0.457966781316138,
-0.725969700760581));
#40198=CARTESIAN_POINT('Ctrl Pts',(-0.441333858628395,0.392916952001327,
-0.722148997414251));
#40199=CARTESIAN_POINT('Ctrl Pts',(-0.5636424333859,0.224934817531868,-0.714787889961011));
#40200=CARTESIAN_POINT('Ctrl Pts',(-0.602534986633661,-0.0723403849529277,
-0.704166677640278));
#40201=CARTESIAN_POINT('Ctrl Pts',(-0.494377117526733,-0.351960929022743,
-0.693545465319546));
#40202=CARTESIAN_POINT('Ctrl Pts',(-0.265553394359715,-0.545678585605523,
-0.682924252998813));
#40203=CARTESIAN_POINT('Ctrl Pts',(0.0280810564139534,-0.606214132210099,
-0.672303040678082));
#40204=CARTESIAN_POINT('Ctrl Pts',(0.314862960821169,-0.518792316784799,
-0.661681828357348));
#40205=CARTESIAN_POINT('Ctrl Pts',(0.524796465182481,-0.30475021433233,
-0.651060616036617));
#40206=CARTESIAN_POINT('Ctrl Pts',(0.60664446863493,-0.0163284320554081,
-0.640439403715884));
#40207=CARTESIAN_POINT('Ctrl Pts',(0.540430098503603,0.27607856963071,-0.629818191395151));
#40208=CARTESIAN_POINT('Ctrl Pts',(0.342314351095128,0.501103761813076,
-0.619196979074419));
#40209=CARTESIAN_POINT('Ctrl Pts',(0.0606507420151454,0.603825781241362,
-0.608575766753688));
#40210=CARTESIAN_POINT('Ctrl Pts',(-0.235815726583716,0.55917352432788,
-0.597954554432955));
#40211=CARTESIAN_POINT('Ctrl Pts',(-0.474727237871055,0.378045153975223,
-0.587333342112222));
#40212=CARTESIAN_POINT('Ctrl Pts',(-0.597773230616621,0.104648229800698,
-0.576712129791491));
#40213=CARTESIAN_POINT('Ctrl Pts',(-0.574922177901191,-0.194289931772878,
-0.566090917470757));
#40214=CARTESIAN_POINT('Ctrl Pts',(-0.41175127661568,-0.445808225543571,
-0.555469705150026));
#40215=CARTESIAN_POINT('Ctrl Pts',(-0.148085250655247,-0.588519198041721,
-0.544848492829293));
#40216=CARTESIAN_POINT('Ctrl Pts',(0.151723579920602,-0.587591731726026,
-0.53422728050856));
#40217=CARTESIAN_POINT('Ctrl Pts',(0.414501607921562,-0.443252191094065,
-0.523606068187829));
#40218=CARTESIAN_POINT('Ctrl Pts',(0.576113244100042,-0.190729174156685,
-0.512984855867096));
#40219=CARTESIAN_POINT('Ctrl Pts',(0.597114332253383,0.108344645017158,
-0.502363643546364));
#40220=CARTESIAN_POINT('Ctrl Pts',(0.472379188307862,0.38097505213334,-0.491742431225632));
#40221=CARTESIAN_POINT('Ctrl Pts',(0.232351613210618,0.560621811678453,
-0.481121218904899));
#40222=CARTESIAN_POINT('Ctrl Pts',(-0.0643854508469475,0.603438979194421,
-0.470500006584167));
#40223=CARTESIAN_POINT('Ctrl Pts',(-0.345408115665845,0.498976273508361,
-0.459878794263435));
#40224=CARTESIAN_POINT('Ctrl Pts',(-0.542127867956924,0.272729651259685,
-0.449257581942702));
#40225=CARTESIAN_POINT('Ctrl Pts',(-0.606531799752129,-0.0200814287731599,
-0.43863636962197));
#40226=CARTESIAN_POINT('Ctrl Pts',(-0.522901001209041,-0.307991283685645,
-0.428015157301237));
#40227=CARTESIAN_POINT('Ctrl Pts',(-0.311647036430625,-0.52073046058026,
-0.417393944980506));
#40228=CARTESIAN_POINT('Ctrl Pts',(-0.0243301430172896,-0.606376229772182,
-0.406772732659772));
#40229=CARTESIAN_POINT('Ctrl Pts',(0.268924948789863,-0.54402523821012,
-0.396151520339041));
#40230=CARTESIAN_POINT('Ctrl Pts',(0.49654418722808,-0.348895339642708,
-0.385530308018308));
#40231=CARTESIAN_POINT('Ctrl Pts',(0.602973102433286,-0.0686114103358565,
-0.374909095697576));
#40232=CARTESIAN_POINT('Ctrl Pts',(0.562235849856194,0.22841833778935,-0.364287883376844));
#40233=CARTESIAN_POINT('Ctrl Pts',(0.384275070866584,0.469698581847689,
-0.353666671056111));
#40234=CARTESIAN_POINT('Ctrl Pts',(0.112525216897816,0.596340643809236,
-0.343045458735379));
#40235=CARTESIAN_POINT('Ctrl Pts',(-0.186688391221607,0.577435305907412,
-0.332424246414646));
#40236=CARTESIAN_POINT('Ctrl Pts',(-0.440337420784613,0.417596747609107,
-0.321803034093914));
#40237=CARTESIAN_POINT('Ctrl Pts',(-0.58651437550708,0.155836374298491,
-0.311181821773182));
#40238=CARTESIAN_POINT('Ctrl Pts',(-0.589542202382296,-0.14395860117576,
-0.30056060945245));
#40239=CARTESIAN_POINT('Ctrl Pts',(-0.44868191070889,-0.408617953378765,
-0.289939397131717));
#40240=CARTESIAN_POINT('Ctrl Pts',(-0.198312919647183,-0.573546923201999,
-0.279318184810985));
#40241=CARTESIAN_POINT('Ctrl Pts',(0.100457810451271,-0.598491699957539,
-0.268696972490252));
#40242=CARTESIAN_POINT('Ctrl Pts',(0.374710067503894,-0.477364075292773,
-0.25807576016952));
#40243=CARTESIAN_POINT('Ctrl Pts',(0.557507719479534,-0.239727367437853,
-0.247454547848788));
#40244=CARTESIAN_POINT('Ctrl Pts',(0.604235901607852,0.0564190059013063,
-0.236833335528056));
#40245=CARTESIAN_POINT('Ctrl Pts',(0.503489562133039,0.338795342097125,
-0.226212123207323));
#40246=CARTESIAN_POINT('Ctrl Pts',(0.279858047502047,0.538482706593586,
-0.215590910886591));
#40247=CARTESIAN_POINT('Ctrl Pts',(-0.0120783079673112,0.606743961071895,
-0.204969698565858));
#40248=CARTESIAN_POINT('Ctrl Pts',(-0.301065603751776,0.526918614476648,
-0.194348486245126));
#40249=CARTESIAN_POINT('Ctrl Pts',(-0.516574810615386,0.318489709300428,
-0.183727273924394));
#40250=CARTESIAN_POINT('Ctrl Pts',(-0.606000393860149,0.0323274504734039,
-0.173106061603662));
#40251=CARTESIAN_POINT('Ctrl Pts',(-0.54752982679742,-0.261724193796561,
-0.162484849282929));
#40252=CARTESIAN_POINT('Ctrl Pts',(-0.355407358238332,-0.491898842808179,
-0.151863636962197));
#40253=CARTESIAN_POINT('Ctrl Pts',(-0.076576683950909,-0.602014117802982,
-0.141242424641464));
#40254=CARTESIAN_POINT('Ctrl Pts',(0.221016091685922,-0.565203769676402,
-0.130621212320732));
#40255=CARTESIAN_POINT('Ctrl Pts',(0.383330620179427,-0.448679815853072,
-0.123540404106911));
#40256=CARTESIAN_POINT('Ctrl Pts',(0.44565123783516,-0.374523575106285,
-0.12));
#40257=CARTESIAN_POINT('Ctrl Pts',(-0.347393831483963,0.454739033234329,
-0.742528335043099));
#40258=CARTESIAN_POINT('Ctrl Pts',(-0.421311558764174,0.398270244285598,
-0.73906984429286));
#40259=CARTESIAN_POINT('Ctrl Pts',(-0.541032820871556,0.248672210016143,
-0.732152862792381));
#40260=CARTESIAN_POINT('Ctrl Pts',(-0.594466754531496,-0.0338563072418703,
-0.721777390541663));
#40261=CARTESIAN_POINT('Ctrl Pts',(-0.509318192700196,-0.308427575223672,
-0.711401918290944));
#40262=CARTESIAN_POINT('Ctrl Pts',(-0.305432606070274,-0.511127575150115,
-0.701026446040226));
#40263=CARTESIAN_POINT('Ctrl Pts',(-0.0303432431553614,-0.594654413195259,
-0.690650973789507));
#40264=CARTESIAN_POINT('Ctrl Pts',(0.251820278225985,-0.539559427088026,
-0.680275501538789));
#40265=CARTESIAN_POINT('Ctrl Pts',(0.47527762677182,-0.358674800641695,
-0.669900029288071));
#40266=CARTESIAN_POINT('Ctrl Pts',(0.587935213613219,-0.0941755582271385,
-0.659524557037353));
#40267=CARTESIAN_POINT('Ctrl Pts',(0.563529430095987,0.192279525622204,
-0.649149084786634));
#40268=CARTESIAN_POINT('Ctrl Pts',(0.407749978910367,0.433908628992312,
-0.638773612535916));
#40269=CARTESIAN_POINT('Ctrl Pts',(0.156913157834808,0.574382355007991,
-0.628398140285198));
#40270=CARTESIAN_POINT('Ctrl Pts',(-0.130504285744414,0.580952155897969,
-0.618022668034479));
#40271=CARTESIAN_POINT('Ctrl Pts',(-0.387497714117257,0.452086632150457,
-0.607647195783761));
#40272=CARTESIAN_POINT('Ctrl Pts',(-0.554155123557569,0.217827664148314,
-0.597271723533043));
#40273=CARTESIAN_POINT('Ctrl Pts',(-0.591624244031004,-0.0672127059237326,
-0.586896251282324));
#40274=CARTESIAN_POINT('Ctrl Pts',(-0.491170026481974,-0.336584016022301,
-0.576520779031606));
#40275=CARTESIAN_POINT('Ctrl Pts',(-0.276211019809465,-0.527488640774144,
-0.566145306780888));
#40276=CARTESIAN_POINT('Ctrl Pts',(0.0031401178304551,-0.595421643954287,
-0.555769834530169));
#40277=CARTESIAN_POINT('Ctrl Pts',(0.281759210488034,-0.524546033533648,
-0.545394362279452));
#40278=CARTESIAN_POINT('Ctrl Pts',(0.494692741566129,-0.331384799915253,
-0.535018890028733));
#40279=CARTESIAN_POINT('Ctrl Pts',(0.59230024480053,-0.0609689603923613,
-0.524643417778015));
#40280=CARTESIAN_POINT('Ctrl Pts',(0.551826816631903,0.223660364318458,
-0.514267945527296));
#40281=CARTESIAN_POINT('Ctrl Pts',(0.382707889009843,0.456148512904055,
-0.503892473276577));
#40282=CARTESIAN_POINT('Ctrl Pts',(0.124369579435742,0.582296317894835,
-0.49351700102586));
#40283=CARTESIAN_POINT('Ctrl Pts',(-0.162962585060135,0.572695372777406,
-0.483141528775141));
#40284=CARTESIAN_POINT('Ctrl Pts',(-0.412303839155969,0.429583913041453,
-0.472766056524423));
#40285=CARTESIAN_POINT('Ctrl Pts',(-0.565526108608774,0.186325024110395,
-0.462390584273704));
#40286=CARTESIAN_POINT('Ctrl Pts',(-0.586909209500827,-0.100371180778523,
-0.452015112022986));
#40287=CARTESIAN_POINT('Ctrl Pts',(-0.471468172615134,-0.363668195390408,
-0.441639639772268));
#40288=CARTESIAN_POINT('Ctrl Pts',(-0.24611537226857,-0.542184486739477,
-0.431264167521549));
#40289=CARTESIAN_POINT('Ctrl Pts',(0.0366134635183988,-0.594303162045059,
-0.420888695270832));
#40290=CARTESIAN_POINT('Ctrl Pts',(0.310806727710773,-0.507873972691536,
-0.410513223020113));
#40291=CARTESIAN_POINT('Ctrl Pts',(0.51254268190422,-0.30304586015049,-0.400137750769395));
#40292=CARTESIAN_POINT('Ctrl Pts',(0.594791312689474,-0.0275697021364228,
-0.389762278518676));
#40293=CARTESIAN_POINT('Ctrl Pts',(0.53837827792754,0.254333686297961,-0.379386806267958));
#40294=CARTESIAN_POINT('Ctrl Pts',(0.356454955565181,0.476945131829576,
-0.36901133401724));
#40295=CARTESIAN_POINT('Ctrl Pts',(0.0914325078965691,0.588367989131544,
-0.358635861766521));
#40296=CARTESIAN_POINT('Ctrl Pts',(-0.1949052878214,0.562626628325057,-0.348260389515803));
#40297=CARTESIAN_POINT('Ctrl Pts',(-0.435805479980445,0.405722044928676,
-0.337884917265085));
#40298=CARTESIAN_POINT('Ctrl Pts',(-0.575107830414381,0.154232867992362,
-0.327509445014366));
#40299=CARTESIAN_POINT('Ctrl Pts',(-0.580337258022503,-0.133212090073103,
-0.317133972763648));
#40300=CARTESIAN_POINT('Ctrl Pts',(-0.450274644860222,-0.389601769278859,
-0.30675850051293));
#40301=CARTESIAN_POINT('Ctrl Pts',(-0.215241042075345,-0.555164919115264,
-0.296383028262211));
#40302=CARTESIAN_POINT('Ctrl Pts',(0.0699709674208999,-0.591304370416951,
-0.286007556011493));
#40303=CARTESIAN_POINT('Ctrl Pts',(0.338870887774159,-0.489595052448449,
-0.275632083760774));
#40304=CARTESIAN_POINT('Ctrl Pts',(0.528770989858389,-0.273748118747132,
-0.265256611510057));
#40305=CARTESIAN_POINT('Ctrl Pts',(0.595400531599021,0.00591678855841044,
-0.254881139259338));
#40306=CARTESIAN_POINT('Ctrl Pts',(0.523226356835316,0.284202314475096,
-0.24450566700862));
#40307=CARTESIAN_POINT('Ctrl Pts',(0.329074261287382,0.496232767362635,
-0.234130194757902));
#40308=CARTESIAN_POINT('Ctrl Pts',(0.0582061064454895,0.592578090033583,
-0.223754722507183));
#40309=CARTESIAN_POINT('Ctrl Pts',(-0.226231237425986,0.550777869717469,
-0.213379250256465));
#40310=CARTESIAN_POINT('Ctrl Pts',(-0.457928466129024,0.380576366952199,
-0.203003778005746));
#40311=CARTESIAN_POINT('Ctrl Pts',(-0.582869603662733,0.121653032232085,
-0.192628305755028));
#40312=CARTESIAN_POINT('Ctrl Pts',(-0.57192991628486,-0.165632118696112,
-0.18225283350431));
#40313=CARTESIAN_POINT('Ctrl Pts',(-0.427655041590171,-0.414301519355521,
-0.171877361253592));
#40314=CARTESIAN_POINT('Ctrl Pts',(-0.183688600698895,-0.566391183638125,
-0.161501889002873));
#40315=CARTESIAN_POINT('Ctrl Pts',(0.103112831945545,-0.586430161623632,
-0.151126416752155));
#40316=CARTESIAN_POINT('Ctrl Pts',(0.365851355459577,-0.469776284513869,
-0.140750944501437));
#40317=CARTESIAN_POINT('Ctrl Pts',(0.543351022386391,-0.243565284402786,
-0.130375472250718));
#40318=CARTESIAN_POINT('Ctrl Pts',(0.577149518655877,-0.0549640805153465,
-0.123458490750239));
#40319=CARTESIAN_POINT('Ctrl Pts',(0.570996795169322,0.0378513197440182,
-0.12));
#40320=CARTESIAN_POINT('Ctrl Pts',(-0.347393831483963,0.454739033234329,
-0.739668503816594));
#40321=CARTESIAN_POINT('Ctrl Pts',(-0.421311232212742,0.398270493751654,
-0.736210013066354));
#40322=CARTESIAN_POINT('Ctrl Pts',(-0.541032978501356,0.24867202957397,
-0.729293031565875));
#40323=CARTESIAN_POINT('Ctrl Pts',(-0.594466633440188,-0.0338562272977153,
-0.718917559315157));
#40324=CARTESIAN_POINT('Ctrl Pts',(-0.509318208145951,-0.30842759690902,
-0.708542087064439));
#40325=CARTESIAN_POINT('Ctrl Pts',(-0.305432567022533,-0.511127527137462,
-0.698166614813721));
#40326=CARTESIAN_POINT('Ctrl Pts',(-0.0303432525733253,-0.594654389935448,
-0.687791142563002));
#40327=CARTESIAN_POINT('Ctrl Pts',(0.251820269803062,-0.53955939207586,
-0.677415670312284));
#40328=CARTESIAN_POINT('Ctrl Pts',(0.475277597483338,-0.358674783173242,
-0.667040198061565));
#40329=CARTESIAN_POINT('Ctrl Pts',(0.587935182297583,-0.0941755517205918,
-0.656664725810847));
#40330=CARTESIAN_POINT('Ctrl Pts',(0.563529397998721,0.192279514278788,
-0.64628925356013));
#40331=CARTESIAN_POINT('Ctrl Pts',(0.407749956566778,0.433908605151244,
-0.635913781309409));
#40332=CARTESIAN_POINT('Ctrl Pts',(0.156913148914841,0.574382322862107,
-0.625538309058693));
#40333=CARTESIAN_POINT('Ctrl Pts',(-0.130504278385431,0.580952123629563,
-0.615162836807973));
#40334=CARTESIAN_POINT('Ctrl Pts',(-0.387497692586036,0.452086606935182,
-0.604787364557256));
#40335=CARTESIAN_POINT('Ctrl Pts',(-0.554155092676422,0.217827652039444,
-0.594411892306537));
#40336=CARTESIAN_POINT('Ctrl Pts',(-0.591624211098557,-0.0672127021914847,
-0.584036420055819));
#40337=CARTESIAN_POINT('Ctrl Pts',(-0.491169999125539,-0.336583997274562,
-0.5736609478051));
#40338=CARTESIAN_POINT('Ctrl Pts',(-0.276211004431821,-0.527488611403925,
-0.563285475554383));
#40339=CARTESIAN_POINT('Ctrl Pts',(0.00314011765710889,-0.595421610797266,
-0.552910003303663));
#40340=CARTESIAN_POINT('Ctrl Pts',(0.281759194797687,-0.524546004325305,
-0.542534531052945));
#40341=CARTESIAN_POINT('Ctrl Pts',(0.494692714019857,-0.331384781461957,
-0.532159058802227));
#40342=CARTESIAN_POINT('Ctrl Pts',(0.592300211818467,-0.060968956997514,
-0.521783586551509));
#40343=CARTESIAN_POINT('Ctrl Pts',(0.551826785903869,0.223660351864156,
-0.51140811430079));
#40344=CARTESIAN_POINT('Ctrl Pts',(0.382707867698945,0.456148487503667,
-0.501032642050072));
#40345=CARTESIAN_POINT('Ctrl Pts',(0.124369572510325,0.58229628547005,-0.490657169799354));
#40346=CARTESIAN_POINT('Ctrl Pts',(-0.162962575985677,0.572695340887211,
-0.480281697548635));
#40347=CARTESIAN_POINT('Ctrl Pts',(-0.412303816197081,0.429583889120347,
-0.469906225297917));
#40348=CARTESIAN_POINT('Ctrl Pts',(-0.565526077117809,0.186325013734999,
-0.459530753047199));
#40349=CARTESIAN_POINT('Ctrl Pts',(-0.586909176819153,-0.100371175189415,
-0.44915528079648));
#40350=CARTESIAN_POINT('Ctrl Pts',(-0.471468146361724,-0.363668175139773,
-0.438779808545763));
#40351=CARTESIAN_POINT('Ctrl Pts',(-0.246115358563789,-0.542184456548272,
-0.428404336295043));
#40352=CARTESIAN_POINT('Ctrl Pts',(0.0366134614796009,-0.59430312895166,
-0.418028864044326));
#40353=CARTESIAN_POINT('Ctrl Pts',(0.310806710403695,-0.507873944410889,
-0.407653391793607));
#40354=CARTESIAN_POINT('Ctrl Pts',(0.5125426533636,-0.303045843275575,-0.397277919542889));
#40355=CARTESIAN_POINT('Ctrl Pts',(0.594791279568892,-0.0275697006012128,
-0.386902447292171));
#40356=CARTESIAN_POINT('Ctrl Pts',(0.538378247948281,0.254333672135533,
-0.376526975041452));
#40357=CARTESIAN_POINT('Ctrl Pts',(0.356454935716209,0.476945105271217,
-0.366151502790734));
#40358=CARTESIAN_POINT('Ctrl Pts',(0.0914325028052065,0.588367956368575,
-0.355776030540016));
#40359=CARTESIAN_POINT('Ctrl Pts',(-0.19490527696822,0.562626596995675,
-0.345400558289297));
#40360=CARTESIAN_POINT('Ctrl Pts',(-0.435805455712891,0.405722022336039,
-0.335025086038579));
#40361=CARTESIAN_POINT('Ctrl Pts',(-0.575107798389857,0.154232859404514,
-0.324649613787861));
#40362=CARTESIAN_POINT('Ctrl Pts',(-0.580337225706793,-0.133212082656289,
-0.314274141537142));
#40363=CARTESIAN_POINT('Ctrl Pts',(-0.450274619786945,-0.389601747582111,
-0.303898669286424));
#40364=CARTESIAN_POINT('Ctrl Pts',(-0.215241030089811,-0.555164888205254,
-0.293523197035706));
#40365=CARTESIAN_POINT('Ctrl Pts',(0.069970963524667,-0.591304337482598,
-0.283147724784988));
#40366=CARTESIAN_POINT('Ctrl Pts',(0.338870868904234,-0.489595025201401,
-0.272772252534269));
#40367=CARTESIAN_POINT('Ctrl Pts',(0.528770960414329,-0.273748103472406,
-0.262396780283551));
#40368=CARTESIAN_POINT('Ctrl Pts',(0.595400498444076,0.00591678816698449,
-0.252021308032832));
#40369=CARTESIAN_POINT('Ctrl Pts',(0.523226327700652,0.284202298772356,
-0.241645835782114));
#40370=CARTESIAN_POINT('Ctrl Pts',(0.329074242961365,0.496232739486468,
-0.231270363531395));
#40371=CARTESIAN_POINT('Ctrl Pts',(0.0582061032077348,0.592578057519749,
-0.220894891280678));
#40372=CARTESIAN_POINT('Ctrl Pts',(-0.226231224835217,0.550777838088684,
-0.210519419029959));
#40373=CARTESIAN_POINT('Ctrl Pts',(-0.457928440616124,0.380576347662404,
-0.200143946779241));
#40374=CARTESIAN_POINT('Ctrl Pts',(-0.582869571232661,0.121653021684456,
-0.189768474528522));
#40375=CARTESIAN_POINT('Ctrl Pts',(-0.571929884384423,-0.165632101988046,
-0.179393002277804));
#40376=CARTESIAN_POINT('Ctrl Pts',(-0.427655017881361,-0.414301511133043,
-0.169017530027086));
#40377=CARTESIAN_POINT('Ctrl Pts',(-0.18368859026215,-0.566391122638,-0.158642057776367));
#40378=CARTESIAN_POINT('Ctrl Pts',(0.103112825789684,-0.586430187525968,
-0.148266585525649));
#40379=CARTESIAN_POINT('Ctrl Pts',(0.365851335923764,-0.469776140734439,
-0.137891113274931));
#40380=CARTESIAN_POINT('Ctrl Pts',(0.543350990324924,-0.243565521844555,
-0.127515641024213));
#40381=CARTESIAN_POINT('Ctrl Pts',(0.577149491474567,-0.0549636704783635,
-0.120598659523734));
#40382=CARTESIAN_POINT('Ctrl Pts',(0.570996795169322,0.0378513197440182,
-0.117140168773494));
#40383=CARTESIAN_POINT('Ctrl Pts',(-0.348354931983335,0.455997115192948,
-0.732991220638421));
#40384=CARTESIAN_POINT('Ctrl Pts',(-0.422477789664249,0.399371618702867,
-0.729532729888182));
#40385=CARTESIAN_POINT('Ctrl Pts',(-0.542529339555234,0.249360534892675,
-0.722615748387703));
#40386=CARTESIAN_POINT('Ctrl Pts',(-0.596111640911723,-0.0339501282728968,
-0.712240276136984));
#40387=CARTESIAN_POINT('Ctrl Pts',(-0.510727243702018,-0.309280829796352,
-0.701864803886266));
#40388=CARTESIAN_POINT('Ctrl Pts',(-0.306277691824433,-0.512541754315929,
-0.691489331635547));
#40389=CARTESIAN_POINT('Ctrl Pts',(-0.0304271726811044,-0.596299630171875,
-0.68111385938483));
#40390=CARTESIAN_POINT('Ctrl Pts',(0.25251698096947,-0.541052240814961,
-0.67073838713411));
#40391=CARTESIAN_POINT('Ctrl Pts',(0.476592587302813,-0.359667144766162,
-0.660362914883394));
#40392=CARTESIAN_POINT('Ctrl Pts',(0.589561856766694,-0.0944361170651719,
-0.649987442632673));
#40393=CARTESIAN_POINT('Ctrl Pts',(0.565088553664507,0.192811508424799,
-0.639611970381957));
#40394=CARTESIAN_POINT('Ctrl Pts',(0.408878103922812,0.435109127467229,
-0.629236498131237));
#40395=CARTESIAN_POINT('Ctrl Pts',(0.157347291299003,0.575971504394943,
-0.61886102588052));
#40396=CARTESIAN_POINT('Ctrl Pts',(-0.130865353358995,0.582559481545958,
-0.608485553629801));
#40397=CARTESIAN_POINT('Ctrl Pts',(-0.388569807605722,0.453337424575784,
-0.598110081379083));
#40398=CARTESIAN_POINT('Ctrl Pts',(-0.555688309805857,0.218430329959781,
-0.587734609128365));
#40399=CARTESIAN_POINT('Ctrl Pts',(-0.593261096380303,-0.0673986639305479,
-0.577359136877646));
#40400=CARTESIAN_POINT('Ctrl Pts',(-0.492528951234956,-0.337515246201882,
-0.566983664626928));
#40401=CARTESIAN_POINT('Ctrl Pts',(-0.276975215435484,-0.528948048563023,
-0.55660819237621));
#40402=CARTESIAN_POINT('Ctrl Pts',(0.00314880562114232,-0.597069002631033,
-0.546232720125491));
#40403=CARTESIAN_POINT('Ctrl Pts',(0.282538756352733,-0.525997299987159,
-0.535857247874774));
#40404=CARTESIAN_POINT('Ctrl Pts',(0.496061412635949,-0.33230164536513,
-0.525481775624054));
#40405=CARTESIAN_POINT('Ctrl Pts',(0.59393896747061,-0.0611376437893791,
-0.515106303373337));
#40406=CARTESIAN_POINT('Ctrl Pts',(0.553353561086247,0.224279167556245,
-0.504730831122618));
#40407=CARTESIAN_POINT('Ctrl Pts',(0.383766730533475,0.457410543293981,
-0.4943553588719));
#40408=CARTESIAN_POINT('Ctrl Pts',(0.1247136739233,0.583907362605643,-0.483979886621181));
#40409=CARTESIAN_POINT('Ctrl Pts',(-0.163413455180115,0.574279854462932,
-0.473604414370463));
#40410=CARTESIAN_POINT('Ctrl Pts',(-0.413444564073729,0.430772446902474,
-0.463228942119745));
#40411=CARTESIAN_POINT('Ctrl Pts',(-0.567090755023527,0.186840531310716,
-0.452853469869027));
#40412=CARTESIAN_POINT('Ctrl Pts',(-0.588533016742363,-0.100648878670382,
-0.442477997618308));
#40413=CARTESIAN_POINT('Ctrl Pts',(-0.472772588051884,-0.364674359614158,
-0.43210252536759));
#40414=CARTESIAN_POINT('Ctrl Pts',(-0.246796301988659,-0.543684553669019,
-0.421727053116871));
#40415=CARTESIAN_POINT('Ctrl Pts',(0.0367147623329972,-0.595947426204782,
-0.411351580866153));
#40416=CARTESIAN_POINT('Ctrl Pts',(0.311666639613677,-0.509279112398487,
-0.400976108615435));
#40417=CARTESIAN_POINT('Ctrl Pts',(0.513960738572949,-0.303884299987962,
-0.390600636364716));
#40418=CARTESIAN_POINT('Ctrl Pts',(0.596436927420187,-0.0276459794911836,
-0.380225164113998));
#40419=CARTESIAN_POINT('Ctrl Pts',(0.539867814183286,0.255037353704964,
-0.36984969186328));
#40420=CARTESIAN_POINT('Ctrl Pts',(0.357441162850323,0.478264700420943,
-0.359474219612561));
#40421=CARTESIAN_POINT('Ctrl Pts',(0.0916854750779169,0.589995832392556,
-0.349098747361843));
#40422=CARTESIAN_POINT('Ctrl Pts',(-0.195444534118195,0.564183252720138,
-0.338723275111125));
#40423=CARTESIAN_POINT('Ctrl Pts',(-0.437011227109361,0.4068445599348,-0.328347802860406));
#40424=CARTESIAN_POINT('Ctrl Pts',(-0.576698986669175,0.15465958552089,
-0.317972330609689));
#40425=CARTESIAN_POINT('Ctrl Pts',(-0.581942882583927,-0.13358064921627,
-0.30759685835897));
#40426=CARTESIAN_POINT('Ctrl Pts',(-0.451520423964013,-0.3906796841698,
-0.297221386108251));
#40427=CARTESIAN_POINT('Ctrl Pts',(-0.215836551495043,-0.556700899121684,
-0.286845913857534));
#40428=CARTESIAN_POINT('Ctrl Pts',(0.0701645567558304,-0.592940337806916,
-0.276470441606815));
#40429=CARTESIAN_POINT('Ctrl Pts',(0.339808445053429,-0.49094961966413,
-0.266094969356097));
#40430=CARTESIAN_POINT('Ctrl Pts',(0.530233945539261,-0.274505500307545,
-0.255719497105378));
#40431=CARTESIAN_POINT('Ctrl Pts',(0.597047831862276,0.00593315871250194,
-0.24534402485466));
#40432=CARTESIAN_POINT('Ctrl Pts',(0.524673972126497,0.284988619460275,
-0.234968552603942));
#40433=CARTESIAN_POINT('Ctrl Pts',(0.329984714150923,0.497605699706947,
-0.224593080353223));
#40434=CARTESIAN_POINT('Ctrl Pts',(0.0583671458221994,0.594217580488307,
-0.214217608102505));
#40435=CARTESIAN_POINT('Ctrl Pts',(-0.226857153509737,0.552301713889382,
-0.203842135851787));
#40436=CARTESIAN_POINT('Ctrl Pts',(-0.459195421158135,0.381629307506569,
-0.193466663601068));
#40437=CARTESIAN_POINT('Ctrl Pts',(-0.584482234437336,0.12198961809667,
-0.18309119135035));
#40438=CARTESIAN_POINT('Ctrl Pts',(-0.5735122802766,-0.166090389068003,
-0.172715719099632));
#40439=CARTESIAN_POINT('Ctrl Pts',(-0.428838238622185,-0.415447742653517,
-0.162340246848914));
#40440=CARTESIAN_POINT('Ctrl Pts',(-0.184196814082961,-0.567958280253259,
-0.151964774598195));
#40441=CARTESIAN_POINT('Ctrl Pts',(0.103398115987721,-0.588052530603492,
-0.141589302347477));
#40442=CARTESIAN_POINT('Ctrl Pts',(0.366863558240637,-0.471076245713187,
-0.131213830096758));
#40443=CARTESIAN_POINT('Ctrl Pts',(0.544854320261013,-0.244238674933168,
-0.12083835784604));
#40444=CARTESIAN_POINT('Ctrl Pts',(0.57874631411382,-0.0551169346444906,
-0.113921376345561));
#40445=CARTESIAN_POINT('Ctrl Pts',(0.572576516094799,0.037956039284237,
-0.110462885595322));
#40446=CARTESIAN_POINT('Ctrl Pts',(-0.351337134117122,0.45990082214547,
-0.728010697470567));
#40447=CARTESIAN_POINT('Ctrl Pts',(-0.426092626832245,0.402792029759496,
-0.724552206720328));
#40448=CARTESIAN_POINT('Ctrl Pts',(-0.547174758248607,0.251494205008789,
-0.717635225219848));
#40449=CARTESIAN_POINT('Ctrl Pts',(-0.601214131526913,-0.0342402997241306,
-0.707259752969131));
#40450=CARTESIAN_POINT('Ctrl Pts',(-0.515099575835888,-0.31192865307436,
-0.696884280718412));
#40451=CARTESIAN_POINT('Ctrl Pts',(-0.308899449256672,-0.516929247603259,
-0.686508808467694));
#40452=CARTESIAN_POINT('Ctrl Pts',(-0.0306877093666915,-0.601404304453816,
-0.676133336216976));
#40453=CARTESIAN_POINT('Ctrl Pts',(0.254678682685534,-0.545683883423435,
-0.665757863966257));
#40454=CARTESIAN_POINT('Ctrl Pts',(0.480672436342572,-0.362746086111476,
-0.655382391715539));
#40455=CARTESIAN_POINT('Ctrl Pts',(0.594608802924677,-0.0952445289974541,
-0.64500691946482));
#40456=CARTESIAN_POINT('Ctrl Pts',(0.569925983813122,0.194462065489843,
-0.634631447214103));
#40457=CARTESIAN_POINT('Ctrl Pts',(0.412378302566623,0.438833876260333,
-0.624255974963383));
#40458=CARTESIAN_POINT('Ctrl Pts',(0.158694259988426,0.580902101186212,
-0.613880502712666));
#40459=CARTESIAN_POINT('Ctrl Pts',(-0.131985624240206,0.587546476071686,
-0.603505030461946));
#40460=CARTESIAN_POINT('Ctrl Pts',(-0.391896155450462,0.457218214381192,
-0.59312955821123));
#40461=CARTESIAN_POINT('Ctrl Pts',(-0.560445273344952,0.220300200523357,
-0.58275408596051));
#40462=CARTESIAN_POINT('Ctrl Pts',(-0.598339701552755,-0.0679756295146297,
-0.572378613709792));
#40463=CARTESIAN_POINT('Ctrl Pts',(-0.496745239880617,-0.340404541731139,
-0.562003141459074));
#40464=CARTESIAN_POINT('Ctrl Pts',(-0.279346258744421,-0.533476102542041,
-0.551627669208356));
#40465=CARTESIAN_POINT('Ctrl Pts',(0.00317576094595877,-0.60218020526613,
-0.541252196957638));
#40466=CARTESIAN_POINT('Ctrl Pts',(0.284957426270576,-0.530500094103756,
-0.530876724706919));
#40467=CARTESIAN_POINT('Ctrl Pts',(0.500307940915774,-0.335146309950583,
-0.520501252456201));
#40468=CARTESIAN_POINT('Ctrl Pts',(0.599023375480799,-0.0616610119189332,
-0.510125780205482));
#40469=CARTESIAN_POINT('Ctrl Pts',(0.5580905381723,0.226199106908691,-0.499750307954764));
#40470=CARTESIAN_POINT('Ctrl Pts',(0.387051961417286,0.461326201228568,
-0.489374835704046));
#40471=CARTESIAN_POINT('Ctrl Pts',(0.125781283960076,0.588905895173768,
-0.478999363453328));
#40472=CARTESIAN_POINT('Ctrl Pts',(-0.164812354269457,0.579195970853089,
-0.468623891202609));
#40473=CARTESIAN_POINT('Ctrl Pts',(-0.416983851726037,0.434460069705598,
-0.458248418951891));
#40474=CARTESIAN_POINT('Ctrl Pts',(-0.571945329206932,0.188439977628023,
-0.447872946701173));
#40475=CARTESIAN_POINT('Ctrl Pts',(-0.593571147171812,-0.101510482291401,
-0.437497474450454));
#40476=CARTESIAN_POINT('Ctrl Pts',(-0.476819752602251,-0.367796150466586,
-0.427122002199736));
#40477=CARTESIAN_POINT('Ctrl Pts',(-0.248908999022731,-0.548338759322636,
-0.416746529949018));
#40478=CARTESIAN_POINT('Ctrl Pts',(0.037029058652927,-0.601049027605061,
-0.406371057698299));
#40479=CARTESIAN_POINT('Ctrl Pts',(0.314334658460906,-0.513638790649771,
-0.395995585447581));
#40480=CARTESIAN_POINT('Ctrl Pts',(0.518360493833721,-0.306485698202276,
-0.385620113196863));
#40481=CARTESIAN_POINT('Ctrl Pts',(0.601542719190241,-0.0278826425950967,
-0.375244640946144));
#40482=CARTESIAN_POINT('Ctrl Pts',(0.544489346680437,0.257220598171695,
-0.364869168695426));
#40483=CARTESIAN_POINT('Ctrl Pts',(0.36050103400125,0.482358880139147,-0.354493696444707));
#40484=CARTESIAN_POINT('Ctrl Pts',(0.092470347580881,0.595046485238944,
-0.34411822419399));
#40485=CARTESIAN_POINT('Ctrl Pts',(-0.197117634907101,0.569012937262736,
-0.33374275194327));
#40486=CARTESIAN_POINT('Ctrl Pts',(-0.44075225692194,0.410327348322645,
-0.323367279692553));
#40487=CARTESIAN_POINT('Ctrl Pts',(-0.581635812014072,0.155983547208043,
-0.312991807441834));
#40488=CARTESIAN_POINT('Ctrl Pts',(-0.586924598242304,-0.134724164903533,
-0.302616335191116));
#40489=CARTESIAN_POINT('Ctrl Pts',(-0.455385659596904,-0.394024093305776,
-0.292240862940398));
#40490=CARTESIAN_POINT('Ctrl Pts',(-0.217684217925031,-0.561466531081166,
-0.281865390689679));
#40491=CARTESIAN_POINT('Ctrl Pts',(0.0707651996740672,-0.598016197013366,
-0.271489918438961));
#40492=CARTESIAN_POINT('Ctrl Pts',(0.342717371516556,-0.495152388586516,
-0.261114446188242));
#40493=CARTESIAN_POINT('Ctrl Pts',(0.534773007410933,-0.276855401446306,
-0.250738973937525));
#40494=CARTESIAN_POINT('Ctrl Pts',(0.602158853270531,0.00598394908883089,
-0.240363501686806));
#40495=CARTESIAN_POINT('Ctrl Pts',(0.529165437910601,0.287428262130249,
-0.229988029436088));
#40496=CARTESIAN_POINT('Ctrl Pts',(0.332809544664039,0.501865446406052,
-0.219612557185369));
#40497=CARTESIAN_POINT('Ctrl Pts',(0.0588667971533626,0.599304376401761,
-0.209237084934651));
#40498=CARTESIAN_POINT('Ctrl Pts',(-0.228799161721906,0.557029681018242,
-0.198861612683933));
#40499=CARTESIAN_POINT('Ctrl Pts',(-0.463126358441445,0.384896252172232,
-0.188486140433214));
#40500=CARTESIAN_POINT('Ctrl Pts',(-0.589485688345832,0.12303388673101,
-0.178110668182496));
#40501=CARTESIAN_POINT('Ctrl Pts',(-0.578421825546005,-0.167512160079637,
-0.167735195931778));
#40502=CARTESIAN_POINT('Ctrl Pts',(-0.432509304272308,-0.419004265658045,
-0.157359723681059));
#40503=CARTESIAN_POINT('Ctrl Pts',(-0.18577362766596,-0.572820107924446,
-0.146984251430341));
#40504=CARTESIAN_POINT('Ctrl Pts',(0.104283251993704,-0.593086891600813,
-0.136608779179623));
#40505=CARTESIAN_POINT('Ctrl Pts',(0.370004094613953,-0.47510819824727,
-0.126233306928905));
#40506=CARTESIAN_POINT('Ctrl Pts',(0.549518529090563,-0.246330950965504,
-0.115857834678186));
#40507=CARTESIAN_POINT('Ctrl Pts',(0.583700694682622,-0.0555863733805506,
-0.108940853177707));
#40508=CARTESIAN_POINT('Ctrl Pts',(0.577478237733509,0.0382809739154165,
-0.105482362427468));
#40509=CARTESIAN_POINT('Ctrl Pts',(-0.353390396098499,0.46258854508056,
-0.72625));
#40510=CARTESIAN_POINT('Ctrl Pts',(-0.42858405975876,0.405145015906336,
-0.722791509249761));
#40511=CARTESIAN_POINT('Ctrl Pts',(-0.55037189938968,0.252964683975255,
-0.715874527749282));
#40512=CARTESIAN_POINT('Ctrl Pts',(-0.604728186893475,-0.0344407204224906,
-0.705499055498564));
#40513=CARTESIAN_POINT('Ctrl Pts',(-0.518109826791218,-0.313751520890275,
-0.695123583247845));
#40514=CARTESIAN_POINT('Ctrl Pts',(-0.310704853852748,-0.519950442031676,
-0.684748110997127));
#40515=CARTESIAN_POINT('Ctrl Pts',(-0.0308670153174011,-0.604919084841303,
-0.674372638746408));
#40516=CARTESIAN_POINT('Ctrl Pts',(0.256167092800043,-0.548873072509114,
-0.663997166495691));
#40517=CARTESIAN_POINT('Ctrl Pts',(0.483481667087119,-0.364866092549401,
-0.653621694244972));
#40518=CARTESIAN_POINT('Ctrl Pts',(0.598083901292941,-0.0958011766717911,
-0.643246221994253));
#40519=CARTESIAN_POINT('Ctrl Pts',(0.573256835517459,0.19559857304029,-0.632870749743536));
#40520=CARTESIAN_POINT('Ctrl Pts',(0.414788385679614,0.441398575257167,
-0.622495277492817));
#40521=CARTESIAN_POINT('Ctrl Pts',(0.159621726049182,0.584297099004858,
-0.612119805242099));
#40522=CARTESIAN_POINT('Ctrl Pts',(-0.132756995237261,0.59098030500446,
-0.601744332991381));
#40523=CARTESIAN_POINT('Ctrl Pts',(-0.394186534902482,0.459890359376923,
-0.591368860740661));
#40524=CARTESIAN_POINT('Ctrl Pts',(-0.563720713685333,0.221587712671107,
-0.580993388489944));
#40525=CARTESIAN_POINT('Ctrl Pts',(-0.601836610185299,-0.068372903075961,
-0.570617916239225));
#40526=CARTESIAN_POINT('Ctrl Pts',(-0.499648394643955,-0.342393986198443,
-0.560242443988507));
#40527=CARTESIAN_POINT('Ctrl Pts',(-0.280978856994308,-0.536593925414127,
-0.549866971737789));
#40528=CARTESIAN_POINT('Ctrl Pts',(0.00319432120933226,-0.605699559211484,
-0.539491499487071));
#40529=CARTESIAN_POINT('Ctrl Pts',(0.286622818181397,-0.53360052413858,
-0.529116027236352));
#40530=CARTESIAN_POINT('Ctrl Pts',(0.503231917338109,-0.337105023433553,
-0.518740554985634));
#40531=CARTESIAN_POINT('Ctrl Pts',(0.602524279792687,-0.0620213806639361,
-0.508365082734915));
#40532=CARTESIAN_POINT('Ctrl Pts',(0.561352216515463,0.227521094431647,
-0.497989610484197));
#40533=CARTESIAN_POINT('Ctrl Pts',(0.389314029870597,0.464022354589065,
-0.487614138233479));
#40534=CARTESIAN_POINT('Ctrl Pts',(0.126516394236637,0.592347669354205,
-0.477238665982761));
#40535=CARTESIAN_POINT('Ctrl Pts',(-0.165775575915184,0.582580996804279,
-0.466863193732042));
#40536=CARTESIAN_POINT('Ctrl Pts',(-0.41942085272457,0.436999207898342,
-0.456487721481324));
#40537=CARTESIAN_POINT('Ctrl Pts',(-0.575287979845788,0.189541287455112,
-0.446112249230606));
#40538=CARTESIAN_POINT('Ctrl Pts',(-0.597040186733796,-0.10210374542541,
-0.435736776979887));
#40539=CARTESIAN_POINT('Ctrl Pts',(-0.479606455752478,-0.369945681155179,
-0.425361304729169));
#40540=CARTESIAN_POINT('Ctrl Pts',(-0.250363711181598,-0.55154344482415,
-0.41498583247845));
#40541=CARTESIAN_POINT('Ctrl Pts',(0.03724546955838,-0.604561770543093,
-0.404610360227732));
#40542=CARTESIAN_POINT('Ctrl Pts',(0.316171741296042,-0.51664067727082,
-0.394234887977014));
#40543=CARTESIAN_POINT('Ctrl Pts',(0.521389975756897,-0.308276908939691,
-0.383859415726296));
#40544=CARTESIAN_POINT('Ctrl Pts',(0.605058347436381,-0.0280455986126449,
-0.373483943475577));
#40545=CARTESIAN_POINT('Ctrl Pts',(0.54767153485402,0.25872388625351,-0.363108471224859));
#40546=CARTESIAN_POINT('Ctrl Pts',(0.362607929451007,0.485177955908193,
-0.35273299897414));
#40547=CARTESIAN_POINT('Ctrl Pts',(0.0930107769727027,0.598524147198255,
-0.342357526723423));
#40548=CARTESIAN_POINT('Ctrl Pts',(-0.198269660030149,0.572338449966212,
-0.331982054472703));
#40549=CARTESIAN_POINT('Ctrl Pts',(-0.443328168880556,0.412725446363766,
-0.321606582221986));
#40550=CARTESIAN_POINT('Ctrl Pts',(-0.585035097259257,0.156895170183079,
-0.311231109971267));
#40551=CARTESIAN_POINT('Ctrl Pts',(-0.59035479302331,-0.13551154053297,
-0.300855637720549));
#40552=CARTESIAN_POINT('Ctrl Pts',(-0.458047094332503,-0.396326909369684,
-0.29048016546983));
#40553=CARTESIAN_POINT('Ctrl Pts',(-0.218956441427693,-0.564747939904601,
-0.280104693219113));
#40554=CARTESIAN_POINT('Ctrl Pts',(0.0711787765103383,-0.601511215048924,
-0.269729220968394));
#40555=CARTESIAN_POINT('Ctrl Pts',(0.344720332958152,-0.49804623407831,
-0.259353748717676));
#40556=CARTESIAN_POINT('Ctrl Pts',(0.537898409863037,-0.27847344238101,
-0.248978276466957));
#40557=CARTESIAN_POINT('Ctrl Pts',(0.605678082423716,0.00601892164681181,
-0.238602804216239));
#40558=CARTESIAN_POINT('Ctrl Pts',(0.532258067742181,0.289108093990727,
-0.228227331965521));
#40559=CARTESIAN_POINT('Ctrl Pts',(0.334754601270279,0.504798526405128,
-0.217851859714803));
#40560=CARTESIAN_POINT('Ctrl Pts',(0.0592108355069413,0.602806921072019,
-0.207476387464084));
#40561=CARTESIAN_POINT('Ctrl Pts',(-0.230136344857676,0.560285163125383,
-0.197100915213366));
#40562=CARTESIAN_POINT('Ctrl Pts',(-0.465833032609804,0.387145714385472,
-0.186725442962647));
#40563=CARTESIAN_POINT('Ctrl Pts',(-0.592930850937281,0.123752955150168,
-0.176349970711929));
#40564=CARTESIAN_POINT('Ctrl Pts',(-0.581802327327214,-0.168491189905756,
-0.165974498461211));
#40565=CARTESIAN_POINT('Ctrl Pts',(-0.435037041088184,-0.421453016030356,
-0.155599026210493));
#40566=CARTESIAN_POINT('Ctrl Pts',(-0.186859355223635,-0.576167987432484,
-0.145223553959774));
#40567=CARTESIAN_POINT('Ctrl Pts',(0.104892721809184,-0.596552869735825,
-0.134848081709056));
#40568=CARTESIAN_POINT('Ctrl Pts',(0.372166526005229,-0.477885362998166,
-0.124472609458337));
#40569=CARTESIAN_POINT('Ctrl Pts',(0.552730116713414,-0.247769604783317,
-0.114097137207619));
#40570=CARTESIAN_POINT('Ctrl Pts',(0.587112028255095,-0.055912847103633,
-0.10718015570714));
#40571=CARTESIAN_POINT('Ctrl Pts',(0.580853099071723,0.0385046931318555,
-0.103721664956901));
#40572=CARTESIAN_POINT('Ctrl Pts',(0.445651237835157,-0.374523575106288,
-0.12));
#40573=CARTESIAN_POINT('Ctrl Pts',(0.471006333574204,-0.339660302329497,
-0.12));
#40574=CARTESIAN_POINT('Ctrl Pts',(0.506496757742905,-0.286240975539979,
-0.12));
#40575=CARTESIAN_POINT('Ctrl Pts',(0.548090602650708,-0.175383051808221,
-0.12));
#40576=CARTESIAN_POINT('Ctrl Pts',(0.558638194972283,-0.135500469697039,
-0.12));
#40577=CARTESIAN_POINT('Ctrl Pts',(0.571925545859982,-0.0509094028730825,
-0.12));
#40578=CARTESIAN_POINT('Ctrl Pts',(0.573933770267675,-0.00645369735957208,
-0.12));
#40579=CARTESIAN_POINT('Ctrl Pts',(0.570996795169322,0.0378513197440184,
-0.12));
#40580=CARTESIAN_POINT('',(-0.565495273463993,0.0874028629208282,-0.72625));
#40581=CARTESIAN_POINT('Ctrl Pts',(-0.565534825602702,0.0874095162469272,
-0.72625));
#40582=CARTESIAN_POINT('Ctrl Pts',(-0.558753848852679,0.131282067753869,
-0.72625));
#40583=CARTESIAN_POINT('Ctrl Pts',(-0.547115463002498,0.17422512350475,
-0.72625));
#40584=CARTESIAN_POINT('Ctrl Pts',(-0.515734564221166,0.253877204522193,
-0.72625));
#40585=CARTESIAN_POINT('Ctrl Pts',(-0.496760829533906,0.290498979877212,
-0.72625));
#40586=CARTESIAN_POINT('Ctrl Pts',(-0.432021967366878,0.389656916743186,
-0.72625));
#40587=CARTESIAN_POINT('Ctrl Pts',(-0.385735474250614,0.434078643348275,
-0.72625));
#40588=CARTESIAN_POINT('Ctrl Pts',(-0.353390396098499,0.46258854508056,
-0.72625));
#40589=CARTESIAN_POINT('Ctrl Pts',(-0.565495271712367,0.0874028626261757,
-0.726250000000001));
#40590=CARTESIAN_POINT('Ctrl Pts',(-0.56997393358064,0.05848913808605,-0.725162434688994));
#40591=CARTESIAN_POINT('Ctrl Pts',(-0.572256945759171,0.0292370242315025,
-0.724074869377987));
#40592=CARTESIAN_POINT('Ctrl Pts',(-0.57227986394681,-1.09618492728156E-5,
-0.722987304066981));
#40593=CARTESIAN_POINT('Origin',(-1.17892742873597E-16,0.,-0.72625));
#40594=CARTESIAN_POINT('',(-0.6516,-7.97979854324415E-17,-0.72625));
#40595=CARTESIAN_POINT('Origin',(0.,0.,-0.72625));
#40596=CARTESIAN_POINT('Origin',(0.,0.,-0.72625));
#40597=CARTESIAN_POINT('',(0.462889160393653,-0.444455658495748,-0.72625));
#40598=CARTESIAN_POINT('Ctrl Pts',(0.6516,-1.66533453693773E-16,-0.72625));
#40599=CARTESIAN_POINT('Ctrl Pts',(0.6516,-0.0505003751377495,-0.72625));
#40600=CARTESIAN_POINT('Ctrl Pts',(0.645506923582183,-0.100849053895293,
-0.72625));
#40601=CARTESIAN_POINT('Ctrl Pts',(0.622270462633308,-0.195195237486754,
-0.72625));
#40602=CARTESIAN_POINT('Ctrl Pts',(0.606052107869727,-0.239165633749014,
-0.72625));
#40603=CARTESIAN_POINT('Ctrl Pts',(0.546829171420724,-0.35650676310561,
-0.72625));
#40604=CARTESIAN_POINT('Ctrl Pts',(0.499772339104853,-0.410635277409444,
-0.72625));
#40605=CARTESIAN_POINT('Ctrl Pts',(0.462889160393654,-0.444455658495747,
-0.72625));
#40606=CARTESIAN_POINT('',(-0.353390396098496,-0.462588545080562,-0.72625));
#40607=CARTESIAN_POINT('Ctrl Pts',(0.462926795561194,-0.444481916564912,
-0.72625));
#40608=CARTESIAN_POINT('Ctrl Pts',(0.439708289239495,-0.465744192282609,
-0.72625));
#40609=CARTESIAN_POINT('Ctrl Pts',(0.414979050320746,-0.485210232281103,
-0.72625));
#40610=CARTESIAN_POINT('Ctrl Pts',(0.388971950023878,-0.502761089181296,
-0.72625));
#40611=CARTESIAN_POINT('Ctrl Pts',(0.361777826790807,-0.521113006924594,
-0.72625));
#40612=CARTESIAN_POINT('Ctrl Pts',(0.333185315488392,-0.537372018715419,
-0.72625));
#40613=CARTESIAN_POINT('Ctrl Pts',(0.303435179814313,-0.551346893096332,
-0.72625));
#40614=CARTESIAN_POINT('Ctrl Pts',(0.296196613580324,-0.554747148306128,
-0.72625));
#40615=CARTESIAN_POINT('Ctrl Pts',(0.288889451743085,-0.558011890011791,
-0.72625));
#40616=CARTESIAN_POINT('Ctrl Pts',(0.281517080262701,-0.56113778168721,
-0.72625));
#40617=CARTESIAN_POINT('Ctrl Pts',(0.274909983304274,-0.563939196325089,
-0.72625));
#40618=CARTESIAN_POINT('Ctrl Pts',(0.268259434616051,-0.566625287495204,
-0.72625));
#40619=CARTESIAN_POINT('Ctrl Pts',(0.261569430937461,-0.56919401133889,
-0.72625));
#40620=CARTESIAN_POINT('Ctrl Pts',(0.24504403797673,-0.575539175402156,
-0.72625));
#40621=CARTESIAN_POINT('Ctrl Pts',(0.22827539249502,-0.581169692531995,
-0.72625));
#40622=CARTESIAN_POINT('Ctrl Pts',(0.211302790467133,-0.586059341419264,
-0.72625));
#40623=CARTESIAN_POINT('Ctrl Pts',(0.186757466137251,-0.593130621214788,
-0.72625));
#40624=CARTESIAN_POINT('Ctrl Pts',(0.161785415196603,-0.59865351137275,
-0.72625));
#40625=CARTESIAN_POINT('Ctrl Pts',(0.136536085409988,-0.602617904235996,
-0.72625));
#40626=CARTESIAN_POINT('Ctrl Pts',(0.121331994017328,-0.605005095972118,
-0.72625));
#40627=CARTESIAN_POINT('Ctrl Pts',(0.106027319098842,-0.606826713214505,
-0.72625));
#40628=CARTESIAN_POINT('Ctrl Pts',(0.0906551911462363,-0.608076286524706,
-0.72625));
#40629=CARTESIAN_POINT('Ctrl Pts',(0.0807017050580736,-0.608885387944989,
-0.72625));
#40630=CARTESIAN_POINT('Ctrl Pts',(0.0707139335318761,-0.609454531657244,
-0.72625));
#40631=CARTESIAN_POINT('Ctrl Pts',(0.0607349132915466,-0.609780907620945,
-0.72625));
#40632=CARTESIAN_POINT('Ctrl Pts',(0.0304829114827247,-0.610770336042418,
-0.72625));
#40633=CARTESIAN_POINT('Ctrl Pts',(0.00026269855040462,-0.609539106859905,
-0.72625));
#40634=CARTESIAN_POINT('Ctrl Pts',(-0.0296765491183145,-0.606076614826858,
-0.72625));
#40635=CARTESIAN_POINT('Ctrl Pts',(-0.0505970509746303,-0.603657146181342,
-0.72625));
#40636=CARTESIAN_POINT('Ctrl Pts',(-0.0713804846129305,-0.600147135085872,
-0.72625));
#40637=CARTESIAN_POINT('Ctrl Pts',(-0.0919381111643192,-0.595528262125297,
-0.72625));
#40638=CARTESIAN_POINT('Ctrl Pts',(-0.106527466400008,-0.592250336133116,
-0.72625));
#40639=CARTESIAN_POINT('Ctrl Pts',(-0.121003020799398,-0.588413642459459,
-0.72625));
#40640=CARTESIAN_POINT('Ctrl Pts',(-0.135334733667594,-0.584028646208658,
-0.72625));
#40641=CARTESIAN_POINT('Ctrl Pts',(-0.142283241551999,-0.581902649037072,
-0.72625));
#40642=CARTESIAN_POINT('Ctrl Pts',(-0.149197909713515,-0.579647727780099,
-0.72625));
#40643=CARTESIAN_POINT('Ctrl Pts',(-0.156075139006189,-0.577264873365136,
-0.72625));
#40644=CARTESIAN_POINT('Ctrl Pts',(-0.162218696929079,-0.575136224821203,
-0.72625));
#40645=CARTESIAN_POINT('Ctrl Pts',(-0.168323407331897,-0.572908574802006,
-0.72625));
#40646=CARTESIAN_POINT('Ctrl Pts',(-0.174385772185665,-0.570583909329584,
-0.72625));
#40647=CARTESIAN_POINT('Ctrl Pts',(-0.202180396576834,-0.559925823714537,
-0.72625));
#40648=CARTESIAN_POINT('Ctrl Pts',(-0.229096085134795,-0.547228928394159,
-0.72625));
#40649=CARTESIAN_POINT('Ctrl Pts',(-0.254911830827949,-0.532610490159781,
-0.72625));
#40650=CARTESIAN_POINT('Ctrl Pts',(-0.280232930328858,-0.518272150547971,
-0.72625));
#40651=CARTESIAN_POINT('Ctrl Pts',(-0.304496791249199,-0.502084414991184,
-0.72625));
#40652=CARTESIAN_POINT('Ctrl Pts',(-0.327463169349827,-0.484120324940849,
-0.72625));
#40653=CARTESIAN_POINT('Ctrl Pts',(-0.336303377345208,-0.477205595426387,
-0.72625));
#40654=CARTESIAN_POINT('Ctrl Pts',(-0.344950933524855,-0.470027335227127,
-0.72625));
#40655=CARTESIAN_POINT('Ctrl Pts',(-0.353390396098497,-0.462588545080562,
-0.72625));
#40656=CARTESIAN_POINT('Ctrl Pts',(-0.353390396098497,-0.462588545080562,
-0.72625));
#40657=CARTESIAN_POINT('Ctrl Pts',(-0.390098616296541,-0.430232841820501,
-0.72625));
#40658=CARTESIAN_POINT('Ctrl Pts',(-0.444801171208843,-0.377290789425656,
-0.72625));
#40659=CARTESIAN_POINT('Ctrl Pts',(-0.528751914986461,-0.232845672680449,
-0.72625));
#40660=CARTESIAN_POINT('Ctrl Pts',(-0.554058019076711,-0.161663831518696,
-0.72625));
#40661=CARTESIAN_POINT('Ctrl Pts',(-0.565534825602701,-0.0874095162469292,
-0.72625));
#40662=CARTESIAN_POINT('Origin',(0.,0.,-0.72625));
#40663=CARTESIAN_POINT('Origin',(0.,0.,-0.930039011722494));
#40664=CARTESIAN_POINT('Ctrl Pts',(-0.575296847308758,-0.0889183421516984,
-0.742528335043099));
#40665=CARTESIAN_POINT('Ctrl Pts',(-0.560843190848635,-0.182432714916398,
-0.73906984429286));
#40666=CARTESIAN_POINT('Ctrl Pts',(-0.485503739143021,-0.362196725342242,
-0.732152862792381));
#40667=CARTESIAN_POINT('Ctrl Pts',(-0.259159251093108,-0.547465824506594,
-0.721777390541662));
#40668=CARTESIAN_POINT('Ctrl Pts',(0.0275428991067036,-0.605077845001504,
-0.711401918290945));
#40669=CARTESIAN_POINT('Ctrl Pts',(0.307852790782245,-0.521644157320061,
-0.701026446040225));
#40670=CARTESIAN_POINT('Ctrl Pts',(0.516379630382223,-0.316594299265632,
-0.690650973789508));
#40671=CARTESIAN_POINT('Ctrl Pts',(0.604531894922356,-0.037741447613471,
-0.680275501538789));
#40672=CARTESIAN_POINT('Ctrl Pts',(0.551748054568745,0.249911729814406,
-0.669900029288071));
#40673=CARTESIAN_POINT('Ctrl Pts',(0.370338916630071,0.479302937024635,
-0.659524557037353));
#40674=CARTESIAN_POINT('Ctrl Pts',(0.102593005245228,0.596956344106599,
-0.649149084786633));
#40675=CARTESIAN_POINT('Ctrl Pts',(-0.189069595066604,0.575443129800777,
-0.638773612535917));
#40676=CARTESIAN_POINT('Ctrl Pts',(-0.436655282749753,0.419778941359981,
-0.628398140285197));
#40677=CARTESIAN_POINT('Ctrl Pts',(-0.582444898128172,0.166253064936486,
-0.618022668034479));
#40678=CARTESIAN_POINT('Ctrl Pts',(-0.59245118529686,-0.126030790814807,
-0.607647195783762));
#40679=CARTESIAN_POINT('Ctrl Pts',(-0.464341322608817,-0.388933533934673,
-0.597271723533042));
#40680=CARTESIAN_POINT('Ctrl Pts',(-0.227981169867371,-0.561165524309829,
-0.586896251282325));
#40681=CARTESIAN_POINT('Ctrl Pts',(0.0615274613730338,-0.602574918002375,
-0.576520779031606));
#40682=CARTESIAN_POINT('Ctrl Pts',(0.336692401993215,-0.503508078945706,
-0.566145306780887));
#40683=CARTESIAN_POINT('Ctrl Pts',(0.533365395804019,-0.287060123544462,
-0.55576983453017));
#40684=CARTESIAN_POINT('Ctrl Pts',(0.605696737111815,-0.00369082231710978,
-0.545394362279451));
#40685=CARTESIAN_POINT('Ctrl Pts',(0.536824069047151,0.280538907457441,
-0.535018890028733));
#40686=CARTESIAN_POINT('Ctrl Pts',(0.342803440542624,0.499367560825895,
-0.524643417778015));
#40687=CARTESIAN_POINT('Ctrl Pts',(0.0688662178762295,0.601780361666548,
-0.514267945527296));
#40688=CARTESIAN_POINT('Ctrl Pts',(-0.221125550821607,0.563902163890325,
-0.503892473276578));
#40689=CARTESIAN_POINT('Ctrl Pts',(-0.459567075698392,0.394563382218786,
-0.493517001025859));
#40690=CARTESIAN_POINT('Ctrl Pts',(-0.590871299173015,0.133241387995481,
-0.483141528775141));
#40691=CARTESIAN_POINT('Ctrl Pts',(-0.584427716440101,-0.159142715555849,
-0.472766056524423));
#40692=CARTESIAN_POINT('Ctrl Pts',(-0.441738497928306,-0.414426421825547,
-0.462390584273705));
#40693=CARTESIAN_POINT('Ctrl Pts',(-0.196068293388198,-0.573096313010961,
-0.452015112022986));
#40694=CARTESIAN_POINT('Ctrl Pts',(0.0953106421677161,-0.598162219760071,
-0.441639639772268));
#40695=CARTESIAN_POINT('Ctrl Pts',(0.364470133516224,-0.483780612916302,
-0.43126416752155));
#40696=CARTESIAN_POINT('Ctrl Pts',(0.548661948506927,-0.256616885491388,
-0.420888695270832));
#40697=CARTESIAN_POINT('Ctrl Pts',(0.60494607893493,0.0303710592533639,
-0.410513223020113));
#40698=CARTESIAN_POINT('Ctrl Pts',(0.520201197869222,0.310278702773021,
-0.400137750769395));
#40699=CARTESIAN_POINT('Ctrl Pts',(0.314183589749731,0.517852132939369,
-0.389762278518676));
#40700=CARTESIAN_POINT('Ctrl Pts',(0.0349214353255983,0.604700465533282,
-0.379386806267958));
#40701=CARTESIAN_POINT('Ctrl Pts',(-0.252481833942362,0.550577045637576,
-0.36901133401724));
#40702=CARTESIAN_POINT('Ctrl Pts',(-0.481024876325774,0.368099481148946,
-0.358635861766521));
#40703=CARTESIAN_POINT('Ctrl Pts',(-0.597428233573601,0.0998081428603092,
-0.348260389515803));
#40704=CARTESIAN_POINT('Ctrl Pts',(-0.574555188931242,-0.191751126529284,
-0.337884917265085));
#40705=CARTESIAN_POINT('Ctrl Pts',(-0.417738057072088,-0.43860811139261,
-0.327509445014367));
#40706=CARTESIAN_POINT('Ctrl Pts',(-0.163535079971663,-0.583213886268098,
-0.317133972763648));
#40707=CARTESIAN_POINT('Ctrl Pts',(0.128792271407237,-0.591857001983,-0.30675850051293));
#40708=CARTESIAN_POINT('Ctrl Pts',(0.3910947206114,-0.462522516893444,-0.296383028262211));
#40709=CARTESIAN_POINT('Ctrl Pts',(0.562222594861329,-0.225361740621548,
-0.286007556011493));
#40710=CARTESIAN_POINT('Ctrl Pts',(0.602281436660628,0.0643368521302563,
-0.275632083760774));
#40711=CARTESIAN_POINT('Ctrl Pts',(0.501932467413927,0.339036806050298,
-0.265256611510057));
#40712=CARTESIAN_POINT('Ctrl Pts',(0.284569694815385,0.534698285003551,
-0.254881139259338));
#40713=CARTESIAN_POINT('Ctrl Pts',(0.00086616792234151,0.605707347412463,
-0.24450566700862));
#40714=CARTESIAN_POINT('Ctrl Pts',(-0.283039297466054,0.535509992112656,
-0.234130194757901));
#40715=CARTESIAN_POINT('Ctrl Pts',(-0.500960755684866,0.340470892555017,
-0.223754722507184));
#40716=CARTESIAN_POINT('Ctrl Pts',(-0.602094991516589,0.066059236182406,
-0.213379250256465));
#40717=CARTESIAN_POINT('Ctrl Pts',(-0.562864788572229,-0.223753096954469,
-0.203003778005747));
#40718=CARTESIAN_POINT('Ctrl Pts',(-0.392416023107415,-0.46140161814604,
-0.192628305755028));
#40719=CARTESIAN_POINT('Ctrl Pts',(-0.130484291345699,-0.591487175311845,
-0.18225283350431));
#40720=CARTESIAN_POINT('Ctrl Pts',(0.161866082666176,-0.583677346042729,
-0.171877361253592));
#40721=CARTESIAN_POINT('Ctrl Pts',(0.416482587440825,-0.439804754427654,
-0.161501889002873));
#40722=CARTESIAN_POINT('Ctrl Pts',(0.574003120398452,-0.193386213509922,
-0.151126416752155));
#40723=CARTESIAN_POINT('Ctrl Pts',(0.597713822063416,0.0980843175241036,
-0.140750944501437));
#40724=CARTESIAN_POINT('Ctrl Pts',(0.482070740684944,0.366753526971408,
-0.130375472250718));
#40725=CARTESIAN_POINT('Ctrl Pts',(0.33006409929725,0.48875809000787,-0.12345849075024));
#40726=CARTESIAN_POINT('Ctrl Pts',(0.244165145742818,0.528447079373888,
-0.12));
#40727=CARTESIAN_POINT('Ctrl Pts',(-0.572789913424251,-0.088530868439758,
-0.741207811940174));
#40728=CARTESIAN_POINT('Ctrl Pts',(-0.558399233618351,-0.181637785669948,
-0.737749321189935));
#40729=CARTESIAN_POINT('Ctrl Pts',(-0.483388100289454,-0.360618378632632,
-0.730832339689455));
#40730=CARTESIAN_POINT('Ctrl Pts',(-0.258029928191081,-0.545080184451301,
-0.720456867438737));
#40731=CARTESIAN_POINT('Ctrl Pts',(0.0274228758760488,-0.602441133683186,
-0.71008139518802));
#40732=CARTESIAN_POINT('Ctrl Pts',(0.306511283236796,-0.519371028784781,
-0.699705922937301));
#40733=CARTESIAN_POINT('Ctrl Pts',(0.514129439073967,-0.315214697079695,
-0.689330450686582));
#40734=CARTESIAN_POINT('Ctrl Pts',(0.601897569304816,-0.0375769852070561,
-0.678954978435864));
#40735=CARTESIAN_POINT('Ctrl Pts',(0.549343741066101,0.248822707591735,
-0.668579506185146));
#40736=CARTESIAN_POINT('Ctrl Pts',(0.368725117019615,0.477214312364194,
-0.658204033934427));
#40737=CARTESIAN_POINT('Ctrl Pts',(0.102145942950475,0.594355029845439,
-0.64782856168371));
#40738=CARTESIAN_POINT('Ctrl Pts',(-0.188245699875266,0.572935561990258,
-0.63745308943299));
#40739=CARTESIAN_POINT('Ctrl Pts',(-0.434752500966896,0.417949700435014,
-0.627077617182273));
#40740=CARTESIAN_POINT('Ctrl Pts',(-0.579906819258096,0.165528595720715,
-0.616702144931554));
#40741=CARTESIAN_POINT('Ctrl Pts',(-0.589869502742826,-0.125481595359992,
-0.606326672680836));
#40742=CARTESIAN_POINT('Ctrl Pts',(-0.462317895324597,-0.387238705832832,
-0.595951200430118));
#40743=CARTESIAN_POINT('Ctrl Pts',(-0.226987712476072,-0.558720173060809,
-0.585575728179399));
#40744=CARTESIAN_POINT('Ctrl Pts',(0.061259347513968,-0.599949119974886,
-0.575200255928681));
#40745=CARTESIAN_POINT('Ctrl Pts',(0.335225221367258,-0.501313977462673,
-0.564824783677962));
#40746=CARTESIAN_POINT('Ctrl Pts',(0.531041187207166,-0.285809221982231,
-0.554449311427245));
#40747=CARTESIAN_POINT('Ctrl Pts',(0.603057335353469,-0.00367473908207673,
-0.544073839176526));
#40748=CARTESIAN_POINT('Ctrl Pts',(0.534484788834912,0.27931642293625,-0.533698366925808));
#40749=CARTESIAN_POINT('Ctrl Pts',(0.341309630277037,0.497191502185792,
-0.523322894675089));
#40750=CARTESIAN_POINT('Ctrl Pts',(0.0685661244376943,0.599158026020019,
-0.512947422424371));
#40751=CARTESIAN_POINT('Ctrl Pts',(-0.220161967675312,0.561444887382637,
-0.502571950173652));
#40752=CARTESIAN_POINT('Ctrl Pts',(-0.457564452812476,0.392844021322498,
-0.492196477922934));
#40753=CARTESIAN_POINT('Ctrl Pts',(-0.588296501175234,0.132660771439031,
-0.481821005672216));
#40754=CARTESIAN_POINT('Ctrl Pts',(-0.581880997186273,-0.15844923061937,
-0.471445533421498));
#40755=CARTESIAN_POINT('Ctrl Pts',(-0.439813565372604,-0.412620505168844,
-0.461070061170779));
#40756=CARTESIAN_POINT('Ctrl Pts',(-0.195213900477338,-0.570598971811038,
-0.450694588920061));
#40757=CARTESIAN_POINT('Ctrl Pts',(0.0948953137350028,-0.595555650634202,
-0.440319116669343));
#40758=CARTESIAN_POINT('Ctrl Pts',(0.362881907837736,-0.481672476414757,
-0.429943644418624));
#40759=CARTESIAN_POINT('Ctrl Pts',(0.546271083206054,-0.255498644270525,
-0.419568172167906));
#40760=CARTESIAN_POINT('Ctrl Pts',(0.602309948266564,0.0302387134402138,
-0.409192699917188));
#40761=CARTESIAN_POINT('Ctrl Pts',(0.517934353964987,0.308926623252875,
-0.398817227666469));
#40762=CARTESIAN_POINT('Ctrl Pts',(0.312814494180264,0.51559552538895,-0.388441755415751));
#40763=CARTESIAN_POINT('Ctrl Pts',(0.0347692606610258,0.602065405157036,
-0.378066283165032));
#40764=CARTESIAN_POINT('Ctrl Pts',(-0.251381611742667,0.548177835053618,
-0.367690810914315));
#40765=CARTESIAN_POINT('Ctrl Pts',(-0.478928748302335,0.366495440119418,
-0.357315338663596));
#40766=CARTESIAN_POINT('Ctrl Pts',(-0.594824862887321,0.0993732159874641,
-0.346939866412878));
#40767=CARTESIAN_POINT('Ctrl Pts',(-0.572051490491107,-0.190915546230564,
-0.336564394162159));
#40768=CARTESIAN_POINT('Ctrl Pts',(-0.415917709537047,-0.436696819900557,
-0.326188921911441));
#40769=CARTESIAN_POINT('Ctrl Pts',(-0.162822454740063,-0.580672456435957,
-0.315813449660722));
#40770=CARTESIAN_POINT('Ctrl Pts',(0.128231042451125,-0.589277908658029,
-0.305437977410005));
#40771=CARTESIAN_POINT('Ctrl Pts',(0.389390474855656,-0.460507015290604,
-0.295062505159286));
#40772=CARTESIAN_POINT('Ctrl Pts',(0.55977263729338,-0.224379697731525,
-0.284687032908568));
#40773=CARTESIAN_POINT('Ctrl Pts',(0.599656917513555,0.0640564959887923,
-0.274311560657849));
#40774=CARTESIAN_POINT('Ctrl Pts',(0.499745231865169,0.337559409379268,
-0.263936088407131));
#40775=CARTESIAN_POINT('Ctrl Pts',(0.283329645611625,0.532368268173216,
-0.253560616156412));
#40776=CARTESIAN_POINT('Ctrl Pts',(0.000862393495920531,0.603067899411643,
-0.243185143905695));
#40777=CARTESIAN_POINT('Ctrl Pts',(-0.281805917196665,0.533176438173738,
-0.232809671654976));
#40778=CARTESIAN_POINT('Ctrl Pts',(-0.498777754444496,0.338987246642003,
-0.222434199404258));
#40779=CARTESIAN_POINT('Ctrl Pts',(-0.59947128492484,0.0657713745817691,
-0.21205872715354));
#40780=CARTESIAN_POINT('Ctrl Pts',(-0.560412032373069,-0.22277806404098,
-0.201683254902822));
#40781=CARTESIAN_POINT('Ctrl Pts',(-0.390706019979498,-0.459391000797317,
-0.191307782652103));
#40782=CARTESIAN_POINT('Ctrl Pts',(-0.129915688452667,-0.588909693965184,
-0.180932310401385));
#40783=CARTESIAN_POINT('Ctrl Pts',(0.161160728835196,-0.581133895809618,
-0.170556838150666));
#40784=CARTESIAN_POINT('Ctrl Pts',(0.414667713695017,-0.437888250026621,
-0.160181365899948));
#40785=CARTESIAN_POINT('Ctrl Pts',(0.571501821867847,-0.192543504893118,
-0.14980589364923));
#40786=CARTESIAN_POINT('Ctrl Pts',(0.59510921853944,0.0976568959835189,
-0.139430421398511));
#40787=CARTESIAN_POINT('Ctrl Pts',(0.479970030309954,0.365155364897378,
-0.129054949147793));
#40788=CARTESIAN_POINT('Ctrl Pts',(0.328625842563643,0.48662824094783,-0.122137967647314));
#40789=CARTESIAN_POINT('Ctrl Pts',(0.243101163069974,0.526144299694755,
-0.118679476897075));
#40790=CARTESIAN_POINT('Ctrl Pts',(-0.567659051683199,-0.0877378383337212,
-0.736720279419894));
#40791=CARTESIAN_POINT('Ctrl Pts',(-0.553397145962568,-0.180011594221972,
-0.733261788669655));
#40792=CARTESIAN_POINT('Ctrl Pts',(-0.479058246054666,-0.357387603482484,
-0.726344807169176));
#40793=CARTESIAN_POINT('Ctrl Pts',(-0.255718555936061,-0.540197843291853,
-0.715969334918457));
#40794=CARTESIAN_POINT('Ctrl Pts',(0.0271772062107107,-0.597044615620193,
-0.70559386266774));
#40795=CARTESIAN_POINT('Ctrl Pts',(0.303765706721173,-0.514718796922303,
-0.695218390417021));
#40796=CARTESIAN_POINT('Ctrl Pts',(0.509524091217568,-0.31239111466724,
-0.684842918166304));
#40797=CARTESIAN_POINT('Ctrl Pts',(0.596506044544102,-0.0372404028672287,
-0.674467445915583));
#40798=CARTESIAN_POINT('Ctrl Pts',(0.544422964561454,0.246593873216988,
-0.664091973664867));
#40799=CARTESIAN_POINT('Ctrl Pts',(0.365422243793962,0.472939636786017,
-0.653716501414147));
#40800=CARTESIAN_POINT('Ctrl Pts',(0.101230964976293,0.589031066186152,
-0.643341029163429));
#40801=CARTESIAN_POINT('Ctrl Pts',(-0.186559479142561,0.567803461338418,
-0.632965556912711));
#40802=CARTESIAN_POINT('Ctrl Pts',(-0.430858183277496,0.414205895078914,
-0.622590084661993));
#40803=CARTESIAN_POINT('Ctrl Pts',(-0.574712274150216,0.164045864589158,
-0.612214612411273));
#40804=CARTESIAN_POINT('Ctrl Pts',(-0.584585716474985,-0.12435758741187,
-0.601839140160557));
#40805=CARTESIAN_POINT('Ctrl Pts',(-0.458176659071989,-0.383769995346564,
-0.591463667909837));
#40806=CARTESIAN_POINT('Ctrl Pts',(-0.224954458417602,-0.553715408447872,
-0.58108819565912));
#40807=CARTESIAN_POINT('Ctrl Pts',(0.0607106137732936,-0.594575045006088,
-0.570712723408401));
#40808=CARTESIAN_POINT('Ctrl Pts',(0.332222424267133,-0.496823431812653,
-0.560337251157683));
#40809=CARTESIAN_POINT('Ctrl Pts',(0.526284358561762,-0.283249071234861,
-0.549961778906964));
#40810=CARTESIAN_POINT('Ctrl Pts',(0.597655418369305,-0.00364182241635053,
-0.539586306656246));
#40811=CARTESIAN_POINT('Ctrl Pts',(0.529697113950753,0.276814431763831,
-0.529210834405528));
#40812=CARTESIAN_POINT('Ctrl Pts',(0.3382523317741,0.492737883828088,-0.51883536215481));
#40813=CARTESIAN_POINT('Ctrl Pts',(0.0679519398645962,0.593791037299236,
-0.508459889904091));
#40814=CARTESIAN_POINT('Ctrl Pts',(-0.21818985556821,0.556415716034123,
-0.498084417653373));
#40815=CARTESIAN_POINT('Ctrl Pts',(-0.453465795779581,0.389325100871067,
-0.487708945402654));
#40816=CARTESIAN_POINT('Ctrl Pts',(-0.583026805120096,0.131472455781011,
-0.477333473151936));
#40817=CARTESIAN_POINT('Ctrl Pts',(-0.576668768336853,-0.157029913516757,
-0.466958000901218));
#40818=CARTESIAN_POINT('Ctrl Pts',(-0.43587391282357,-0.40892443585002,
-0.4565825286505));
#40819=CARTESIAN_POINT('Ctrl Pts',(-0.193465261960535,-0.565487802282046,
-0.446207056399781));
#40820=CARTESIAN_POINT('Ctrl Pts',(0.0940452840995342,-0.590220930375798,
-0.435831584149063));
#40821=CARTESIAN_POINT('Ctrl Pts',(0.359631374553251,-0.477357870525102,
-0.425456111898345));
#40822=CARTESIAN_POINT('Ctrl Pts',(0.54137783198586,-0.253210002072044,
-0.415080639647626));
#40823=CARTESIAN_POINT('Ctrl Pts',(0.596914726041016,0.0299678486150587,
-0.404705167396908));
#40824=CARTESIAN_POINT('Ctrl Pts',(0.513294930449014,0.306159397194876,
-0.394329695146189));
#40825=CARTESIAN_POINT('Ctrl Pts',(0.310012442319218,0.510977052049793,
-0.383954222895472));
#40826=CARTESIAN_POINT('Ctrl Pts',(0.0344578132269551,0.596672373438936,
-0.373578750644753));
#40827=CARTESIAN_POINT('Ctrl Pts',(-0.249129848073962,0.54326750400601,
-0.363203278394035));
#40828=CARTESIAN_POINT('Ctrl Pts',(-0.474638719497963,0.36321253843442,
-0.352827806143316));
#40829=CARTESIAN_POINT('Ctrl Pts',(-0.589496688697369,0.0984830753129765,
-0.342452333892598));
#40830=CARTESIAN_POINT('Ctrl Pts',(-0.566927309952081,-0.189205410441921,
-0.33207686164188));
#40831=CARTESIAN_POINT('Ctrl Pts',(-0.412192105340198,-0.432785085759324,
-0.321701389391161));
#40832=CARTESIAN_POINT('Ctrl Pts',(-0.161363964260157,-0.575471053151198,
-0.311325917140443));
#40833=CARTESIAN_POINT('Ctrl Pts',(0.127082406321203,-0.583999421597136,
-0.300950444889725));
#40834=CARTESIAN_POINT('Ctrl Pts',(0.385902489716337,-0.456382000099439,
-0.290574972639006));
#40835=CARTESIAN_POINT('Ctrl Pts',(0.554758445225278,-0.222369805099424,
-0.280199500388288));
#40836=CARTESIAN_POINT('Ctrl Pts',(0.594285459917798,0.0634827066596925,
-0.26982402813757));
#40837=CARTESIAN_POINT('Ctrl Pts',(0.495268738400242,0.334535703640292,
-0.259448555886852));
#40838=CARTESIAN_POINT('Ctrl Pts',(0.2807917056779,0.527599552194623,-0.249073083636133));
#40839=CARTESIAN_POINT('Ctrl Pts',(0.000854668789314793,0.597665887673856,
-0.238697611385415));
#40840=CARTESIAN_POINT('Ctrl Pts',(-0.279281626703832,0.528400483157397,
-0.228322139134696));
#40841=CARTESIAN_POINT('Ctrl Pts',(-0.494309926255865,0.33595075051375,
-0.217946666883978));
#40842=CARTESIAN_POINT('Ctrl Pts',(-0.594101491946025,0.0651822251072623,
-0.20757119463326));
#40843=CARTESIAN_POINT('Ctrl Pts',(-0.555392109356301,-0.220782520067741,
-0.197195722382542));
#40844=CARTESIAN_POINT('Ctrl Pts',(-0.387206257766804,-0.455275978496852,
-0.186820250131823));
#40845=CARTESIAN_POINT('Ctrl Pts',(-0.12875194816593,-0.583634512881856,
-0.176444777881105));
#40846=CARTESIAN_POINT('Ctrl Pts',(0.159717095872789,-0.575928343928385,
-0.166069305630386));
#40847=CARTESIAN_POINT('Ctrl Pts',(0.410953360921151,-0.433965873811025,
-0.155693833379668));
#40848=CARTESIAN_POINT('Ctrl Pts',(0.56638245664278,-0.19081872650705,-0.14531836112895));
#40849=CARTESIAN_POINT('Ctrl Pts',(0.589778714899386,0.0967820086525517,
-0.134942888878231));
#40850=CARTESIAN_POINT('Ctrl Pts',(0.475670209653462,0.361884724579745,
-0.124567416627513));
#40851=CARTESIAN_POINT('Ctrl Pts',(0.325682910944071,0.482268822061771,
-0.117650435127034));
#40852=CARTESIAN_POINT('Ctrl Pts',(0.240923543618988,0.52143127386398,-0.114191944376795));
#40853=CARTESIAN_POINT('Ctrl Pts',(-0.565534825602701,-0.0874095162469292,
-0.730063108302008));
#40854=CARTESIAN_POINT('Ctrl Pts',(-0.551326779224584,-0.179334805112556,
-0.726604617551768));
#40855=CARTESIAN_POINT('Ctrl Pts',(-0.477264922845315,-0.356051984665031,
-0.719687636051289));
#40856=CARTESIAN_POINT('Ctrl Pts',(-0.254761731927526,-0.53817525012622,
-0.70931216380057));
#40857=CARTESIAN_POINT('Ctrl Pts',(0.0270755978711435,-0.594810612863019,
-0.698936691549854));
#40858=CARTESIAN_POINT('Ctrl Pts',(0.302628807416583,-0.512792230164359,
-0.688561219299133));
#40859=CARTESIAN_POINT('Ctrl Pts',(0.50761721588506,-0.311222099281607,
-0.678185747048417));
#40860=CARTESIAN_POINT('Ctrl Pts',(0.594273598793385,-0.0371009731803471,
-0.667810274797697));
#40861=CARTESIAN_POINT('Ctrl Pts',(0.542385460253111,0.245670963329659,
-0.65743480254698));
#40862=CARTESIAN_POINT('Ctrl Pts',(0.364054642350776,0.471169667728722,
-0.647059330296261));
#40863=CARTESIAN_POINT('Ctrl Pts',(0.100852108287779,0.586826601489527,
-0.636683858045543));
#40864=CARTESIAN_POINT('Ctrl Pts',(-0.18586127840427,0.565678452235062,
-0.626308385794825));
#40865=CARTESIAN_POINT('Ctrl Pts',(-0.429245689780927,0.412655721589033,
-0.615932913544106));
#40866=CARTESIAN_POINT('Ctrl Pts',(-0.57256140525216,0.163431921469813,
-0.605557441293388));
#40867=CARTESIAN_POINT('Ctrl Pts',(-0.582397895750055,-0.123892177788475,
-0.59518196904267));
#40868=CARTESIAN_POINT('Ctrl Pts',(-0.456461926261484,-0.382333730273898,
-0.58480649679195));
#40869=CARTESIAN_POINT('Ctrl Pts',(-0.224112563030628,-0.551643120531786,
-0.574431024541234));
#40870=CARTESIAN_POINT('Ctrl Pts',(0.0604834033970661,-0.592349839120952,
-0.564055552290514));
#40871=CARTESIAN_POINT('Ctrl Pts',(0.330979076979619,-0.494964062864097,
-0.553680080039796));
#40872=CARTESIAN_POINT('Ctrl Pts',(0.524314731628871,-0.282189007416862,
-0.543304607789078));
#40873=CARTESIAN_POINT('Ctrl Pts',(0.59541868420382,-0.00362819285028554,
-0.53292913553836));
#40874=CARTESIAN_POINT('Ctrl Pts',(0.527714714733413,0.275778449697644,
-0.522553663287641));
#40875=CARTESIAN_POINT('Ctrl Pts',(0.336986417462755,0.490893805070386,
-0.512178191036923));
#40876=CARTESIAN_POINT('Ctrl Pts',(0.0676976287329768,0.591568765635781,
-0.501802718786204));
#40877=CARTESIAN_POINT('Ctrl Pts',(-0.217373276834094,0.554333322057082,
-0.491427246535487));
#40878=CARTESIAN_POINT('Ctrl Pts',(-0.45176869338931,0.387868045972245,
-0.481051774284768));
#40879=CARTESIAN_POINT('Ctrl Pts',(-0.580844818752399,0.130980418187211,
-0.47067630203405));
#40880=CARTESIAN_POINT('Ctrl Pts',(-0.574510577015094,-0.15644222676267,
-0.460300829783332));
#40881=CARTESIAN_POINT('Ctrl Pts',(-0.434242648313164,-0.407394030152414,
-0.449925357532613));
#40882=CARTESIAN_POINT('Ctrl Pts',(-0.192741215380677,-0.563371455889674,
-0.439549885281895));
#40883=CARTESIAN_POINT('Ctrl Pts',(0.0936933182447148,-0.588012019888873,
-0.429174413031176));
#40884=CARTESIAN_POINT('Ctrl Pts',(0.358285448860346,-0.475571351694678,
-0.418798940780458));
#40885=CARTESIAN_POINT('Ctrl Pts',(0.539351717510894,-0.252262359926223,
-0.40842346852974));
#40886=CARTESIAN_POINT('Ctrl Pts',(0.594680763925633,0.0298556935021776,
-0.398047996279021));
#40887=CARTESIAN_POINT('Ctrl Pts',(0.511373916644878,0.305013591161334,
-0.387672524028303));
#40888=CARTESIAN_POINT('Ctrl Pts',(0.308852216207758,0.509064712939559,
-0.377297051777585));
#40889=CARTESIAN_POINT('Ctrl Pts',(0.0343288543557777,0.594439318331672,
-0.366921579526867));
#40890=CARTESIAN_POINT('Ctrl Pts',(-0.24819747596453,0.541234317405916,
-0.356546107276148));
#40891=CARTESIAN_POINT('Ctrl Pts',(-0.47286237712969,0.361853210182931,
-0.34617063502543));
#40892=CARTESIAN_POINT('Ctrl Pts',(-0.587290488696427,0.0981145009599544,
-0.335795162774712));
#40893=CARTESIAN_POINT('Ctrl Pts',(-0.564805576179397,-0.188497306419811,
-0.325419690523993));
#40894=CARTESIAN_POINT('Ctrl Pts',(-0.410649470345074,-0.431165381227568,
-0.315044218273275));
#40895=CARTESIAN_POINT('Ctrl Pts',(-0.160760057250731,-0.573317344299916,
-0.304668746022556));
#40896=CARTESIAN_POINT('Ctrl Pts',(0.126606798538242,-0.581813795190408,
-0.294293273771839));
#40897=CARTESIAN_POINT('Ctrl Pts',(0.384458244017007,-0.454673983786817,
-0.28391780152112));
#40898=CARTESIAN_POINT('Ctrl Pts',(0.552682253554872,-0.22153758281298,
-0.273542329270402));
#40899=CARTESIAN_POINT('Ctrl Pts',(0.592061337976905,0.0632451216395426,
-0.263166857019683));
#40900=CARTESIAN_POINT('Ctrl Pts',(0.493415187671003,0.333283698981943,
-0.252791384768965));
#40901=CARTESIAN_POINT('Ctrl Pts',(0.279740839024693,0.525625002899427,
-0.242415912518246));
#40902=CARTESIAN_POINT('Ctrl Pts',(0.000851469340100179,0.595429114790003,
-0.232040440267529));
#40903=CARTESIAN_POINT('Ctrl Pts',(-0.278236409456736,0.526422935678427,
-0.22166496801681));
#40904=CARTESIAN_POINT('Ctrl Pts',(-0.492459967408646,0.334693451733073,
-0.211289495766092));
#40905=CARTESIAN_POINT('Ctrl Pts',(-0.591878051853725,0.064938276044851,
-0.200914023515373));
#40906=CARTESIAN_POINT('Ctrl Pts',(-0.553313559229366,-0.219956231049899,
-0.190538551264655));
#40907=CARTESIAN_POINT('Ctrl Pts',(-0.385757106908071,-0.453572115751417,
-0.180163079013937));
#40908=CARTESIAN_POINT('Ctrl Pts',(-0.128270143213515,-0.581450223831547,
-0.169787606763218));
#40909=CARTESIAN_POINT('Ctrl Pts',(0.159119453673079,-0.573772979850855,
-0.1594121345125));
#40910=CARTESIAN_POINT('Ctrl Pts',(0.409415160784161,-0.432341638655589,
-0.149036662261782));
#40911=CARTESIAN_POINT('Ctrl Pts',(0.564263161836264,-0.190104806275652,
-0.138661190011064));
#40912=CARTESIAN_POINT('Ctrl Pts',(0.587570656259513,0.0964202458298895,
-0.128285717760345));
#40913=CARTESIAN_POINT('Ctrl Pts',(0.473891720790759,0.360529415344193,
-0.117910245509627));
#40914=CARTESIAN_POINT('Ctrl Pts',(0.324461266232845,0.480465479019555,
-0.110993264009148));
#40915=CARTESIAN_POINT('Ctrl Pts',(0.240021988234213,0.519480035866726,
-0.107534773258909));
#40916=CARTESIAN_POINT('Ctrl Pts',(-0.565534825602701,-0.0874095162469292,
-0.72625));
#40917=CARTESIAN_POINT('Ctrl Pts',(-0.551326428453064,-0.179337074585254,
-0.722791509249761));
#40918=CARTESIAN_POINT('Ctrl Pts',(-0.477265386956567,-0.356050729042777,
-0.715874527749281));
#40919=CARTESIAN_POINT('Ctrl Pts',(-0.254761663575757,-0.538176058210883,
-0.705499055498564));
#40920=CARTESIAN_POINT('Ctrl Pts',(0.0270755327719408,-0.594810479406871,
-0.695123583247846));
#40921=CARTESIAN_POINT('Ctrl Pts',(0.302628938713621,-0.512792550344605,
-0.684748110997126));
#40922=CARTESIAN_POINT('Ctrl Pts',(0.507617355421152,-0.311222115434097,
-0.674372638746409));
#40923=CARTESIAN_POINT('Ctrl Pts',(0.594273793373837,-0.0371010254861046,
-0.66399716649569));
#40924=CARTESIAN_POINT('Ctrl Pts',(0.542385624529068,0.245671060423536,
-0.653621694244972));
#40925=CARTESIAN_POINT('Ctrl Pts',(0.364054758182736,0.471169804196079,
-0.643246221994254));
#40926=CARTESIAN_POINT('Ctrl Pts',(0.100852138510465,0.586826789571409,
-0.632870749743535));
#40927=CARTESIAN_POINT('Ctrl Pts',(-0.185861335713837,0.565678625875551,
-0.622495277492817));
#40928=CARTESIAN_POINT('Ctrl Pts',(-0.429245823844828,0.412655851503898,
-0.612119805242099));
#40929=CARTESIAN_POINT('Ctrl Pts',(-0.572561583514668,0.163431971728343,
-0.601744332991379));
#40930=CARTESIAN_POINT('Ctrl Pts',(-0.582398077309737,-0.123892216057582,
-0.591368860740663));
#40931=CARTESIAN_POINT('Ctrl Pts',(-0.4564620684611,-0.382333849583464,
-0.580993388489942));
#40932=CARTESIAN_POINT('Ctrl Pts',(-0.224112632886457,-0.551643292344488,
-0.570617916239226));
#40933=CARTESIAN_POINT('Ctrl Pts',(0.0604834222543564,-0.592350023747205,
-0.560242443988507));
#40934=CARTESIAN_POINT('Ctrl Pts',(0.330979180111506,-0.494964217078851,
-0.549866971737789));
#40935=CARTESIAN_POINT('Ctrl Pts',(0.524314895013938,-0.282189095361197,
-0.539491499487071));
#40936=CARTESIAN_POINT('Ctrl Pts',(0.595418869741894,-0.00362819397533901,
-0.529116027236352));
#40937=CARTESIAN_POINT('Ctrl Pts',(0.527714879176066,0.27577853563061,-0.518740554985634));
#40938=CARTESIAN_POINT('Ctrl Pts',(0.336986522471297,0.490893958039981,
-0.508365082734915));
#40939=CARTESIAN_POINT('Ctrl Pts',(0.0676976498285046,0.591568949974742,
-0.497989610484197));
#40940=CARTESIAN_POINT('Ctrl Pts',(-0.217373344570204,0.554333494794116,
-0.487614138233479));
#40941=CARTESIAN_POINT('Ctrl Pts',(-0.451768834165619,0.387868166836234,
-0.47723866598276));
#40942=CARTESIAN_POINT('Ctrl Pts',(-0.580844999750384,0.130980459002316,
-0.466863193732042));
#40943=CARTESIAN_POINT('Ctrl Pts',(-0.574510756039226,-0.156442275511923,
-0.456487721481324));
#40944=CARTESIAN_POINT('Ctrl Pts',(-0.434242783628202,-0.407394157101084,
-0.446112249230605));
#40945=CARTESIAN_POINT('Ctrl Pts',(-0.192741275441066,-0.563371631442748,
-0.435736776979888));
#40946=CARTESIAN_POINT('Ctrl Pts',(0.0936933474406337,-0.588012203120214,
-0.425361304729168));
#40947=CARTESIAN_POINT('Ctrl Pts',(0.35828556050624,-0.475571499888217,
-0.414985832478451));
#40948=CARTESIAN_POINT('Ctrl Pts',(0.539351885579122,-0.252262438534088,
-0.404610360227732));
#40949=CARTESIAN_POINT('Ctrl Pts',(0.594680949235049,0.0298557028055502,
-0.394234887977014));
#40950=CARTESIAN_POINT('Ctrl Pts',(0.511374075994885,0.30501368620711,-0.383859415726295));
#40951=CARTESIAN_POINT('Ctrl Pts',(0.308852312449722,0.509064871569989,
-0.373483943475578));
#40952=CARTESIAN_POINT('Ctrl Pts',(0.0343288650529642,0.594439503565886,
-0.363108471224859));
#40953=CARTESIAN_POINT('Ctrl Pts',(-0.248197553305573,0.5412344860607,-0.352732998974141));
#40954=CARTESIAN_POINT('Ctrl Pts',(-0.472862524479398,0.361853322940755,
-0.342357526723422));
#40955=CARTESIAN_POINT('Ctrl Pts',(-0.5872906717023,0.0981145315332149,
-0.331982054472704));
#40956=CARTESIAN_POINT('Ctrl Pts',(-0.564805752180611,-0.188497365157053,
-0.321606582221986));
#40957=CARTESIAN_POINT('Ctrl Pts',(-0.410649598305695,-0.431165515585077,
-0.311231109971268));
#40958=CARTESIAN_POINT('Ctrl Pts',(-0.160760107350392,-0.57331752294948,
-0.300855637720549));
#40959=CARTESIAN_POINT('Ctrl Pts',(0.126606838000238,-0.581813976495778,
-0.290480165469831));
#40960=CARTESIAN_POINT('Ctrl Pts',(0.3844583637991,-0.454674125457656,-0.280104693219112));
#40961=CARTESIAN_POINT('Ctrl Pts',(0.552682425815823,-0.221537651868143,
-0.269729220968394));
#40962=CARTESIAN_POINT('Ctrl Pts',(0.592061522393167,0.0632451413900827,
-0.259353748717676));
#40963=CARTESIAN_POINT('Ctrl Pts',(0.493415341577429,0.333283802752439,
-0.248978276466957));
#40964=CARTESIAN_POINT('Ctrl Pts',(0.279740925892577,0.525625166857998,
-0.238602804216239));
#40965=CARTESIAN_POINT('Ctrl Pts',(0.000851470205678055,0.595429299999864,
-0.228227331965521));
#40966=CARTESIAN_POINT('Ctrl Pts',(-0.278236497349112,0.526423100377946,
-0.217851859714802));
#40967=CARTESIAN_POINT('Ctrl Pts',(-0.492460118502939,0.334693554718123,
-0.207476387464084));
#40968=CARTESIAN_POINT('Ctrl Pts',(-0.591878240975039,0.0649382988775781,
-0.197100915213366));
#40969=CARTESIAN_POINT('Ctrl Pts',(-0.553313722354291,-0.219956304742787,
-0.186725442962648));
#40970=CARTESIAN_POINT('Ctrl Pts',(-0.385757245550577,-0.453572246869937,
-0.176349970711929));
#40971=CARTESIAN_POINT('Ctrl Pts',(-0.128270146612636,-0.581450425290948,
-0.165974498461211));
#40972=CARTESIAN_POINT('Ctrl Pts',(0.159119430707533,-0.573773118428659,
-0.155599026210492));
#40973=CARTESIAN_POINT('Ctrl Pts',(0.409415432322886,-0.432341853180699,
-0.145223553959774));
#40974=CARTESIAN_POINT('Ctrl Pts',(0.56426305151595,-0.190104706888137,
-0.134848081709056));
#40975=CARTESIAN_POINT('Ctrl Pts',(0.587571414135597,0.0964199572183358,
-0.124472609458338));
#40976=CARTESIAN_POINT('Ctrl Pts',(0.47389064191257,0.360530207813974,-0.114097137207619));
#40977=CARTESIAN_POINT('Ctrl Pts',(0.324463350889184,0.480464515819192,
-0.10718015570714));
#40978=CARTESIAN_POINT('Ctrl Pts',(0.240021988234213,0.519480035866726,
-0.103721664956901));
#40979=CARTESIAN_POINT('',(0.244165145742818,0.528447079373888,-0.12));
#40980=CARTESIAN_POINT('Ctrl Pts',(0.532924512516476,0.208474282488455,
-0.12));
#40981=CARTESIAN_POINT('Ctrl Pts',(0.505551419169843,0.278448344774197,
-0.12));
#40982=CARTESIAN_POINT('Ctrl Pts',(0.465349567486002,0.342411647567949,
-0.12));
#40983=CARTESIAN_POINT('Ctrl Pts',(0.351955928646152,0.46510551701231,-0.12));
#40984=CARTESIAN_POINT('Ctrl Pts',(0.287038107347888,0.504862695897963,
-0.12));
#40985=CARTESIAN_POINT('Ctrl Pts',(0.244165145742818,0.528447079373888,
-0.12));
#40986=CARTESIAN_POINT('Ctrl Pts',(-0.353365195478197,-0.462556454142148,
-0.72625));
#40987=CARTESIAN_POINT('Ctrl Pts',(-0.320950876724053,-0.487335965390693,
-0.724759130180554));
#40988=CARTESIAN_POINT('Ctrl Pts',(-0.204788602894649,-0.558391458988749,
-0.719809769610869));
#40989=CARTESIAN_POINT('Ctrl Pts',(0.0275428991067036,-0.605077845001504,
-0.711401918290945));
#40990=CARTESIAN_POINT('Ctrl Pts',(0.307852790782245,-0.521644157320061,
-0.701026446040225));
#40991=CARTESIAN_POINT('Ctrl Pts',(0.516379630382223,-0.316594299265632,
-0.690650973789508));
#40992=CARTESIAN_POINT('Ctrl Pts',(0.604531894922356,-0.037741447613471,
-0.680275501538789));
#40993=CARTESIAN_POINT('Ctrl Pts',(0.551748054568745,0.249911729814406,
-0.669900029288071));
#40994=CARTESIAN_POINT('Ctrl Pts',(0.370338916630071,0.479302937024635,
-0.659524557037353));
#40995=CARTESIAN_POINT('Ctrl Pts',(0.102593005245228,0.596956344106599,
-0.649149084786633));
#40996=CARTESIAN_POINT('Ctrl Pts',(-0.189069595066604,0.575443129800777,
-0.638773612535917));
#40997=CARTESIAN_POINT('Ctrl Pts',(-0.436655282749753,0.419778941359981,
-0.628398140285197));
#40998=CARTESIAN_POINT('Ctrl Pts',(-0.582444898128172,0.166253064936486,
-0.618022668034479));
#40999=CARTESIAN_POINT('Ctrl Pts',(-0.59245118529686,-0.126030790814807,
-0.607647195783762));
#41000=CARTESIAN_POINT('Ctrl Pts',(-0.464341322608817,-0.388933533934673,
-0.597271723533042));
#41001=CARTESIAN_POINT('Ctrl Pts',(-0.227981169867371,-0.561165524309829,
-0.586896251282325));
#41002=CARTESIAN_POINT('Ctrl Pts',(0.0615274613730338,-0.602574918002375,
-0.576520779031606));
#41003=CARTESIAN_POINT('Ctrl Pts',(0.336692401993215,-0.503508078945706,
-0.566145306780887));
#41004=CARTESIAN_POINT('Ctrl Pts',(0.533365395804019,-0.287060123544462,
-0.55576983453017));
#41005=CARTESIAN_POINT('Ctrl Pts',(0.605696737111815,-0.00369082231710978,
-0.545394362279451));
#41006=CARTESIAN_POINT('Ctrl Pts',(0.536824069047151,0.280538907457441,
-0.535018890028733));
#41007=CARTESIAN_POINT('Ctrl Pts',(0.342803440542624,0.499367560825895,
-0.524643417778015));
#41008=CARTESIAN_POINT('Ctrl Pts',(0.0688662178762295,0.601780361666548,
-0.514267945527296));
#41009=CARTESIAN_POINT('Ctrl Pts',(-0.221125550821607,0.563902163890325,
-0.503892473276578));
#41010=CARTESIAN_POINT('Ctrl Pts',(-0.459567075698392,0.394563382218786,
-0.493517001025859));
#41011=CARTESIAN_POINT('Ctrl Pts',(-0.590871299173015,0.133241387995481,
-0.483141528775141));
#41012=CARTESIAN_POINT('Ctrl Pts',(-0.584427716440101,-0.159142715555849,
-0.472766056524423));
#41013=CARTESIAN_POINT('Ctrl Pts',(-0.441738497928306,-0.414426421825547,
-0.462390584273705));
#41014=CARTESIAN_POINT('Ctrl Pts',(-0.196068293388198,-0.573096313010961,
-0.452015112022986));
#41015=CARTESIAN_POINT('Ctrl Pts',(0.0953106421677161,-0.598162219760071,
-0.441639639772268));
#41016=CARTESIAN_POINT('Ctrl Pts',(0.364470133516224,-0.483780612916302,
-0.43126416752155));
#41017=CARTESIAN_POINT('Ctrl Pts',(0.548661948506927,-0.256616885491388,
-0.420888695270832));
#41018=CARTESIAN_POINT('Ctrl Pts',(0.60494607893493,0.0303710592533639,
-0.410513223020113));
#41019=CARTESIAN_POINT('Ctrl Pts',(0.520201197869222,0.310278702773021,
-0.400137750769395));
#41020=CARTESIAN_POINT('Ctrl Pts',(0.314183589749731,0.517852132939369,
-0.389762278518676));
#41021=CARTESIAN_POINT('Ctrl Pts',(0.0349214353255983,0.604700465533282,
-0.379386806267958));
#41022=CARTESIAN_POINT('Ctrl Pts',(-0.252481833942362,0.550577045637576,
-0.36901133401724));
#41023=CARTESIAN_POINT('Ctrl Pts',(-0.481024876325774,0.368099481148946,
-0.358635861766521));
#41024=CARTESIAN_POINT('Ctrl Pts',(-0.597428233573601,0.0998081428603092,
-0.348260389515803));
#41025=CARTESIAN_POINT('Ctrl Pts',(-0.574555188931242,-0.191751126529284,
-0.337884917265085));
#41026=CARTESIAN_POINT('Ctrl Pts',(-0.417738057072088,-0.43860811139261,
-0.327509445014367));
#41027=CARTESIAN_POINT('Ctrl Pts',(-0.163535079971663,-0.583213886268098,
-0.317133972763648));
#41028=CARTESIAN_POINT('Ctrl Pts',(0.128792271407237,-0.591857001983,-0.30675850051293));
#41029=CARTESIAN_POINT('Ctrl Pts',(0.3910947206114,-0.462522516893444,-0.296383028262211));
#41030=CARTESIAN_POINT('Ctrl Pts',(0.562222594861329,-0.225361740621548,
-0.286007556011493));
#41031=CARTESIAN_POINT('Ctrl Pts',(0.602281436660628,0.0643368521302563,
-0.275632083760774));
#41032=CARTESIAN_POINT('Ctrl Pts',(0.501932467413927,0.339036806050298,
-0.265256611510057));
#41033=CARTESIAN_POINT('Ctrl Pts',(0.284569694815385,0.534698285003551,
-0.254881139259338));
#41034=CARTESIAN_POINT('Ctrl Pts',(0.00086616792234151,0.605707347412463,
-0.24450566700862));
#41035=CARTESIAN_POINT('Ctrl Pts',(-0.283039297466054,0.535509992112656,
-0.234130194757901));
#41036=CARTESIAN_POINT('Ctrl Pts',(-0.500960755684866,0.340470892555017,
-0.223754722507184));
#41037=CARTESIAN_POINT('Ctrl Pts',(-0.602094991516589,0.066059236182406,
-0.213379250256465));
#41038=CARTESIAN_POINT('Ctrl Pts',(-0.562864788572229,-0.223753096954469,
-0.203003778005747));
#41039=CARTESIAN_POINT('Ctrl Pts',(-0.392416023107415,-0.46140161814604,
-0.192628305755028));
#41040=CARTESIAN_POINT('Ctrl Pts',(-0.130484291345699,-0.591487175311845,
-0.18225283350431));
#41041=CARTESIAN_POINT('Ctrl Pts',(0.161866082666176,-0.583677346042729,
-0.171877361253592));
#41042=CARTESIAN_POINT('Ctrl Pts',(0.416482587440825,-0.439804754427654,
-0.161501889002873));
#41043=CARTESIAN_POINT('Ctrl Pts',(0.574003120398452,-0.193386213509922,
-0.151126416752155));
#41044=CARTESIAN_POINT('Ctrl Pts',(0.597713822063416,0.0980843175241036,
-0.140750944501437));
#41045=CARTESIAN_POINT('Ctrl Pts',(0.482070740684944,0.366753526971408,
-0.130375472250718));
#41046=CARTESIAN_POINT('Ctrl Pts',(0.33006409929725,0.48875809000787,-0.12345849075024));
#41047=CARTESIAN_POINT('Ctrl Pts',(0.244165145742818,0.528447079373888,
-0.12));
#41048=CARTESIAN_POINT('Ctrl Pts',(-0.389567997368774,-0.509945078027931,
-0.75727273924394));
#41049=CARTESIAN_POINT('Ctrl Pts',(-0.304713279680621,-0.574769083320626,
-0.753732335137029));
#41050=CARTESIAN_POINT('Ctrl Pts',(-0.102102228503407,-0.661170845788992,
-0.746651526923207));
#41051=CARTESIAN_POINT('Ctrl Pts',(0.226918975852293,-0.629330849807756,
-0.736030314602476));
#41052=CARTESIAN_POINT('Ctrl Pts',(0.500480649699589,-0.443915736617459,
-0.725409102281742));
#41053=CARTESIAN_POINT('Ctrl Pts',(0.651928335250053,-0.150143800232939,
-0.714787889961012));
#41054=CARTESIAN_POINT('Ctrl Pts',(0.644242880084047,0.180267689012914,
-0.704166677640277));
#41055=CARTESIAN_POINT('Ctrl Pts',(0.479327999531238,0.466684539337087,
-0.693545465319547));
#41056=CARTESIAN_POINT('Ctrl Pts',(0.197419996334723,0.639197400194773,
-0.682924252998813));
#41057=CARTESIAN_POINT('Ctrl Pts',(-0.13266944809657,0.655703641639384,
-0.672303040678082));
#41058=CARTESIAN_POINT('Ctrl Pts',(-0.430379781004106,0.512173537080057,
-0.661681828357348));
#41059=CARTESIAN_POINT('Ctrl Pts',(-0.623047772943777,0.243638675874784,
-0.651060616036617));
#41060=CARTESIAN_POINT('Ctrl Pts',(-0.663650324809919,-0.0843605725621005,
-0.640439403715884));
#41061=CARTESIAN_POINT('Ctrl Pts',(-0.542277215052327,-0.391770096128179,
-0.629818191395152));
#41062=CARTESIAN_POINT('Ctrl Pts',(-0.288551910996521,-0.603561275664924,
-0.61919697907442));
#41063=CARTESIAN_POINT('Ctrl Pts',(0.0355995897879127,-0.668042721572721,
-0.608575766753687));
#41064=CARTESIAN_POINT('Ctrl Pts',(0.351062366380979,-0.569476623116135,
-0.597954554432955));
#41065=CARTESIAN_POINT('Ctrl Pts',(0.580842221167565,-0.331919757495687,
-0.587333342112222));
#41066=CARTESIAN_POINT('Ctrl Pts',(0.668857333165026,-0.0133520513920273,
-0.57671212979149));
#41067=CARTESIAN_POINT('Ctrl Pts',(0.593626077081373,0.308474457943291,
-0.566090917470758));
#41068=CARTESIAN_POINT('Ctrl Pts',(0.373509957515226,0.555012361719922,
-0.555469705150025));
#41069=CARTESIAN_POINT('Ctrl Pts',(0.0622321783665508,0.666089758367902,
-0.544848492829294));
#41070=CARTESIAN_POINT('Ctrl Pts',(-0.264234456403739,0.614596259540999,
-0.53422728050856));
#41071=CARTESIAN_POINT('Ctrl Pts',(-0.526210034624122,0.413099757483066,
-0.523606068187829));
#41072=CARTESIAN_POINT('Ctrl Pts',(-0.659754819010986,0.110779009702939,
-0.512984855867096));
#41073=CARTESIAN_POINT('Ctrl Pts',(-0.632274861107494,-0.218579299549813,
-0.502363643546364));
#41074=CARTESIAN_POINT('Ctrl Pts',(-0.450477126973457,-0.494589494695984,
-0.491742431225631));
#41075=CARTESIAN_POINT('Ctrl Pts',(-0.158732544136138,-0.64988644363315,
-0.481121218904899));
#41076=CARTESIAN_POINT('Ctrl Pts',(0.171753501841992,-0.646567200522882,
-0.470500006584167));
#41077=CARTESIAN_POINT('Ctrl Pts',(0.460320091431361,-0.48544188489642,
-0.459878794263435));
#41078=CARTESIAN_POINT('Ctrl Pts',(0.636537484106821,-0.205835957776284,
-0.449257581942702));
#41079=CARTESIAN_POINT('Ctrl Pts',(0.657396732580188,0.124007847251966,
-0.43863636962197));
#41080=CARTESIAN_POINT('Ctrl Pts',(0.517806771181053,0.423585360825624,
-0.428015157301238));
#41081=CARTESIAN_POINT('Ctrl Pts',(0.251836979788509,0.619779433184232,
-0.417393944980505));
#41082=CARTESIAN_POINT('Ctrl Pts',(-0.0755980462515238,0.664705457770534,
-0.406772732659774));
#41083=CARTESIAN_POINT('Ctrl Pts',(-0.384582042358491,0.547398449834714,
-0.39615152033904));
#41084=CARTESIAN_POINT('Ctrl Pts',(-0.599702041634294,0.296489243396025,
-0.385530308018309));
#41085=CARTESIAN_POINT('Ctrl Pts',(-0.668454232892285,-0.0267833662666586,
-0.374909095697576));
#41086=CARTESIAN_POINT('Ctrl Pts',(-0.574058437290037,-0.343519025346637,
-0.364287883376844));
#41087=CARTESIAN_POINT('Ctrl Pts',(-0.339553605322675,-0.576412837542728,
-0.353666671056111));
#41088=CARTESIAN_POINT('Ctrl Pts',(-0.0221747569089046,-0.668622980721422,
-0.343045458735379));
#41089=CARTESIAN_POINT('Ctrl Pts',(0.300616230262104,-0.597643951136341,
-0.332424246414647));
#41090=CARTESIAN_POINT('Ctrl Pts',(0.550036550302552,-0.380799426675277,
-0.321803034093914));
#41091=CARTESIAN_POINT('Ctrl Pts',(0.665210797783139,-0.0710141190690022,
-0.311181821773182));
#41092=CARTESIAN_POINT('Ctrl Pts',(0.618028674331743,0.256103430490016,
-0.30056060945245));
#41093=CARTESIAN_POINT('Ctrl Pts',(0.420005809134218,0.520714443433612,
-0.289939397131717));
#41094=CARTESIAN_POINT('Ctrl Pts',(0.119473149966588,0.658235957542453,
-0.279318184810985));
#41095=CARTESIAN_POINT('Ctrl Pts',(-0.210219017943201,0.635103434988625,
-0.268696972490253));
#41096=CARTESIAN_POINT('Ctrl Pts',(-0.488603565549287,0.456962771519233,
-0.25807576016952));
#41097=CARTESIAN_POINT('Ctrl Pts',(-0.647735797590754,0.167292327094403,
-0.247454547848788));
#41098=CARTESIAN_POINT('Ctrl Pts',(-0.648776820735564,-0.163208751908622,
-0.236833335528056));
#41099=CARTESIAN_POINT('Ctrl Pts',(-0.491472315475939,-0.453875858438117,
-0.226212123207324));
#41100=CARTESIAN_POINT('Ctrl Pts',(-0.214215682544731,-0.633766620558494,
-0.215590910886591));
#41101=CARTESIAN_POINT('Ctrl Pts',(0.115324674990204,-0.658975468022751,
-0.204969698565859));
#41102=CARTESIAN_POINT('Ctrl Pts',(0.416716775328578,-0.523349883470236,
-0.194348486245126));
#41103=CARTESIAN_POINT('Ctrl Pts',(0.616404307509721,-0.259991384615625,
-0.183727273924394));
#41104=CARTESIAN_POINT('Ctrl Pts',(0.66564263859121,0.0668221963899351,
-0.173106061603661));
#41105=CARTESIAN_POINT('Ctrl Pts',(0.552428954539379,0.377327397940862,
-0.162484849282929));
#41106=CARTESIAN_POINT('Ctrl Pts',(0.304365909285143,0.595737740289611,
-0.151863636962197));
#41107=CARTESIAN_POINT('Ctrl Pts',(-0.0179442774568819,0.668750733104762,
-0.141242424641465));
#41108=CARTESIAN_POINT('Ctrl Pts',(-0.33595438712131,0.578538159640864,
-0.130621212320732));
#41109=CARTESIAN_POINT('Ctrl Pts',(-0.493165134596604,0.424261513660227,
-0.123540404106911));
#41110=CARTESIAN_POINT('Ctrl Pts',(-0.548572772984126,0.332979158385831,
-0.12));
#41111=CARTESIAN_POINT('Ctrl Pts',(-0.377508796945348,-0.494159567045475,
-0.746931826162627));
#41112=CARTESIAN_POINT('Ctrl Pts',(-0.295280783848913,-0.556976924776374,
-0.743391422055716));
#41113=CARTESIAN_POINT('Ctrl Pts',(-0.0989416217658999,-0.640704093393138,
-0.736310613841894));
#41114=CARTESIAN_POINT('Ctrl Pts',(0.219894627270879,-0.609849714545784,
-0.725689401521162));
#41115=CARTESIAN_POINT('Ctrl Pts',(0.484988113085858,-0.430174184757091,
-0.71506818920043));
#41116=CARTESIAN_POINT('Ctrl Pts',(0.631747687687648,-0.145496051466169,
-0.704446976879697));
#41117=CARTESIAN_POINT('Ctrl Pts',(0.62430013821415,0.174687445752796,-0.693825764558965));
#41118=CARTESIAN_POINT('Ctrl Pts',(0.464490249885608,0.452238171995848,
-0.683204552238233));
#41119=CARTESIAN_POINT('Ctrl Pts',(0.191308797983031,0.619410842748719,
-0.672583339917501));
#41120=CARTESIAN_POINT('Ctrl Pts',(-0.128562623420344,0.635406128275076,
-0.661962127596767));
#41121=CARTESIAN_POINT('Ctrl Pts',(-0.41705723892577,0.49631904344367,-0.651340915276036));
#41122=CARTESIAN_POINT('Ctrl Pts',(-0.603761132310959,0.236096763697407,
-0.640719702955302));
#41123=CARTESIAN_POINT('Ctrl Pts',(-0.643106819357702,-0.0817491643888608,
-0.630098490634572));
#41124=CARTESIAN_POINT('Ctrl Pts',(-0.52549085255453,-0.379642729042011,
-0.619477278313838));
#41125=CARTESIAN_POINT('Ctrl Pts',(-0.279619695437819,-0.584877845711175,
-0.608856065993107));
#41126=CARTESIAN_POINT('Ctrl Pts',(0.0344975932400858,-0.647363248091151,
-0.598234853672374));
#41127=CARTESIAN_POINT('Ctrl Pts',(0.340195119928743,-0.551848294349405,
-0.587613641351642));
#41128=CARTESIAN_POINT('Ctrl Pts',(0.562862066722751,-0.321645076548663,
-0.576992429030909));
#41129=CARTESIAN_POINT('Ctrl Pts',(0.648152643124277,-0.0129387344232621,
-0.566371216710177));
#41130=CARTESIAN_POINT('Ctrl Pts',(0.575250194338317,0.298925533650301,
-0.555750004389445));
#41131=CARTESIAN_POINT('Ctrl Pts',(0.361947838788215,0.537831778733985,
-0.545128792068713));
#41132=CARTESIAN_POINT('Ctrl Pts',(0.0603057616260149,0.645470739479278,
-0.53450757974798));
#41133=CARTESIAN_POINT('Ctrl Pts',(-0.256054995333863,0.595571238175405,
-0.523886367427248));
#41134=CARTESIAN_POINT('Ctrl Pts',(-0.509921036772116,0.400312123991598,
-0.513265155106515));
#41135=CARTESIAN_POINT('Ctrl Pts',(-0.63933190017137,0.107349810462397,
-0.502643942785783));
#41136=CARTESIAN_POINT('Ctrl Pts',(-0.612702593045721,-0.211813108282854,
-0.49202273046505));
#41137=CARTESIAN_POINT('Ctrl Pts',(-0.436532465201871,-0.47927932064641,
-0.481401518144319));
#41138=CARTESIAN_POINT('Ctrl Pts',(-0.153818928088652,-0.629769003470783,
-0.470780305823586));
#41139=CARTESIAN_POINT('Ctrl Pts',(0.16643681793539,-0.626552508579544,
-0.460159093502854));
#41140=CARTESIAN_POINT('Ctrl Pts',(0.446070737585578,-0.47041487799793,
-0.449537881182121));
#41141=CARTESIAN_POINT('Ctrl Pts',(0.61683326520354,-0.199464240679558,
-0.438916668861389));
#41142=CARTESIAN_POINT('Ctrl Pts',(0.637046809050958,0.120169145166092,
-0.428295456540657));
#41143=CARTESIAN_POINT('Ctrl Pts',(0.501777899003527,0.410473142170276,
-0.417674244219924));
#41144=CARTESIAN_POINT('Ctrl Pts',(0.244041286523631,0.600593965041143,
-0.407053031899192));
#41145=CARTESIAN_POINT('Ctrl Pts',(-0.0732578848483181,0.644129290344205,
-0.396431819578459));
#41146=CARTESIAN_POINT('Ctrl Pts',(-0.372677183747475,0.530453557896425,
-0.385810607257728));
#41147=CARTESIAN_POINT('Ctrl Pts',(-0.581138075489099,0.287311325205486,
-0.375189394936995));
#41148=CARTESIAN_POINT('Ctrl Pts',(-0.64776202094782,-0.0259542787029844,
-0.364568182616263));
#41149=CARTESIAN_POINT('Ctrl Pts',(-0.556288277018155,-0.332885285399068,
-0.35394697029553));
#41150=CARTESIAN_POINT('Ctrl Pts',(-0.329042616204627,-0.558569796067267,
-0.343325757974798));
#41151=CARTESIAN_POINT('Ctrl Pts',(-0.0214883303037647,-0.647925545134599,
-0.332704545654066));
#41152=CARTESIAN_POINT('Ctrl Pts',(0.291310559889408,-0.579143693832662,
-0.322083333333334));
#41153=CARTESIAN_POINT('Ctrl Pts',(0.533009995130902,-0.369011660127668,
-0.311462121012601));
#41154=CARTESIAN_POINT('Ctrl Pts',(0.644618987397083,-0.0688158545797981,
-0.300840908691869));
#41155=CARTESIAN_POINT('Ctrl Pts',(0.598897401481997,0.248175667895896,
-0.290219696371136));
#41156=CARTESIAN_POINT('Ctrl Pts',(0.407004396632262,0.504595563342971,
-0.279598484050404));
#41157=CARTESIAN_POINT('Ctrl Pts',(0.115774820867698,0.637860055539404,
-0.268977271729672));
#41158=CARTESIAN_POINT('Ctrl Pts',(-0.203711621834396,0.615443607528816,
-0.258356059408939));
#41159=CARTESIAN_POINT('Ctrl Pts',(-0.473478687827409,0.442817344571911,
-0.247734847088207));
#41160=CARTESIAN_POINT('Ctrl Pts',(-0.62768493135602,0.162113740261402,
-0.237113634767475));
#41161=CARTESIAN_POINT('Ctrl Pts',(-0.628693729300522,-0.158156573435501,
-0.226492422446742));
#41162=CARTESIAN_POINT('Ctrl Pts',(-0.476258634693842,-0.439825987860379,
-0.215871210126011));
#41163=CARTESIAN_POINT('Ctrl Pts',(-0.207584568420635,-0.614148174611669,
-0.205249997805277));
#41164=CARTESIAN_POINT('Ctrl Pts',(0.111754763244715,-0.638576674239172,
-0.194628785484546));
#41165=CARTESIAN_POINT('Ctrl Pts',(0.403817175907084,-0.507149422500723,
-0.184007573163813));
#41166=CARTESIAN_POINT('Ctrl Pts',(0.59732331744809,-0.251943269173339,
-0.173386360843081));
#41167=CARTESIAN_POINT('Ctrl Pts',(0.645037460436522,0.0647536941914932,
-0.162765148522348));
#41168=CARTESIAN_POINT('Ctrl Pts',(0.535328341738816,0.365647109139544,
-0.152143936201616));
#41169=CARTESIAN_POINT('Ctrl Pts',(0.294944166413762,0.577296490344866,
-0.141522723880883));
#41170=CARTESIAN_POINT('Ctrl Pts',(-0.0173888066795909,0.648049342902555,
-0.130901511560152));
#41171=CARTESIAN_POINT('Ctrl Pts',(-0.325554812939681,0.560629328148464,
-0.120280299239419));
#41172=CARTESIAN_POINT('Ctrl Pts',(-0.477899052063863,0.411128364480287,
-0.113199491025598));
#41173=CARTESIAN_POINT('Ctrl Pts',(-0.531591529501778,0.322671683349587,
-0.109659086918687));
#41174=CARTESIAN_POINT('Ctrl Pts',(-0.365449596521923,-0.478374056063018,
-0.736590913081313));
#41175=CARTESIAN_POINT('Ctrl Pts',(-0.285848288017205,-0.539184766232121,
-0.733050508974403));
#41176=CARTESIAN_POINT('Ctrl Pts',(-0.0957810150283928,-0.620237340997284,
-0.72596970076058));
#41177=CARTESIAN_POINT('Ctrl Pts',(0.212870278689466,-0.590368579283812,
-0.715348488439849));
#41178=CARTESIAN_POINT('Ctrl Pts',(0.469495576472127,-0.416432632896724,
-0.704727276119116));
#41179=CARTESIAN_POINT('Ctrl Pts',(0.611567040125244,-0.140848302699399,
-0.694106063798384));
#41180=CARTESIAN_POINT('Ctrl Pts',(0.604357396344252,0.169107202492678,
-0.683484851477651));
#41181=CARTESIAN_POINT('Ctrl Pts',(0.44965250023998,0.437791804654609,-0.67286363915692));
#41182=CARTESIAN_POINT('Ctrl Pts',(0.185197599631338,0.599624285302665,
-0.662242426836187));
#41183=CARTESIAN_POINT('Ctrl Pts',(-0.124455798744119,0.615108614910768,
-0.651621214515455));
#41184=CARTESIAN_POINT('Ctrl Pts',(-0.403734696847433,0.480464549807283,
-0.641000002194722));
#41185=CARTESIAN_POINT('Ctrl Pts',(-0.584474491678141,0.22855485152003,
-0.630378789873991));
#41186=CARTESIAN_POINT('Ctrl Pts',(-0.622563313905486,-0.0791377562156208,
-0.619757577553257));
#41187=CARTESIAN_POINT('Ctrl Pts',(-0.508704490056733,-0.367515361955843,
-0.609136365232526));
#41188=CARTESIAN_POINT('Ctrl Pts',(-0.270687479879118,-0.566194415757424,
-0.598515152911792));
#41189=CARTESIAN_POINT('Ctrl Pts',(0.033395596692259,-0.62668377460958,
-0.587893940591062));
#41190=CARTESIAN_POINT('Ctrl Pts',(0.329327873476507,-0.534219965582675,
-0.577272728270328));
#41191=CARTESIAN_POINT('Ctrl Pts',(0.544881912277937,-0.311370395601639,
-0.566651515949596));
#41192=CARTESIAN_POINT('Ctrl Pts',(0.627447953083531,-0.0125254174544974,
-0.556030303628864));
#41193=CARTESIAN_POINT('Ctrl Pts',(0.556874311595259,0.289376609357312,
-0.545409091308131));
#41194=CARTESIAN_POINT('Ctrl Pts',(0.350385720061206,0.520651195748048,
-0.5347878789874));
#41195=CARTESIAN_POINT('Ctrl Pts',(0.0583793448854777,0.624851720590656,
-0.524166666666666));
#41196=CARTESIAN_POINT('Ctrl Pts',(-0.247875534263986,0.576546216809811,
-0.513545454345935));
#41197=CARTESIAN_POINT('Ctrl Pts',(-0.49363203892011,0.387524490500131,
-0.502924242025201));
#41198=CARTESIAN_POINT('Ctrl Pts',(-0.618908981331752,0.103920611221856,
-0.49230302970447));
#41199=CARTESIAN_POINT('Ctrl Pts',(-0.593130324983951,-0.205046917015896,
-0.481681817383737));
#41200=CARTESIAN_POINT('Ctrl Pts',(-0.422587803430283,-0.463969146596836,
-0.471060605063006));
#41201=CARTESIAN_POINT('Ctrl Pts',(-0.148905312041167,-0.609651563308416,
-0.460439392742272));
#41202=CARTESIAN_POINT('Ctrl Pts',(0.161120134028788,-0.606537816636207,
-0.449818180421541));
#41203=CARTESIAN_POINT('Ctrl Pts',(0.431821383739795,-0.455387871099441,
-0.439196968100808));
#41204=CARTESIAN_POINT('Ctrl Pts',(0.597129046300259,-0.193092523582832,
-0.428575755780076));
#41205=CARTESIAN_POINT('Ctrl Pts',(0.616696885521728,0.116330443080218,
-0.417954543459344));
#41206=CARTESIAN_POINT('Ctrl Pts',(0.485749026826,0.397360923514928,-0.407333331138611));
#41207=CARTESIAN_POINT('Ctrl Pts',(0.236245593258753,0.581408496898052,
-0.396712118817879));
#41208=CARTESIAN_POINT('Ctrl Pts',(-0.0709177234451122,0.623553122917875,
-0.386090906497146));
#41209=CARTESIAN_POINT('Ctrl Pts',(-0.36077232513646,0.513508665958136,
-0.375469694176414));
#41210=CARTESIAN_POINT('Ctrl Pts',(-0.562574109343903,0.278133407014948,
-0.364848481855682));
#41211=CARTESIAN_POINT('Ctrl Pts',(-0.627069809003355,-0.0251251911393111,
-0.35422726953495));
#41212=CARTESIAN_POINT('Ctrl Pts',(-0.538518116746273,-0.322251545451498,
-0.343606057214217));
#41213=CARTESIAN_POINT('Ctrl Pts',(-0.31853162708658,-0.540726754591806,
-0.332984844893485));
#41214=CARTESIAN_POINT('Ctrl Pts',(-0.0208019036986243,-0.627228109547775,
-0.322363632572752));
#41215=CARTESIAN_POINT('Ctrl Pts',(0.28200488951671,-0.560643436528983,
-0.311742420252021));
#41216=CARTESIAN_POINT('Ctrl Pts',(0.515983439959253,-0.357223893580059,
-0.301121207931288));
#41217=CARTESIAN_POINT('Ctrl Pts',(0.624027177011026,-0.0666175900905945,
-0.290499995610556));
#41218=CARTESIAN_POINT('Ctrl Pts',(0.579766128632252,0.240247905301778,
-0.279878783289823));
#41219=CARTESIAN_POINT('Ctrl Pts',(0.394002984130306,0.488476683252329,
-0.269257570969091));
#41220=CARTESIAN_POINT('Ctrl Pts',(0.112076491768808,0.617484153536356,
-0.258636358648359));
#41221=CARTESIAN_POINT('Ctrl Pts',(-0.197204225725589,0.595783780069004,
-0.248015146327626));
#41222=CARTESIAN_POINT('Ctrl Pts',(-0.458353810105532,0.428671917624589,
-0.237393934006894));
#41223=CARTESIAN_POINT('Ctrl Pts',(-0.607634065121286,0.1569351534284,-0.226772721686162));
#41224=CARTESIAN_POINT('Ctrl Pts',(-0.608610637865481,-0.15310439496238,
-0.216151509365429));
#41225=CARTESIAN_POINT('Ctrl Pts',(-0.461044953911745,-0.425776117282641,
-0.205530297044697));
#41226=CARTESIAN_POINT('Ctrl Pts',(-0.200953454296539,-0.594529728664845,
-0.194909084723964));
#41227=CARTESIAN_POINT('Ctrl Pts',(0.108184851499226,-0.618177880455594,
-0.184287872403232));
#41228=CARTESIAN_POINT('Ctrl Pts',(0.390917576485589,-0.490948961531211,
-0.1736666600825));
#41229=CARTESIAN_POINT('Ctrl Pts',(0.57824232738646,-0.243895153731054,
-0.163045447761767));
#41230=CARTESIAN_POINT('Ctrl Pts',(0.624432282281831,0.0626851919930514,
-0.152424235441035));
#41231=CARTESIAN_POINT('Ctrl Pts',(0.518227728938254,0.353966820338225,
-0.141803023120303));
#41232=CARTESIAN_POINT('Ctrl Pts',(0.28552242354238,0.558855240400121,-0.13118181079957));
#41233=CARTESIAN_POINT('Ctrl Pts',(-0.0168333359022998,0.627347952700348,
-0.120560598478838));
#41234=CARTESIAN_POINT('Ctrl Pts',(-0.315155238758052,0.542720496656064,
-0.109939386158106));
#41235=CARTESIAN_POINT('Ctrl Pts',(-0.462632969531122,0.397995215300347,
-0.102858577944284));
#41236=CARTESIAN_POINT('Ctrl Pts',(-0.514610286019429,0.312364208313342,
-0.0993181738373735));
#41237=CARTESIAN_POINT('Ctrl Pts',(-0.353390396098497,-0.462588545080562,
-0.72625));
#41238=CARTESIAN_POINT('Ctrl Pts',(-0.276415792185496,-0.521392607687868,
-0.722709595893089));
#41239=CARTESIAN_POINT('Ctrl Pts',(-0.0926204082908857,-0.59977058860143,
-0.715628787679267));
#41240=CARTESIAN_POINT('Ctrl Pts',(0.205845930108053,-0.57088744402184,
-0.705007575358536));
#41241=CARTESIAN_POINT('Ctrl Pts',(0.454003039858395,-0.402691081036356,
-0.694386363037803));
#41242=CARTESIAN_POINT('Ctrl Pts',(0.59138639256284,-0.136200553932629,
-0.683765150717071));
#41243=CARTESIAN_POINT('Ctrl Pts',(0.584414654474354,0.16352695923256,-0.673143938396339));
#41244=CARTESIAN_POINT('Ctrl Pts',(0.434814750594351,0.42334543731337,-0.662522726075606));
#41245=CARTESIAN_POINT('Ctrl Pts',(0.179086401279645,0.57983772785661,-0.651901513754874));
#41246=CARTESIAN_POINT('Ctrl Pts',(-0.120348974067893,0.59481110154646,
-0.641280301434141));
#41247=CARTESIAN_POINT('Ctrl Pts',(-0.390412154769097,0.464610056170896,
-0.630659089113409));
#41248=CARTESIAN_POINT('Ctrl Pts',(-0.565187851045323,0.221012939342653,
-0.620037876792677));
#41249=CARTESIAN_POINT('Ctrl Pts',(-0.602019808453269,-0.0765263480423816,
-0.609416664471945));
#41250=CARTESIAN_POINT('Ctrl Pts',(-0.491918127558936,-0.355387994869674,
-0.598795452151212));
#41251=CARTESIAN_POINT('Ctrl Pts',(-0.261755264320416,-0.547510985803676,
-0.58817423983048));
#41252=CARTESIAN_POINT('Ctrl Pts',(0.0322936001444312,-0.606004301128008,
-0.577553027509747));
#41253=CARTESIAN_POINT('Ctrl Pts',(0.318460627024272,-0.516591636815947,
-0.566931815189015));
#41254=CARTESIAN_POINT('Ctrl Pts',(0.526901757833122,-0.301095714654614,
-0.556310602868283));
#41255=CARTESIAN_POINT('Ctrl Pts',(0.606743263042784,-0.012112100485733,
-0.545689390547551));
#41256=CARTESIAN_POINT('Ctrl Pts',(0.538498428852201,0.279827685064323,
-0.535068178226818));
#41257=CARTESIAN_POINT('Ctrl Pts',(0.338823601334196,0.50347061276211,-0.524446965906085));
#41258=CARTESIAN_POINT('Ctrl Pts',(0.056452928144941,0.604232701702033,
-0.513825753585354));
#41259=CARTESIAN_POINT('Ctrl Pts',(-0.239696073194109,0.557521195444216,
-0.503204541264621));
#41260=CARTESIAN_POINT('Ctrl Pts',(-0.477343041068104,0.374736857008664,
-0.492583328943889));
#41261=CARTESIAN_POINT('Ctrl Pts',(-0.598486062492136,0.100491411981314,
-0.481962116623157));
#41262=CARTESIAN_POINT('Ctrl Pts',(-0.57355805692218,-0.198280725748937,
-0.471340904302424));
#41263=CARTESIAN_POINT('Ctrl Pts',(-0.408643141658697,-0.448658972547262,
-0.460719691981692));
#41264=CARTESIAN_POINT('Ctrl Pts',(-0.143991695993682,-0.589534123146049,
-0.45009847966096));
#41265=CARTESIAN_POINT('Ctrl Pts',(0.155803450122185,-0.58652312469287,
-0.439477267340227));
#41266=CARTESIAN_POINT('Ctrl Pts',(0.417572029894014,-0.440360864200951,
-0.428856055019495));
#41267=CARTESIAN_POINT('Ctrl Pts',(0.577424827396976,-0.186720806486106,
-0.418234842698762));
#41268=CARTESIAN_POINT('Ctrl Pts',(0.596346961992498,0.112491740994345,
-0.407613630378031));
#41269=CARTESIAN_POINT('Ctrl Pts',(0.469720154648472,0.38424870485958,-0.396992418057298));
#41270=CARTESIAN_POINT('Ctrl Pts',(0.228449899993875,0.562223028754963,
-0.386371205736566));
#41271=CARTESIAN_POINT('Ctrl Pts',(-0.0685775620419064,0.602976955491545,
-0.375749993415833));
#41272=CARTESIAN_POINT('Ctrl Pts',(-0.348867466525445,0.496563774019848,
-0.365128781095101));
#41273=CARTESIAN_POINT('Ctrl Pts',(-0.544010143198707,0.268955488824409,
-0.354507568774369));
#41274=CARTESIAN_POINT('Ctrl Pts',(-0.606377597058891,-0.0242961035756373,
-0.343886356453636));
#41275=CARTESIAN_POINT('Ctrl Pts',(-0.520747956474391,-0.311617805503928,
-0.333265144132904));
#41276=CARTESIAN_POINT('Ctrl Pts',(-0.308020637968532,-0.522883713116344,
-0.322643931812172));
#41277=CARTESIAN_POINT('Ctrl Pts',(-0.0201154770934842,-0.606530673960952,
-0.312022719491439));
#41278=CARTESIAN_POINT('Ctrl Pts',(0.272699219144013,-0.542143179225304,
-0.301401507170707));
#41279=CARTESIAN_POINT('Ctrl Pts',(0.498956884787604,-0.34543612703245,
-0.290780294849974));
#41280=CARTESIAN_POINT('Ctrl Pts',(0.603435366624969,-0.0644193256013902,
-0.280159082529242));
#41281=CARTESIAN_POINT('Ctrl Pts',(0.560634855782508,0.232320142707658,
-0.26953787020851));
#41282=CARTESIAN_POINT('Ctrl Pts',(0.381001571628349,0.472357803161688,
-0.258916657887777));
#41283=CARTESIAN_POINT('Ctrl Pts',(0.108378162669919,0.597108251533307,
-0.248295445567045));
#41284=CARTESIAN_POINT('Ctrl Pts',(-0.190696829616783,0.576123952609194,
-0.237674233246313));
#41285=CARTESIAN_POINT('Ctrl Pts',(-0.443228932383655,0.414526490677267,
-0.227053020925581));
#41286=CARTESIAN_POINT('Ctrl Pts',(-0.587583198886552,0.151756566595399,
-0.216431808604848));
#41287=CARTESIAN_POINT('Ctrl Pts',(-0.588527546430439,-0.148052216489259,
-0.205810596284116));
#41288=CARTESIAN_POINT('Ctrl Pts',(-0.445831273129648,-0.411726246704904,
-0.195189383963384));
#41289=CARTESIAN_POINT('Ctrl Pts',(-0.194322340172443,-0.574911282718019,
-0.184568171642651));
#41290=CARTESIAN_POINT('Ctrl Pts',(0.104614939753737,-0.597779086672016,
-0.173946959321919));
#41291=CARTESIAN_POINT('Ctrl Pts',(0.378017977064095,-0.474748500561697,
-0.163325747001186));
#41292=CARTESIAN_POINT('Ctrl Pts',(0.55916133732483,-0.235847038288769,
-0.152704534680454));
#41293=CARTESIAN_POINT('Ctrl Pts',(0.603827104127141,0.0606166897946097,
-0.142083322359722));
#41294=CARTESIAN_POINT('Ctrl Pts',(0.501127116137692,0.342286531536906,
-0.13146211003899));
#41295=CARTESIAN_POINT('Ctrl Pts',(0.276100680670998,0.540413990455376,
-0.120840897718257));
#41296=CARTESIAN_POINT('Ctrl Pts',(-0.0162778651250086,0.606646562498142,
-0.110219685397525));
#41297=CARTESIAN_POINT('Ctrl Pts',(-0.304755664576424,0.524811665163664,
-0.0995984730767926));
#41298=CARTESIAN_POINT('Ctrl Pts',(-0.447366886998382,0.384862066120406,
-0.092517664862971));
#41299=CARTESIAN_POINT('Ctrl Pts',(-0.49762904253708,0.302056733277098,
-0.0889772607560603));
#41300=CARTESIAN_POINT('',(-0.548572772984126,0.332979158385831,-0.12));
#41301=CARTESIAN_POINT('Ctrl Pts',(0.244188262120089,0.528481699529947,
-0.12));
#41302=CARTESIAN_POINT('Ctrl Pts',(0.218445435093476,0.542622181160769,
-0.12));
#41303=CARTESIAN_POINT('Ctrl Pts',(0.191707940815084,0.554740156615991,
-0.12));
#41304=CARTESIAN_POINT('Ctrl Pts',(0.164242712890297,0.56481938294899,-0.12));
#41305=CARTESIAN_POINT('Ctrl Pts',(0.135399059471504,0.575404465726192,
-0.12));
#41306=CARTESIAN_POINT('Ctrl Pts',(0.105751683718357,0.583741941385187,
-0.12));
#41307=CARTESIAN_POINT('Ctrl Pts',(0.0755747762095856,0.589763858499476,
-0.12));
#41308=CARTESIAN_POINT('Ctrl Pts',(0.0608331404233321,0.592705608206865,
-0.12));
#41309=CARTESIAN_POINT('Ctrl Pts',(0.0459647294330388,0.595093961778282,
-0.12));
#41310=CARTESIAN_POINT('Ctrl Pts',(0.0310000226320474,0.596915993675276,
-0.12));
#41311=CARTESIAN_POINT('Ctrl Pts',(0.0251721580287127,0.597625566895777,
-0.12));
#41312=CARTESIAN_POINT('Ctrl Pts',(0.0193318047130446,0.598248864029065,
-0.12));
#41313=CARTESIAN_POINT('Ctrl Pts',(0.0134897283974255,0.598784612282793,
-0.12));
#41314=CARTESIAN_POINT('Ctrl Pts',(0.00362475613712504,0.599689280653419,
-0.12));
#41315=CARTESIAN_POINT('Ctrl Pts',(-0.00625226620039982,0.600345248614976,
-0.12));
#41316=CARTESIAN_POINT('Ctrl Pts',(-0.0161321161443918,0.600751319652268,
-0.12));
#41317=CARTESIAN_POINT('Ctrl Pts',(-0.0462082784714154,0.60198747794446,
-0.12));
#41318=CARTESIAN_POINT('Ctrl Pts',(-0.0763096986544558,0.600911821118615,
-0.12));
#41319=CARTESIAN_POINT('Ctrl Pts',(-0.10619074537105,0.597625116816541,
-0.12));
#41320=CARTESIAN_POINT('Ctrl Pts',(-0.126342040119356,0.595408616579124,
-0.12));
#41321=CARTESIAN_POINT('Ctrl Pts',(-0.146393540566889,0.592185434384527,
-0.12));
#41322=CARTESIAN_POINT('Ctrl Pts',(-0.166271047885959,0.587973203665797,
-0.12));
#41323=CARTESIAN_POINT('Ctrl Pts',(-0.177982331622319,0.585491472515194,
-0.12));
#41324=CARTESIAN_POINT('Ctrl Pts',(-0.189633215255517,0.582666219304311,
-0.12));
#41325=CARTESIAN_POINT('Ctrl Pts',(-0.201208227469216,0.579499366783346,
-0.12));
#41326=CARTESIAN_POINT('Ctrl Pts',(-0.207704857075218,0.577721928672205,
-0.12));
#41327=CARTESIAN_POINT('Ctrl Pts',(-0.214175648256732,0.575837255539024,
-0.12));
#41328=CARTESIAN_POINT('Ctrl Pts',(-0.220606829957527,0.573849512326344,
-0.12));
#41329=CARTESIAN_POINT('Ctrl Pts',(-0.25015216366532,0.56471767011191,-0.12));
#41330=CARTESIAN_POINT('Ctrl Pts',(-0.278927093165708,0.553397185268195,
-0.12));
#41331=CARTESIAN_POINT('Ctrl Pts',(-0.30667747358036,0.539970478586301,
-0.12));
#41332=CARTESIAN_POINT('Ctrl Pts',(-0.30845905545231,0.53910848041305,-0.12));
#41333=CARTESIAN_POINT('Ctrl Pts',(-0.310236412641107,0.538237783373462,
-0.12));
#41334=CARTESIAN_POINT('Ctrl Pts',(-0.312009476799349,0.537358402041895,
-0.12));
#41335=CARTESIAN_POINT('Ctrl Pts',(-0.335549088486224,0.525683531184262,
-0.12));
#41336=CARTESIAN_POINT('Ctrl Pts',(-0.358332961769366,0.512480115942743,
-0.12));
#41337=CARTESIAN_POINT('Ctrl Pts',(-0.380250615167753,0.497858544366281,
-0.12));
#41338=CARTESIAN_POINT('Ctrl Pts',(-0.386498225486996,0.493690676583894,
-0.12));
#41339=CARTESIAN_POINT('Ctrl Pts',(-0.392677270141369,0.489406051262931,
-0.12));
#41340=CARTESIAN_POINT('Ctrl Pts',(-0.398778867975252,0.485011296272449,
-0.12));
#41341=CARTESIAN_POINT('Ctrl Pts',(-0.424115404323213,0.46676232729937,
-0.12));
#41342=CARTESIAN_POINT('Ctrl Pts',(-0.44802782182311,0.446685130200945,
-0.12));
#41343=CARTESIAN_POINT('Ctrl Pts',(-0.470348776553481,0.424986510597564,
-0.12));
#41344=CARTESIAN_POINT('Ctrl Pts',(-0.492791511018824,0.403169506625034,
-0.12));
#41345=CARTESIAN_POINT('Ctrl Pts',(-0.513626430101255,0.379712592792303,
-0.12));
#41346=CARTESIAN_POINT('Ctrl Pts',(-0.53265652290141,0.354781937742959,
-0.12));
#41347=CARTESIAN_POINT('Ctrl Pts',(-0.538112251162996,0.347634580094158,
-0.12));
#41348=CARTESIAN_POINT('Ctrl Pts',(-0.54341941474828,0.340365857942668,
-0.12));
#41349=CARTESIAN_POINT('Ctrl Pts',(-0.548572772984126,0.332979158385831,
-0.12));
#41350=CARTESIAN_POINT('Ctrl Pts',(0.462926795561193,-0.444481916564912,
-0.72625));
#41351=CARTESIAN_POINT('Ctrl Pts',(0.468784532279406,-0.438389058883916,
-0.725969700760581));
#41352=CARTESIAN_POINT('Ctrl Pts',(0.546966429469725,-0.353744549862236,
-0.722148997414251));
#41353=CARTESIAN_POINT('Ctrl Pts',(0.651928335250053,-0.150143800232939,
-0.714787889961012));
#41354=CARTESIAN_POINT('Ctrl Pts',(0.644242880084047,0.180267689012914,
-0.704166677640277));
#41355=CARTESIAN_POINT('Ctrl Pts',(0.479327999531238,0.466684539337087,
-0.693545465319547));
#41356=CARTESIAN_POINT('Ctrl Pts',(0.197419996334723,0.639197400194773,
-0.682924252998813));
#41357=CARTESIAN_POINT('Ctrl Pts',(-0.13266944809657,0.655703641639384,
-0.672303040678082));
#41358=CARTESIAN_POINT('Ctrl Pts',(-0.430379781004106,0.512173537080057,
-0.661681828357348));
#41359=CARTESIAN_POINT('Ctrl Pts',(-0.623047772943777,0.243638675874784,
-0.651060616036617));
#41360=CARTESIAN_POINT('Ctrl Pts',(-0.663650324809919,-0.0843605725621005,
-0.640439403715884));
#41361=CARTESIAN_POINT('Ctrl Pts',(-0.542277215052327,-0.391770096128179,
-0.629818191395152));
#41362=CARTESIAN_POINT('Ctrl Pts',(-0.288551910996521,-0.603561275664924,
-0.61919697907442));
#41363=CARTESIAN_POINT('Ctrl Pts',(0.0355995897879127,-0.668042721572721,
-0.608575766753687));
#41364=CARTESIAN_POINT('Ctrl Pts',(0.351062366380979,-0.569476623116135,
-0.597954554432955));
#41365=CARTESIAN_POINT('Ctrl Pts',(0.580842221167565,-0.331919757495687,
-0.587333342112222));
#41366=CARTESIAN_POINT('Ctrl Pts',(0.668857333165026,-0.0133520513920273,
-0.57671212979149));
#41367=CARTESIAN_POINT('Ctrl Pts',(0.593626077081373,0.308474457943291,
-0.566090917470758));
#41368=CARTESIAN_POINT('Ctrl Pts',(0.373509957515226,0.555012361719922,
-0.555469705150025));
#41369=CARTESIAN_POINT('Ctrl Pts',(0.0622321783665508,0.666089758367902,
-0.544848492829294));
#41370=CARTESIAN_POINT('Ctrl Pts',(-0.264234456403739,0.614596259540999,
-0.53422728050856));
#41371=CARTESIAN_POINT('Ctrl Pts',(-0.526210034624122,0.413099757483066,
-0.523606068187829));
#41372=CARTESIAN_POINT('Ctrl Pts',(-0.659754819010986,0.110779009702939,
-0.512984855867096));
#41373=CARTESIAN_POINT('Ctrl Pts',(-0.632274861107494,-0.218579299549813,
-0.502363643546364));
#41374=CARTESIAN_POINT('Ctrl Pts',(-0.450477126973457,-0.494589494695984,
-0.491742431225631));
#41375=CARTESIAN_POINT('Ctrl Pts',(-0.158732544136138,-0.64988644363315,
-0.481121218904899));
#41376=CARTESIAN_POINT('Ctrl Pts',(0.171753501841992,-0.646567200522882,
-0.470500006584167));
#41377=CARTESIAN_POINT('Ctrl Pts',(0.460320091431361,-0.48544188489642,
-0.459878794263435));
#41378=CARTESIAN_POINT('Ctrl Pts',(0.636537484106821,-0.205835957776284,
-0.449257581942702));
#41379=CARTESIAN_POINT('Ctrl Pts',(0.657396732580188,0.124007847251966,
-0.43863636962197));
#41380=CARTESIAN_POINT('Ctrl Pts',(0.517806771181053,0.423585360825624,
-0.428015157301238));
#41381=CARTESIAN_POINT('Ctrl Pts',(0.251836979788509,0.619779433184232,
-0.417393944980505));
#41382=CARTESIAN_POINT('Ctrl Pts',(-0.0755980462515238,0.664705457770534,
-0.406772732659774));
#41383=CARTESIAN_POINT('Ctrl Pts',(-0.384582042358491,0.547398449834714,
-0.39615152033904));
#41384=CARTESIAN_POINT('Ctrl Pts',(-0.599702041634294,0.296489243396025,
-0.385530308018309));
#41385=CARTESIAN_POINT('Ctrl Pts',(-0.668454232892285,-0.0267833662666586,
-0.374909095697576));
#41386=CARTESIAN_POINT('Ctrl Pts',(-0.574058437290037,-0.343519025346637,
-0.364287883376844));
#41387=CARTESIAN_POINT('Ctrl Pts',(-0.339553605322675,-0.576412837542728,
-0.353666671056111));
#41388=CARTESIAN_POINT('Ctrl Pts',(-0.0221747569089046,-0.668622980721422,
-0.343045458735379));
#41389=CARTESIAN_POINT('Ctrl Pts',(0.300616230262104,-0.597643951136341,
-0.332424246414647));
#41390=CARTESIAN_POINT('Ctrl Pts',(0.550036550302552,-0.380799426675277,
-0.321803034093914));
#41391=CARTESIAN_POINT('Ctrl Pts',(0.665210797783139,-0.0710141190690022,
-0.311181821773182));
#41392=CARTESIAN_POINT('Ctrl Pts',(0.618028674331743,0.256103430490016,
-0.30056060945245));
#41393=CARTESIAN_POINT('Ctrl Pts',(0.420005809134218,0.520714443433612,
-0.289939397131717));
#41394=CARTESIAN_POINT('Ctrl Pts',(0.119473149966588,0.658235957542453,
-0.279318184810985));
#41395=CARTESIAN_POINT('Ctrl Pts',(-0.210219017943201,0.635103434988625,
-0.268696972490253));
#41396=CARTESIAN_POINT('Ctrl Pts',(-0.488603565549287,0.456962771519233,
-0.25807576016952));
#41397=CARTESIAN_POINT('Ctrl Pts',(-0.647735797590754,0.167292327094403,
-0.247454547848788));
#41398=CARTESIAN_POINT('Ctrl Pts',(-0.648776820735564,-0.163208751908622,
-0.236833335528056));
#41399=CARTESIAN_POINT('Ctrl Pts',(-0.491472315475939,-0.453875858438117,
-0.226212123207324));
#41400=CARTESIAN_POINT('Ctrl Pts',(-0.214215682544731,-0.633766620558494,
-0.215590910886591));
#41401=CARTESIAN_POINT('Ctrl Pts',(0.115324674990204,-0.658975468022751,
-0.204969698565859));
#41402=CARTESIAN_POINT('Ctrl Pts',(0.416716775328578,-0.523349883470236,
-0.194348486245126));
#41403=CARTESIAN_POINT('Ctrl Pts',(0.616404307509721,-0.259991384615625,
-0.183727273924394));
#41404=CARTESIAN_POINT('Ctrl Pts',(0.66564263859121,0.0668221963899351,
-0.173106061603661));
#41405=CARTESIAN_POINT('Ctrl Pts',(0.552428954539379,0.377327397940862,
-0.162484849282929));
#41406=CARTESIAN_POINT('Ctrl Pts',(0.304365909285143,0.595737740289611,
-0.151863636962197));
#41407=CARTESIAN_POINT('Ctrl Pts',(-0.0179442774568819,0.668750733104762,
-0.141242424641465));
#41408=CARTESIAN_POINT('Ctrl Pts',(-0.33595438712131,0.578538159640864,
-0.130621212320732));
#41409=CARTESIAN_POINT('Ctrl Pts',(-0.493165134596604,0.424261513660227,
-0.123540404106911));
#41410=CARTESIAN_POINT('Ctrl Pts',(-0.548572772984126,0.332979158385831,
-0.12));
#41411=CARTESIAN_POINT('Ctrl Pts',(0.462889160393653,-0.444455658495748,
-0.72625));
#41412=CARTESIAN_POINT('Ctrl Pts',(0.535135327429651,-0.369213129884151,
-0.722791509249761));
#41413=CARTESIAN_POINT('Ctrl Pts',(0.642190315853192,-0.182914675178815,
-0.715874527749283));
#41414=CARTESIAN_POINT('Ctrl Pts',(0.653014131807411,0.139347482177261,
-0.705499055498563));
#41415=CARTESIAN_POINT('Ctrl Pts',(0.511617065765403,0.429054145801984,
-0.695123583247846));
#41416=CARTESIAN_POINT('Ctrl Pts',(0.25094192882907,0.618770941114435,-0.684748110997127));
#41417=CARTESIAN_POINT('Ctrl Pts',(-0.0682312037537184,0.664218747915985,
-0.674372638746408));
#41418=CARTESIAN_POINT('Ctrl Pts',(-0.37149945364269,0.554828066014907,
-0.663997166495691));
#41419=CARTESIAN_POINT('Ctrl Pts',(-0.588160489258797,0.316087911596656,
-0.653621694244971));
#41420=CARTESIAN_POINT('Ctrl Pts',(-0.667706091050652,0.00366142581770804,
-0.643246221994255));
#41421=CARTESIAN_POINT('Ctrl Pts',(-0.591591447850655,-0.309619723170008,
-0.632870749743535));
#41422=CARTESIAN_POINT('Ctrl Pts',(-0.377561216430721,-0.550719737673313,
-0.622495277492817));
#41423=CARTESIAN_POINT('Ctrl Pts',(-0.0755113770637089,-0.663432617182758,
-0.612119805242099));
#41424=CARTESIAN_POINT('Ctrl Pts',(0.244142145282362,-0.621481580233081,
-0.601744332991381));
#41425=CARTESIAN_POINT('Ctrl Pts',(0.506879657041181,-0.434646736395633,
-0.591368860740661));
#41426=CARTESIAN_POINT('Ctrl Pts',(0.651450040389794,-0.146484149712398,
-0.580993388489944));
#41427=CARTESIAN_POINT('Ctrl Pts',(0.644150106010189,0.175827768496734,
-0.570617916239225));
#41428=CARTESIAN_POINT('Ctrl Pts',(0.486681657639716,0.457149568902442,
-0.560242443988508));
#41429=CARTESIAN_POINT('Ctrl Pts',(0.215754778891774,0.631897648543906,
-0.549866971737789));
#41430=CARTESIAN_POINT('Ctrl Pts',(-0.105470274367959,0.659333591630754,
-0.53949149948707));
#41431=CARTESIAN_POINT('Ctrl Pts',(-0.402107402880485,0.53306134717955,
-0.529116027236352));
#41432=CARTESIAN_POINT('Ctrl Pts',(-0.605002607191347,0.28251833358982,
-0.518740554985634));
#41433=CARTESIAN_POINT('Ctrl Pts',(-0.666855621715713,-0.0338872136604341,
-0.508365082734916));
#41434=CARTESIAN_POINT('Ctrl Pts',(-0.573246864690785,-0.342392750484064,
-0.497989610484197));
#41435=CARTESIAN_POINT('Ctrl Pts',(-0.345999025618036,-0.571077435861077,
-0.487614138233478));
#41436=CARTESIAN_POINT('Ctrl Pts',(-0.0380896164391166,-0.666628790695116,
-0.477238665982761));
#41437=CARTESIAN_POINT('Ctrl Pts',(0.278699494821865,-0.60677125431137,
-0.466863193732042));
#41438=CARTESIAN_POINT('Ctrl Pts',(0.530516345532464,-0.405459209528553,
-0.456487721481324));
#41439=CARTESIAN_POINT('Ctrl Pts',(0.658655734075261,-0.109623845215152,
-0.446112249230605));
#41440=CARTESIAN_POINT('Ctrl Pts',(0.633244962817189,0.211767751408133,
-0.435736776979887));
#41441=CARTESIAN_POINT('Ctrl Pts',(0.46020795800052,0.483790656030648,-0.425361304729169));
#41442=CARTESIAN_POINT('Ctrl Pts',(0.179884245065169,0.643029098756216,
-0.414985832478451));
#41443=CARTESIAN_POINT('Ctrl Pts',(-0.142375267023613,0.652360365756174,
-0.404610360227732));
#41444=CARTESIAN_POINT('Ctrl Pts',(-0.431443319792535,0.509609090653018,
-0.394234887977014));
#41445=CARTESIAN_POINT('Ctrl Pts',(-0.619930466222754,0.248054390242977,
-0.383859415726295));
#41446=CARTESIAN_POINT('Ctrl Pts',(-0.663895342170731,-0.0713283822377002,
-0.373483943475577));
#41447=CARTESIAN_POINT('Ctrl Pts',(-0.553088566396638,-0.374082612792774,
-0.363108471224859));
#41448=CARTESIAN_POINT('Ctrl Pts',(-0.313342143756286,-0.58962824254807,
-0.35273299897414));
#41449=CARTESIAN_POINT('Ctrl Pts',(-0.000547338252603717,-0.667715855659524,
-0.342357526723423));
#41450=CARTESIAN_POINT('Ctrl Pts',(0.312375066371514,-0.590141153768528,
-0.331982054472704));
#41451=CARTESIAN_POINT('Ctrl Pts',(0.55247453951602,-0.374988862034699,
-0.321606582221986));
#41452=CARTESIAN_POINT('Ctrl Pts',(0.663777511885435,-0.0724166986121209,
-0.311231109971267));
#41453=CARTESIAN_POINT('Ctrl Pts',(0.620336301707957,0.247037722001034,
-0.300855637720549));
#41454=CARTESIAN_POINT('Ctrl Pts',(0.432278210394921,0.508901083360732,
-0.29048016546983));
#41455=CARTESIAN_POINT('Ctrl Pts',(0.14344457678541,0.652126073885111,-0.280104693219112));
#41456=CARTESIAN_POINT('Ctrl Pts',(-0.178829799152076,0.643323143657881,
-0.269729220968394));
#41457=CARTESIAN_POINT('Ctrl Pts',(-0.459414198332819,0.48454448466337,
-0.259353748717676));
#41458=CARTESIAN_POINT('Ctrl Pts',(-0.632896929856003,0.212805632960395,
-0.248978276466957));
#41459=CARTESIAN_POINT('Ctrl Pts',(-0.658834575522026,-0.108543881809492,
-0.238602804216239));
#41460=CARTESIAN_POINT('Ctrl Pts',(-0.531180344891156,-0.404588906018681,
-0.228227331965521));
#41461=CARTESIAN_POINT('Ctrl Pts',(-0.279693903529316,-0.606313554142205,
-0.217851859714802));
#41462=CARTESIAN_POINT('Ctrl Pts',(0.0369967156354772,-0.666690291400585,
-0.207476387464084));
#41463=CARTESIAN_POINT('Ctrl Pts',(0.345062229691949,-0.571644007915702,
-0.197100915213366));
#41464=CARTESIAN_POINT('Ctrl Pts',(0.572684938105708,-0.343331897341362,
-0.186725442962647));
#41465=CARTESIAN_POINT('Ctrl Pts',(0.666798823765209,-0.0349808177150975,
-0.176349970711929));
#41466=CARTESIAN_POINT('Ctrl Pts',(0.605465652234757,0.281526856371821,
-0.165974498461211));
#41467=CARTESIAN_POINT('Ctrl Pts',(0.402979412578655,0.532399882876135,
-0.155599026210492));
#41468=CARTESIAN_POINT('Ctrl Pts',(0.106553789103513,0.659162816942658,
-0.145223553959774));
#41469=CARTESIAN_POINT('Ctrl Pts',(-0.214723962090429,0.632244495520886,
-0.134848081709056));
#41470=CARTESIAN_POINT('Ctrl Pts',(-0.485920592934187,0.457958900439567,
-0.124472609458337));
#41471=CARTESIAN_POINT('Ctrl Pts',(-0.643884510525116,0.176858466795417,
-0.114097137207619));
#41472=CARTESIAN_POINT('Ctrl Pts',(-0.649036352703418,-0.0379468946230774,
-0.10718015570714));
#41473=CARTESIAN_POINT('Ctrl Pts',(-0.626319218357157,-0.139754942292966,
-0.103721664956901));
#41474=CARTESIAN_POINT('Ctrl Pts',(0.464718942461958,-0.44621257367903,
-0.727570523102925));
#41475=CARTESIAN_POINT('Ctrl Pts',(0.537250663424813,-0.37067264798198,
-0.724112032352686));
#41476=CARTESIAN_POINT('Ctrl Pts',(0.644728882109174,-0.183637706565169,
-0.717195050852207));
#41477=CARTESIAN_POINT('Ctrl Pts',(0.655595457840136,0.139898306064466,
-0.706819578601489));
#41478=CARTESIAN_POINT('Ctrl Pts',(0.513639468333482,0.430750181907022,
-0.69644410635077));
#41479=CARTESIAN_POINT('Ctrl Pts',(0.251933888482677,0.621216911245235,
-0.686068634100052));
#41480=CARTESIAN_POINT('Ctrl Pts',(-0.0685009174702088,0.666844374933673,
-0.675693161849334));
#41481=CARTESIAN_POINT('Ctrl Pts',(-0.372967974187952,0.557021274844762,
-0.665317689598615));
#41482=CARTESIAN_POINT('Ctrl Pts',(-0.590485459981355,0.31733739269549,
-0.654942217347898));
#41483=CARTESIAN_POINT('Ctrl Pts',(-0.670345502226871,0.00367589910057958,
-0.644566745097178));
#41484=CARTESIAN_POINT('Ctrl Pts',(-0.593929981190927,-0.310843635416322,
-0.634191272846461));
#41485=CARTESIAN_POINT('Ctrl Pts',(-0.379053698347304,-0.552896707157342,
-0.623815800595742));
#41486=CARTESIAN_POINT('Ctrl Pts',(-0.0758098699991723,-0.666055135361883,
-0.613440328345024));
#41487=CARTESIAN_POINT('Ctrl Pts',(0.245107227789762,-0.623938267950393,
-0.603064856094305));
#41488=CARTESIAN_POINT('Ctrl Pts',(0.508883328693909,-0.436364874671762,
-0.592689383843588));
#41489=CARTESIAN_POINT('Ctrl Pts',(0.654025192020124,-0.147063194728269,
-0.582313911592868));
#41490=CARTESIAN_POINT('Ctrl Pts',(0.646696401343553,0.176522807468057,
-0.571938439342151));
#41491=CARTESIAN_POINT('Ctrl Pts',(0.48860548753781,0.458956659830723,-0.561562967091432));
#41492=CARTESIAN_POINT('Ctrl Pts',(0.216607647472342,0.634395510483487,
-0.551187494840714));
#41493=CARTESIAN_POINT('Ctrl Pts',(-0.105887193444585,0.661939906573517,
-0.540812022589996));
#41494=CARTESIAN_POINT('Ctrl Pts',(-0.403696914693697,0.535168513828335,
-0.530436550339277));
#41495=CARTESIAN_POINT('Ctrl Pts',(-0.607394154286282,0.283635115388603,
-0.520061078088559));
#41496=CARTESIAN_POINT('Ctrl Pts',(-0.669491670892799,-0.0340211682358486,
-0.509685605837841));
#41497=CARTESIAN_POINT('Ctrl Pts',(-0.575512882816362,-0.343746213060933,
-0.499310133587123));
#41498=CARTESIAN_POINT('Ctrl Pts',(-0.347366743632334,-0.573334878335637,
-0.488934661336404));
#41499=CARTESIAN_POINT('Ctrl Pts',(-0.0382401829167803,-0.669263943219774,
-0.478559189085686));
#41500=CARTESIAN_POINT('Ctrl Pts',(0.279801180929114,-0.609169792785862,
-0.468183716834967));
#41501=CARTESIAN_POINT('Ctrl Pts',(0.532613451908327,-0.40706197087722,
-0.457808244584249));
#41502=CARTESIAN_POINT('Ctrl Pts',(0.661259369478884,-0.110057183163517,
-0.44743277233353));
#41503=CARTESIAN_POINT('Ctrl Pts',(0.635748150626934,0.212604859454699,
-0.437057300082813));
#41504=CARTESIAN_POINT('Ctrl Pts',(0.462027138598958,0.485703057934735,
-0.426681827832093));
#41505=CARTESIAN_POINT('Ctrl Pts',(0.180595319097893,0.645570962799093,
-0.416306355581376));
#41506=CARTESIAN_POINT('Ctrl Pts',(-0.142938069815186,0.654939115862385,
-0.405930883330657));
#41507=CARTESIAN_POINT('Ctrl Pts',(-0.433148795117433,0.51162355162525,
-0.395555411079939));
#41508=CARTESIAN_POINT('Ctrl Pts',(-0.622381022448319,0.249034937680809,
-0.385179938829221));
#41509=CARTESIAN_POINT('Ctrl Pts',(-0.666519689500831,-0.0716103400066377,
-0.374804466578503));
#41510=CARTESIAN_POINT('Ctrl Pts',(-0.555274899709033,-0.375561343917636,
-0.364428994327784));
#41511=CARTESIAN_POINT('Ctrl Pts',(-0.314580770639381,-0.591959015496446,
-0.354053522077066));
#41512=CARTESIAN_POINT('Ctrl Pts',(-0.000549501855194795,-0.670355305301288,
-0.343678049826347));
#41513=CARTESIAN_POINT('Ctrl Pts',(0.313609870442805,-0.592473954231052,
-0.333302577575629));
#41514=CARTESIAN_POINT('Ctrl Pts',(0.554658445608785,-0.37647117552053,
-0.32292710532491));
#41515=CARTESIAN_POINT('Ctrl Pts',(0.666401393437919,-0.0727029584449918,
-0.312551633074193));
#41516=CARTESIAN_POINT('Ctrl Pts',(0.622788462182255,0.248014250596821,
-0.302176160823474));
#41517=CARTESIAN_POINT('Ctrl Pts',(0.43398698600347,0.510912745612938,-0.291800688572756));
#41518=CARTESIAN_POINT('Ctrl Pts',(0.144011606508548,0.654703897846908,
-0.281425216322037));
#41519=CARTESIAN_POINT('Ctrl Pts',(-0.179536705009153,0.645866170045693,
-0.271049744071319));
#41520=CARTESIAN_POINT('Ctrl Pts',(-0.461230241236544,0.486459866418583,
-0.260674271820601));
#41521=CARTESIAN_POINT('Ctrl Pts',(-0.635398741907202,0.213646843700976,
-0.250298799569883));
#41522=CARTESIAN_POINT('Ctrl Pts',(-0.661438917878502,-0.108972950706181,
-0.239923327319164));
#41523=CARTESIAN_POINT('Ctrl Pts',(-0.533280076023624,-0.406188227111467,
-0.229547855068446));
#41524=CARTESIAN_POINT('Ctrl Pts',(-0.280799520491592,-0.608710283322796,
-0.219172382817727));
#41525=CARTESIAN_POINT('Ctrl Pts',(0.0371429619347367,-0.669325687087322,
-0.208796910567009));
#41526=CARTESIAN_POINT('Ctrl Pts',(0.346426244580695,-0.573903689918445,
-0.198421438316291));
#41527=CARTESIAN_POINT('Ctrl Pts',(0.574948734991407,-0.344689072530265,
-0.188045966065572));
#41528=CARTESIAN_POINT('Ctrl Pts',(0.669434648363557,-0.035119094842057,
-0.177670493814854));
#41529=CARTESIAN_POINT('Ctrl Pts',(0.607859029842677,0.282639718083408,
-0.167295021564136));
#41530=CARTESIAN_POINT('Ctrl Pts',(0.404572371171796,0.534504436426277,
-0.156919549313418));
#41531=CARTESIAN_POINT('Ctrl Pts',(0.106974991728399,0.661768453560443,
-0.146544077062699));
#41532=CARTESIAN_POINT('Ctrl Pts',(-0.215572756826861,0.634743735027689,
-0.136168604811981));
#41533=CARTESIAN_POINT('Ctrl Pts',(-0.487841412514633,0.459769177540265,
-0.125793132561263));
#41534=CARTESIAN_POINT('Ctrl Pts',(-0.646429759948626,0.17755760797843,
-0.115417660310544));
#41535=CARTESIAN_POINT('Ctrl Pts',(-0.651601956932064,-0.038096942589642,
-0.108500678810065));
#41536=CARTESIAN_POINT('Ctrl Pts',(-0.628795032813062,-0.14030738790899,
-0.105042188059826));
#41537=CARTESIAN_POINT('Ctrl Pts',(0.468463827977225,-0.449808327695529,
-0.732058124057058));
#41538=CARTESIAN_POINT('Ctrl Pts',(0.541579446992128,-0.373660287164295,
-0.728599633306819));
#41539=CARTESIAN_POINT('Ctrl Pts',(0.649924613974643,-0.185117110828464,
-0.721682651806341));
#41540=CARTESIAN_POINT('Ctrl Pts',(0.660878274402623,0.141025458328198,
-0.711307179555621));
#41541=CARTESIAN_POINT('Ctrl Pts',(0.5177785939746,0.434221379345974,-0.700931707304904));
#41542=CARTESIAN_POINT('Ctrl Pts',(0.253964003373025,0.626222802832036,
-0.690556235054185));
#41543=CARTESIAN_POINT('Ctrl Pts',(-0.0690528976258993,0.672218015378987,
-0.680180762803467));
#41544=CARTESIAN_POINT('Ctrl Pts',(-0.375973463283883,0.561509895041683,
-0.66980529055275));
#41545=CARTESIAN_POINT('Ctrl Pts',(-0.595243750791249,0.319894591382352,
-0.659429818302029));
#41546=CARTESIAN_POINT('Ctrl Pts',(-0.67574733472572,0.00370551753535922,
-0.649054346051313));
#41547=CARTESIAN_POINT('Ctrl Pts',(-0.59871603254323,-0.313348498179755,
-0.638678873800593));
#41548=CARTESIAN_POINT('Ctrl Pts',(-0.382108218840265,-0.557352102985363,
-0.628303401549875));
#41549=CARTESIAN_POINT('Ctrl Pts',(-0.0764207666551862,-0.67142239206951,
-0.617927929299157));
#41550=CARTESIAN_POINT('Ctrl Pts',(0.247082369683177,-0.628966135823776,
-0.607552457048439));
#41551=CARTESIAN_POINT('Ctrl Pts',(0.512984051831413,-0.439881223811224,
-0.59717698479772));
#41552=CARTESIAN_POINT('Ctrl Pts',(0.659295508445708,-0.148248270804131,
-0.586801512547002));
#41553=CARTESIAN_POINT('Ctrl Pts',(0.651907660399777,0.177945277253391,
-0.576426040296284));
#41554=CARTESIAN_POINT('Ctrl Pts',(0.49254280611635,0.462655059926965,-0.566050568045565));
#41555=CARTESIAN_POINT('Ctrl Pts',(0.218353132001307,0.639507645534371,
-0.555675095794847));
#41556=CARTESIAN_POINT('Ctrl Pts',(-0.106740461831666,0.667274002001449,
-0.545299623544128));
#41557=CARTESIAN_POINT('Ctrl Pts',(-0.40695001644199,0.539481050203778,
-0.534924151293411));
#41558=CARTESIAN_POINT('Ctrl Pts',(-0.612288704911572,0.28592072584588,
-0.524548679042691));
#41559=CARTESIAN_POINT('Ctrl Pts',(-0.674886620535706,-0.0342953202487183,
-0.514173206791974));
#41560=CARTESIAN_POINT('Ctrl Pts',(-0.580150525309795,-0.346516215422834,
-0.503797734541255));
#41561=CARTESIAN_POINT('Ctrl Pts',(-0.350165921233864,-0.577954969864389,
-0.493422262290537));
#41562=CARTESIAN_POINT('Ctrl Pts',(-0.0385483329210009,-0.674657057770278,
-0.483046790039819));
#41563=CARTESIAN_POINT('Ctrl Pts',(0.282055896479539,-0.614078651998191,
-0.4726713177891));
#41564=CARTESIAN_POINT('Ctrl Pts',(0.536905398884327,-0.410342189183201,
-0.462295845538382));
#41565=CARTESIAN_POINT('Ctrl Pts',(0.666587980953165,-0.11094405448224,
-0.451920373287663));
#41566=CARTESIAN_POINT('Ctrl Pts',(0.64087118562128,0.214318088402166,-0.441544901036946));
#41567=CARTESIAN_POINT('Ctrl Pts',(0.46575028147723,0.489616987940208,-0.431169428786226));
#41568=CARTESIAN_POINT('Ctrl Pts',(0.182050606287704,0.65077315273939,-0.420793956535509));
#41569=CARTESIAN_POINT('Ctrl Pts',(-0.144089904441783,0.660216796979385,
-0.41041848428479));
#41570=CARTESIAN_POINT('Ctrl Pts',(-0.436639228291258,0.515746356160854,
-0.400043012034072));
#41571=CARTESIAN_POINT('Ctrl Pts',(-0.627396341414921,0.251041730306632,
-0.389667539783354));
#41572=CARTESIAN_POINT('Ctrl Pts',(-0.671890690093387,-0.072187395995648,
-0.379292067532636));
#41573=CARTESIAN_POINT('Ctrl Pts',(-0.559749458919139,-0.378587721431273,
-0.368916595281917));
#41574=CARTESIAN_POINT('Ctrl Pts',(-0.317115749773712,-0.596729185490112,
-0.358541123031199));
#41575=CARTESIAN_POINT('Ctrl Pts',(-0.00055392989362848,-0.675757214350081,
-0.348165650780481));
#41576=CARTESIAN_POINT('Ctrl Pts',(0.316137025794007,-0.597248273744105,
-0.337790178529762));
#41577=CARTESIAN_POINT('Ctrl Pts',(0.559128037260631,-0.3795048847092,-0.327414706279044));
#41578=CARTESIAN_POINT('Ctrl Pts',(0.671771440768122,-0.0732888190575194,
-0.317039234028325));
#41579=CARTESIAN_POINT('Ctrl Pts',(0.627807064410998,0.250012818244892,
-0.306663761777607));
#41580=CARTESIAN_POINT('Ctrl Pts',(0.437484173552585,0.515029822272535,
-0.296288289526889));
#41581=CARTESIAN_POINT('Ctrl Pts',(0.145172091990569,0.65997968351971,-0.28591281727617));
#41582=CARTESIAN_POINT('Ctrl Pts',(-0.180983461590688,0.651070738832306,
-0.275537345025452));
#41583=CARTESIAN_POINT('Ctrl Pts',(-0.464946962499182,0.490379895027805,
-0.265161872774734));
#41584=CARTESIAN_POINT('Ctrl Pts',(-0.640518961260343,0.215368469184956,
-0.254786400524015));
#41585=CARTESIAN_POINT('Ctrl Pts',(-0.666768976221095,-0.1098510848563,
-0.244410928273297));
#41586=CARTESIAN_POINT('Ctrl Pts',(-0.537577394806923,-0.409461404791647,
-0.234035456022579));
#41587=CARTESIAN_POINT('Ctrl Pts',(-0.283062281008399,-0.613615439195291,
-0.223659983771861));
#41588=CARTESIAN_POINT('Ctrl Pts',(0.0374422703654468,-0.674719300151826,
-0.213284511521142));
#41589=CARTESIAN_POINT('Ctrl Pts',(0.349217843106239,-0.578528363169896,
-0.202909039270424));
#41590=CARTESIAN_POINT('Ctrl Pts',(0.57958183196945,-0.347466676531802,
-0.192533567019706));
#41591=CARTESIAN_POINT('Ctrl Pts',(0.674829137420516,-0.0354020866616497,
-0.182158094768987));
#41592=CARTESIAN_POINT('Ctrl Pts',(0.612757328717359,0.28491729225613,-0.171782622518269));
#41593=CARTESIAN_POINT('Ctrl Pts',(0.407832523308644,0.538811651509414,
-0.161407150267551));
#41594=CARTESIAN_POINT('Ctrl Pts',(0.10783703441614,0.667101107632415,-0.151031678016832));
#41595=CARTESIAN_POINT('Ctrl Pts',(-0.21730991889707,0.639858795210619,
-0.140656205766114));
#41596=CARTESIAN_POINT('Ctrl Pts',(-0.491772539806295,0.463473885528119,
-0.130280733515396));
#41597=CARTESIAN_POINT('Ctrl Pts',(-0.651638943195009,0.178988927823084,
-0.119905261264677));
#41598=CARTESIAN_POINT('Ctrl Pts',(-0.656852632537107,-0.0384047749254474,
-0.112988279764198));
#41599=CARTESIAN_POINT('Ctrl Pts',(-0.633862107113883,-0.14143803926975,
-0.109529789013959));
#41600=CARTESIAN_POINT('Ctrl Pts',(0.470014347211915,-0.451297101048697,
-0.738715226741092));
#41601=CARTESIAN_POINT('Ctrl Pts',(0.54337417968881,-0.374894718465072,
-0.735256735990852));
#41602=CARTESIAN_POINT('Ctrl Pts',(0.652074769329847,-0.185731384534561,
-0.728339754490373));
#41603=CARTESIAN_POINT('Ctrl Pts',(0.663066493609553,0.141492983497566,
-0.717964282239655));
#41604=CARTESIAN_POINT('Ctrl Pts',(0.519492261637952,0.435658392894028,
-0.707588809988937));
#41605=CARTESIAN_POINT('Ctrl Pts',(0.254804820165469,0.628295904325486,
-0.697213337738218));
#41606=CARTESIAN_POINT('Ctrl Pts',(-0.0692815491306441,0.67444310756472,
-0.6868378654875));
#41607=CARTESIAN_POINT('Ctrl Pts',(-0.377217976623324,0.563368652712182,
-0.676462393236782));
#41608=CARTESIAN_POINT('Ctrl Pts',(-0.597214148502112,0.320953486159955,
-0.666086920986063));
#41609=CARTESIAN_POINT('Ctrl Pts',(-0.677984188465101,0.00371779474059088,
-0.655711448735345));
#41610=CARTESIAN_POINT('Ctrl Pts',(-0.600697910587708,-0.314385751893901,
-0.645335976484627));
#41611=CARTESIAN_POINT('Ctrl Pts',(-0.383373073457732,-0.559197050461262,
-0.634960504233908));
#41612=CARTESIAN_POINT('Ctrl Pts',(-0.076673736305239,-0.673644939952962,
-0.62458503198319));
#41613=CARTESIAN_POINT('Ctrl Pts',(0.247900263823826,-0.631048142615807,
-0.614209559732472));
#41614=CARTESIAN_POINT('Ctrl Pts',(0.514682134447219,-0.441337321657616,
-0.603834087481753));
#41615=CARTESIAN_POINT('Ctrl Pts',(0.661477912573016,-0.148739002946069,
-0.593458615231035));
#41616=CARTESIAN_POINT('Ctrl Pts',(0.654065609005064,0.178534312695462,
-0.583083142980317));
#41617=CARTESIAN_POINT('Ctrl Pts',(0.494173224329236,0.464186543549856,
-0.572707670729598));
#41618=CARTESIAN_POINT('Ctrl Pts',(0.21907592584049,0.641624547587032,-0.56233219847888));
#41619=CARTESIAN_POINT('Ctrl Pts',(-0.107093794744453,0.669482816449697,
-0.551956726228162));
#41620=CARTESIAN_POINT('Ctrl Pts',(-0.408297104852174,0.541266843632825,
-0.541581253977443));
#41621=CARTESIAN_POINT('Ctrl Pts',(-0.614315506682938,0.286867182364573,
-0.531205781726725));
#41622=CARTESIAN_POINT('Ctrl Pts',(-0.677120634309526,-0.0344088448266699,
-0.520830309476007));
#41623=CARTESIAN_POINT('Ctrl Pts',(-0.58207094308648,-0.347663255493916,
-0.510454837225289));
#41624=CARTESIAN_POINT('Ctrl Pts',(-0.351325042584235,-0.579868119901137,
-0.50007936497457));
#41625=CARTESIAN_POINT('Ctrl Pts',(-0.0386759358456004,-0.676890311642653,
-0.489703892723852));
#41626=CARTESIAN_POINT('Ctrl Pts',(0.282989559613697,-0.616111378865716,
-0.479328420473133));
#41627=CARTESIAN_POINT('Ctrl Pts',(0.538682666382641,-0.411700506379297,
-0.468952948222416));
#41628=CARTESIAN_POINT('Ctrl Pts',(0.66879452451883,-0.111311302162335,
-0.458577475971697));
#41629=CARTESIAN_POINT('Ctrl Pts',(0.642992601295546,0.215027525434478,
-0.448202003720979));
#41630=CARTESIAN_POINT('Ctrl Pts',(0.467292010875556,0.491237721054596,
-0.43782653147026));
#41631=CARTESIAN_POINT('Ctrl Pts',(0.182653231305575,0.652927345965089,
-0.427451059219542));
#41632=CARTESIAN_POINT('Ctrl Pts',(-0.144566871714838,0.662402250613341,
-0.417075586968824));
#41633=CARTESIAN_POINT('Ctrl Pts',(-0.438084594105287,0.517453582867965,
-0.406700114718105));
#41634=CARTESIAN_POINT('Ctrl Pts',(-0.629473152578393,0.251872730160416,
-0.396324642467387));
#41635=CARTESIAN_POINT('Ctrl Pts',(-0.674114786718943,-0.0724263511503591,
-0.385949170216669));
#41636=CARTESIAN_POINT('Ctrl Pts',(-0.561602344963072,-0.379840924796351,
-0.375573697965951));
#41637=CARTESIAN_POINT('Ctrl Pts',(-0.318165468246377,-0.59870448204835,
-0.365198225715232));
#41638=CARTESIAN_POINT('Ctrl Pts',(-0.000555763515644371,-0.67799410996808,
-0.354822753464514));
#41639=CARTESIAN_POINT('Ctrl Pts',(0.317183504488467,-0.599225288590716,
-0.344447281213795));
#41640=CARTESIAN_POINT('Ctrl Pts',(0.560978866271118,-0.380761124075465,
-0.334071808963077));
#41641=CARTESIAN_POINT('Ctrl Pts',(0.673995142653298,-0.073531420145835,
-0.323696336712359));
#41642=CARTESIAN_POINT('Ctrl Pts',(0.629885235153281,0.250840412180345,
-0.313320864461641));
#41643=CARTESIAN_POINT('Ctrl Pts',(0.438932336307417,0.5167346771196,-0.302945392210922));
#41644=CARTESIAN_POINT('Ctrl Pts',(0.145652641531586,0.662164352229869,
-0.292569919960204));
#41645=CARTESIAN_POINT('Ctrl Pts',(-0.181582554148068,0.653225917187752,
-0.282194447709485));
#41646=CARTESIAN_POINT('Ctrl Pts',(-0.466486032729584,0.492003153405566,
-0.271818975458767));
#41647=CARTESIAN_POINT('Ctrl Pts',(-0.642639211032385,0.216081383425365,
-0.261443503208049));
#41648=CARTESIAN_POINT('Ctrl Pts',(-0.668976118852786,-0.11021471504172,
-0.251068030957331));
#41649=CARTESIAN_POINT('Ctrl Pts',(-0.539356886880686,-0.410816805495047,
-0.240692558706612));
#41650=CARTESIAN_POINT('Ctrl Pts',(-0.283999275223193,-0.615646634552595,
-0.230317086455894));
#41651=CARTESIAN_POINT('Ctrl Pts',(0.03756621147893,-0.676952756440303,
-0.219941614205175));
#41652=CARTESIAN_POINT('Ctrl Pts',(0.350373827149244,-0.58044341845448,
-0.209566141954457));
#41653=CARTESIAN_POINT('Ctrl Pts',(0.581500365212223,-0.348616848509172,
-0.199190669703739));
#41654=CARTESIAN_POINT('Ctrl Pts',(0.677062964974281,-0.0355193033372838,
-0.18881519745302));
#41655=CARTESIAN_POINT('Ctrl Pts',(0.614785673653287,0.285860483832951,
-0.178439725202302));
#41656=CARTESIAN_POINT('Ctrl Pts',(0.409182549063095,0.540595116453827,
-0.168064252951584));
#41657=CARTESIAN_POINT('Ctrl Pts',(0.108193965249678,0.669309573855992,
-0.157688780700866));
#41658=CARTESIAN_POINT('Ctrl Pts',(-0.218029195802555,0.641976413101301,
-0.147313308450147));
#41659=CARTESIAN_POINT('Ctrl Pts',(-0.493400536410654,0.465008978404062,
-0.136937836199429));
#41660=CARTESIAN_POINT('Ctrl Pts',(-0.653795728983253,0.1795794998349,-0.126562363948711));
#41661=CARTESIAN_POINT('Ctrl Pts',(-0.659027376817395,-0.038528764458213,
-0.119645382448232));
#41662=CARTESIAN_POINT('Ctrl Pts',(-0.635960060745575,-0.141906170184684,
-0.116186891697992));
#41663=CARTESIAN_POINT('Ctrl Pts',(0.470014347211915,-0.451297101048697,
-0.742528335043099));
#41664=CARTESIAN_POINT('Ctrl Pts',(0.543372589191722,-0.374896374926965,
-0.73906984429286));
#41665=CARTESIAN_POINT('Ctrl Pts',(0.652075459781473,-0.185730254682432,
-0.732152862792381));
#41666=CARTESIAN_POINT('Ctrl Pts',(0.66306588519074,0.14149243809354,-0.721777390541662));
#41667=CARTESIAN_POINT('Ctrl Pts',(0.519492314280382,0.435658515066948,
-0.711401918290944));
#41668=CARTESIAN_POINT('Ctrl Pts',(0.254804642144546,0.628295593947961,
-0.701026446040226));
#41669=CARTESIAN_POINT('Ctrl Pts',(-0.0692814769404281,0.674442972356818,
-0.690650973789507));
#41670=CARTESIAN_POINT('Ctrl Pts',(-0.377217891740993,0.563368455293,-0.680275501538789));
#41671=CARTESIAN_POINT('Ctrl Pts',(-0.597213959773261,0.320953407732286,
-0.669900029288071));
#41672=CARTESIAN_POINT('Ctrl Pts',(-0.677983995666914,0.00371778562304485,
-0.659524557037352));
#41673=CARTESIAN_POINT('Ctrl Pts',(-0.600697730621323,-0.314385655403825,
-0.649149084786635));
#41674=CARTESIAN_POINT('Ctrl Pts',(-0.383372962378955,-0.559196888039266,
-0.638773612535916));
#41675=CARTESIAN_POINT('Ctrl Pts',(-0.0766737129197174,-0.67364474082535,
-0.628398140285198));
#41676=CARTESIAN_POINT('Ctrl Pts',(0.247900190499642,-0.631047957547907,
-0.618022668034479));
#41677=CARTESIAN_POINT('Ctrl Pts',(0.514681983299422,-0.441337191609865,
-0.60764719578376));
#41678=CARTESIAN_POINT('Ctrl Pts',(0.661477717937038,-0.148738959334052,
-0.597271723533043));
#41679=CARTESIAN_POINT('Ctrl Pts',(0.654065416708807,0.178534260256687,
-0.586896251282324));
#41680=CARTESIAN_POINT('Ctrl Pts',(0.494173078974265,0.46418640700759,-0.576520779031606));
#41681=CARTESIAN_POINT('Ctrl Pts',(0.219075861427449,0.641624358912467,
-0.566145306780888));
#41682=CARTESIAN_POINT('Ctrl Pts',(-0.107093763256759,0.669482619557719,
-0.555769834530169));
#41683=CARTESIAN_POINT('Ctrl Pts',(-0.408296984775409,0.54126668445947,
-0.545394362279451));
#41684=CARTESIAN_POINT('Ctrl Pts',(-0.614315326024746,0.28686709799964,
-0.535018890028733));
#41685=CARTESIAN_POINT('Ctrl Pts',(-0.677120435178814,-0.0344088347065514,
-0.524643417778014));
#41686=CARTESIAN_POINT('Ctrl Pts',(-0.582070771909591,-0.3476631532525,
-0.514267945527297));
#41687=CARTESIAN_POINT('Ctrl Pts',(-0.351324939265201,-0.579867949371361,
-0.503892473276577));
#41688=CARTESIAN_POINT('Ctrl Pts',(-0.0386759244717649,-0.676890112580673,
-0.49351700102586));
#41689=CARTESIAN_POINT('Ctrl Pts',(0.282989476391259,-0.616111197677603,
-0.483141528775141));
#41690=CARTESIAN_POINT('Ctrl Pts',(0.538682507965055,-0.411700385305101,
-0.472766056524423));
#41691=CARTESIAN_POINT('Ctrl Pts',(0.668794327837566,-0.111311269427527,
-0.462390584273704));
#41692=CARTESIAN_POINT('Ctrl Pts',(0.642992412202175,0.215027462198472,
-0.452015112022986));
#41693=CARTESIAN_POINT('Ctrl Pts',(0.467291873452798,0.491237576589808,
-0.441639639772268));
#41694=CARTESIAN_POINT('Ctrl Pts',(0.182653177590315,0.652927153950078,
-0.431264167521549));
#41695=CARTESIAN_POINT('Ctrl Pts',(-0.14456682920014,0.66240205581193,-0.420888695270831));
#41696=CARTESIAN_POINT('Ctrl Pts',(-0.438084465271938,0.517453430693514,
-0.410513223020113));
#41697=CARTESIAN_POINT('Ctrl Pts',(-0.629472967460876,0.251872656088883,
-0.400137750769395));
#41698=CARTESIAN_POINT('Ctrl Pts',(-0.674114588473059,-0.0724263298510245,
-0.389762278518676));
#41699=CARTESIAN_POINT('Ctrl Pts',(-0.561602179805233,-0.379840813091406,
-0.379386806267958));
#41700=CARTESIAN_POINT('Ctrl Pts',(-0.318165374679212,-0.598704305979552,
-0.369011334017239));
#41701=CARTESIAN_POINT('Ctrl Pts',(-0.000555763352252093,-0.677993910581017,
-0.358635861766521));
#41702=CARTESIAN_POINT('Ctrl Pts',(0.317183411210203,-0.599225112369264,
-0.348260389515803));
#41703=CARTESIAN_POINT('Ctrl Pts',(0.560978701296429,-0.380761012098642,
-0.337884917265085));
#41704=CARTESIAN_POINT('Ctrl Pts',(0.673994944442988,-0.0735313985241569,
-0.327509445014366));
#41705=CARTESIAN_POINT('Ctrl Pts',(0.629885049913813,0.250840338417712,
-0.317133972763648));
#41706=CARTESIAN_POINT('Ctrl Pts',(0.438932207226276,0.516734525145969,
-0.306758500512929));
#41707=CARTESIAN_POINT('Ctrl Pts',(0.145652598694571,0.662164157519516,
-0.296383028262211));
#41708=CARTESIAN_POINT('Ctrl Pts',(-0.18158250074169,0.653225725042971,
-0.286007556011493));
#41709=CARTESIAN_POINT('Ctrl Pts',(-0.466485895555756,0.492003008799146,
-0.275632083760774));
#41710=CARTESIAN_POINT('Ctrl Pts',(-0.642639022019262,0.216081319713422,
-0.265256611510056));
#41711=CARTESIAN_POINT('Ctrl Pts',(-0.66897592216521,-0.110214682299213,
-0.254881139259338));
#41712=CARTESIAN_POINT('Ctrl Pts',(-0.539356728171161,-0.410816685337444,
-0.24450566700862));
#41713=CARTESIAN_POINT('Ctrl Pts',(-0.283999191890099,-0.615646452195022,
-0.234130194757901));
#41714=CARTESIAN_POINT('Ctrl Pts',(0.0375662008019495,-0.67695255995773,
-0.223754722507183));
#41715=CARTESIAN_POINT('Ctrl Pts',(0.350373723373049,-0.580443242588805,
-0.213379250256465));
#41716=CARTESIAN_POINT('Ctrl Pts',(0.581500195668746,-0.34861675626341,
-0.203003778005746));
#41717=CARTESIAN_POINT('Ctrl Pts',(0.67706276294556,-0.0355192724524337,
-0.192628305755028));
#41718=CARTESIAN_POINT('Ctrl Pts',(0.614785498654458,0.285860359114252,
-0.18225283350431));
#41719=CARTESIAN_POINT('Ctrl Pts',(0.409182417194479,0.540595038330385,
-0.171877361253591));
#41720=CARTESIAN_POINT('Ctrl Pts',(0.108193956380082,0.66930921615921,-0.161501889002873));
#41721=CARTESIAN_POINT('Ctrl Pts',(-0.218029177410119,0.641976544855489,
-0.151126416752155));
#41722=CARTESIAN_POINT('Ctrl Pts',(-0.493400299308284,0.46500819646962,
-0.140750944501436));
#41723=CARTESIAN_POINT('Ctrl Pts',(-0.653795732950318,0.17958082394726,
-0.130375472250718));
#41724=CARTESIAN_POINT('Ctrl Pts',(-0.659026876700399,-0.0385310057591697,
-0.123458490750239));
#41725=CARTESIAN_POINT('Ctrl Pts',(-0.635960060745575,-0.141906170184684,
-0.12));
#41726=CARTESIAN_POINT('Ctrl Pts',(-0.548572772984126,0.332979158385831,
-0.12));
#41727=CARTESIAN_POINT('Ctrl Pts',(-0.577197265262902,0.291949500684259,
-0.12));
#41728=CARTESIAN_POINT('Ctrl Pts',(-0.611328090029018,0.228891973083493,
-0.12));
#41729=CARTESIAN_POINT('Ctrl Pts',(-0.643583475482228,0.101487125632845,
-0.12));
#41730=CARTESIAN_POINT('Ctrl Pts',(-0.649841246643075,0.0550307489159153,
-0.12));
#41731=CARTESIAN_POINT('Ctrl Pts',(-0.651978221577845,-0.0421309211851907,
-0.12));
#41732=CARTESIAN_POINT('Ctrl Pts',(-0.646960254890958,-0.0926082141634192,
-0.12));
#41733=CARTESIAN_POINT('Ctrl Pts',(-0.635960060745575,-0.141906170184684,
-0.12));
#41734=CARTESIAN_POINT('Origin',(0.,0.,0.0705711144245887));
#41735=CARTESIAN_POINT('',(-0.9025,-1.10524373623049E-16,-5.55111512312578E-17));
#41736=CARTESIAN_POINT('Origin',(0.,0.,0.));
#41737=CARTESIAN_POINT('',(-0.95,-1.33616303797361E-16,0.0274241377865074));
#41738=CARTESIAN_POINT('',(-1.02473275573014,-1.25493568928637E-16,0.0705711144245887));
#41739=CARTESIAN_POINT('',(-0.95,0.548482755730144,0.112274715389696));
#41740=CARTESIAN_POINT('Ctrl Pts',(-0.95,0.548482755730144,0.112274715389696));
#41741=CARTESIAN_POINT('Ctrl Pts',(-0.95,0.254551732809566,0.0274241377865074));
#41742=CARTESIAN_POINT('Ctrl Pts',(-0.95,-1.50891161675723E-16,0.0274241377865074));
#41743=CARTESIAN_POINT('',(6.71697651192441E-17,1.09696551146029,0.112274715389696));
#41744=CARTESIAN_POINT('Ctrl Pts',(6.71697651192441E-17,1.09696551146029,
0.112274715389696));
#41745=CARTESIAN_POINT('Ctrl Pts',(-0.475000000000001,0.822724133595216,
-0.0460586179436371));
#41746=CARTESIAN_POINT('Ctrl Pts',(-0.95,0.548482755730144,0.112274715389696));
#41747=CARTESIAN_POINT('',(0.95,0.548482755730144,0.112274715389696));
#41748=CARTESIAN_POINT('Ctrl Pts',(0.95,0.548482755730144,0.112274715389696));
#41749=CARTESIAN_POINT('Ctrl Pts',(0.475,0.822724133595217,-0.0460586179436373));
#41750=CARTESIAN_POINT('Ctrl Pts',(6.71697651192441E-17,1.09696551146029,
0.112274715389696));
#41751=CARTESIAN_POINT('',(0.95,-0.548482755730145,0.112274715389696));
#41752=CARTESIAN_POINT('Ctrl Pts',(0.95,-0.548482755730145,0.112274715389696));
#41753=CARTESIAN_POINT('Ctrl Pts',(0.95,-1.11022302462516E-16,-0.0460586179436371));
#41754=CARTESIAN_POINT('Ctrl Pts',(0.95,0.548482755730144,0.112274715389696));
#41755=CARTESIAN_POINT('',(-2.01509295357732E-16,-1.09696551146029,0.112274715389696));
#41756=CARTESIAN_POINT('Ctrl Pts',(-2.01509295357732E-16,-1.09696551146029,
0.112274715389696));
#41757=CARTESIAN_POINT('Ctrl Pts',(0.475,-0.822724133595217,-0.0460586179436371));
#41758=CARTESIAN_POINT('Ctrl Pts',(0.95,-0.548482755730145,0.112274715389696));
#41759=CARTESIAN_POINT('',(-0.95,-0.548482755730145,0.112274715389696));
#41760=CARTESIAN_POINT('Ctrl Pts',(-0.95,-0.548482755730145,0.112274715389696));
#41761=CARTESIAN_POINT('Ctrl Pts',(-0.475,-0.822724133595217,-0.0460586179436367));
#41762=CARTESIAN_POINT('Ctrl Pts',(-2.01509295357732E-16,-1.09696551146029,
0.112274715389696));
#41763=CARTESIAN_POINT('Ctrl Pts',(-0.95,-1.50891161675723E-16,0.0274241377865074));
#41764=CARTESIAN_POINT('Ctrl Pts',(-0.95,-0.254551732809567,0.0274241377865074));
#41765=CARTESIAN_POINT('Ctrl Pts',(-0.95,-0.548482755730145,0.112274715389696));
#41766=CARTESIAN_POINT('Origin',(-2.01509295357732E-16,-1.09696551146029,
0.));
#41767=CARTESIAN_POINT('',(0.95,-0.548482755730145,0.587725284610304));
#41768=CARTESIAN_POINT('',(0.95,-0.548482755730145,0.));
#41769=CARTESIAN_POINT('',(-2.01509295357732E-16,-1.09696551146029,0.587725284610304));
#41770=CARTESIAN_POINT('Ctrl Pts',(0.95,-0.548482755730145,0.587725284610304));
#41771=CARTESIAN_POINT('Ctrl Pts',(0.475,-0.822724133595217,0.746058617943637));
#41772=CARTESIAN_POINT('Ctrl Pts',(-2.01509295357732E-16,-1.09696551146029,
0.587725284610304));
#41773=CARTESIAN_POINT('',(-2.01509295357732E-16,-1.09696551146029,0.));
#41774=CARTESIAN_POINT('Origin',(0.95,-0.548482755730145,0.));
#41775=CARTESIAN_POINT('',(0.95,0.548482755730144,0.587725284610304));
#41776=CARTESIAN_POINT('',(0.95,0.548482755730144,0.));
#41777=CARTESIAN_POINT('Ctrl Pts',(0.95,0.548482755730144,0.587725284610304));
#41778=CARTESIAN_POINT('Ctrl Pts',(0.95,-7.7715611723761E-16,0.746058617943637));
#41779=CARTESIAN_POINT('Ctrl Pts',(0.95,-0.548482755730145,0.587725284610304));
#41780=CARTESIAN_POINT('Origin',(0.95,0.548482755730144,0.));
#41781=CARTESIAN_POINT('',(6.71697651192441E-17,1.09696551146029,0.587725284610304));
#41782=CARTESIAN_POINT('',(6.71697651192441E-17,1.09696551146029,0.));
#41783=CARTESIAN_POINT('Ctrl Pts',(6.71697651192441E-17,1.09696551146029,
0.587725284610304));
#41784=CARTESIAN_POINT('Ctrl Pts',(0.475,0.822724133595216,0.746058617943637));
#41785=CARTESIAN_POINT('Ctrl Pts',(0.95,0.548482755730144,0.587725284610304));
#41786=CARTESIAN_POINT('Origin',(0.,0.,0.629428885575411));
#41787=CARTESIAN_POINT('',(-0.95,0.548482755730144,0.587725284610304));
#41788=CARTESIAN_POINT('Ctrl Pts',(-0.95,0.548482755730144,0.587725284610304));
#41789=CARTESIAN_POINT('Ctrl Pts',(-0.475,0.822724133595217,0.746058617943637));
#41790=CARTESIAN_POINT('Ctrl Pts',(6.71697651192441E-17,1.09696551146029,
0.587725284610304));
#41791=CARTESIAN_POINT('',(-0.95,-7.07449864324762E-17,0.672575862213493));
#41792=CARTESIAN_POINT('Ctrl Pts',(-0.95,-2.51485269459538E-17,0.672575862213493));
#41793=CARTESIAN_POINT('Ctrl Pts',(-0.95,0.254551732809567,0.672575862213493));
#41794=CARTESIAN_POINT('Ctrl Pts',(-0.95,0.548482755730144,0.587725284610304));
#41795=CARTESIAN_POINT('',(-0.9025,-1.10524373623049E-16,0.7));
#41796=CARTESIAN_POINT('',(-1.02473275573014,-1.25493568928637E-16,0.629428885575411));
#41797=CARTESIAN_POINT('Origin',(0.,0.,0.7));
#41798=CARTESIAN_POINT('',(-0.95,-0.548482755730145,0.587725284610304));
#41799=CARTESIAN_POINT('Ctrl Pts',(-0.95,-0.548482755730145,0.587725284610304));
#41800=CARTESIAN_POINT('Ctrl Pts',(-0.95,-0.254551732809567,0.672575862213493));
#41801=CARTESIAN_POINT('Ctrl Pts',(-0.95,-2.51485269459538E-17,0.672575862213493));
#41802=CARTESIAN_POINT('Ctrl Pts',(-2.01509295357732E-16,-1.09696551146029,
0.587725284610304));
#41803=CARTESIAN_POINT('Ctrl Pts',(-0.475,-0.822724133595217,0.746058617943637));
#41804=CARTESIAN_POINT('Ctrl Pts',(-0.95,-0.548482755730145,0.587725284610304));
#41805=CARTESIAN_POINT('Origin',(6.71697651192441E-17,1.09696551146029,
0.));
#41806=CARTESIAN_POINT('',(-0.95,0.548482755730144,0.));
#41807=CARTESIAN_POINT('Origin',(0.,0.,0.7));
#41808=CARTESIAN_POINT('Origin',(0.,0.,0.7));
#41809=CARTESIAN_POINT('',(-0.3,3.67394039744206E-17,0.7));
#41810=CARTESIAN_POINT('Origin',(0.,0.,0.7));
#41811=CARTESIAN_POINT('Origin',(0.,0.,0.));
#41812=CARTESIAN_POINT('',(-0.56785,6.95415684895825E-17,0.));
#41813=CARTESIAN_POINT('Origin',(0.,0.,0.));
#41814=CARTESIAN_POINT('Origin',(0.,0.,0.));
#41815=CARTESIAN_POINT('',(-0.3,-3.67394039744206E-17,0.));
#41816=CARTESIAN_POINT('Origin',(0.,0.,0.));
#41817=CARTESIAN_POINT('Origin',(-0.95,-0.548482755730145,0.));
#41818=CARTESIAN_POINT('',(-0.95,-0.548482755730145,0.));
#41819=CARTESIAN_POINT('Origin',(-0.95,0.548482755730144,0.));
#41820=CARTESIAN_POINT('Origin',(0.,0.,0.0765832901469392));
#41821=CARTESIAN_POINT('',(-0.3,-3.67394039744206E-17,-0.8));
#41822=CARTESIAN_POINT('',(-0.3,-3.67394039744206E-17,0.0765832901469392));
#41823=CARTESIAN_POINT('Origin',(0.,0.,-0.8));
#41824=CARTESIAN_POINT('Origin',(0.,0.,0.0765832901469392));
#41825=CARTESIAN_POINT('',(-0.3,-3.67394039744206E-17,0.953166580293878));
#41826=CARTESIAN_POINT('Origin',(0.,0.,0.953166580293878));
#41827=CARTESIAN_POINT('',(-0.3,-3.67394039744206E-17,0.0765832901469392));
#41828=CARTESIAN_POINT('Origin',(0.57785,0.,-0.8));
#41829=CARTESIAN_POINT('',(-0.57785,-7.07662152887298E-17,-0.8));
#41830=CARTESIAN_POINT('Origin',(0.,0.,-0.8));
#41831=CARTESIAN_POINT('Origin',(0.,0.,-0.76));
#41832=CARTESIAN_POINT('',(-0.61785,-7.56648024853192E-17,-0.76));
#41833=CARTESIAN_POINT('Origin',(0.56785,0.,-0.12));
#41834=CARTESIAN_POINT('',(-0.56785,-6.95415684895825E-17,-0.12));
#41835=CARTESIAN_POINT('Origin',(0.,0.,-0.12));
#41836=CARTESIAN_POINT('Origin',(0.,0.,-0.0349999999999999));
#41837=CARTESIAN_POINT('',(-0.56785,-6.95415684895825E-17,-0.0349999999999999));
#41838=CARTESIAN_POINT('Origin',(0.,0.,1.77));
#41839=CARTESIAN_POINT('',(-0.64,-7.83773951454306E-17,1.8));
#41840=CARTESIAN_POINT('Origin',(0.,0.,1.8));
#41841=CARTESIAN_POINT('',(-0.67,-8.20513355428727E-17,1.77));
#41842=CARTESIAN_POINT('Origin',(0.48,0.,1.8));
#41843=CARTESIAN_POINT('',(-0.48,-5.8783046359073E-17,1.8));
#41844=CARTESIAN_POINT('Origin',(0.,0.,1.8));
#41845=CARTESIAN_POINT('Origin',(0.,0.,1.37658329014694));
#41846=CARTESIAN_POINT('',(-0.39,-4.77612251667468E-17,1.37658329014694));
#41847=CARTESIAN_POINT('',(0.,0.,0.));
#41848=CARTESIAN_POINT('Origin',(0.,0.,-16.505));
#41849=CARTESIAN_POINT('',(-0.24404761904762,-2.98872135506201E-17,-16.6));
#41850=CARTESIAN_POINT('Origin',(0.,0.,-16.6));
#41851=CARTESIAN_POINT('',(-0.125,-1.53080849893419E-17,-16.4));
#41852=CARTESIAN_POINT('',(-0.1875,-2.29621274840129E-17,-16.505));
#41853=CARTESIAN_POINT('Origin',(0.,0.,-16.4));
#41854=CARTESIAN_POINT('Origin',(0.,0.,-16.4));
#41855=CARTESIAN_POINT('',(0.,0.,-16.325));
#41856=CARTESIAN_POINT('',(-0.125,-1.53080849893419E-17,-16.4));
#41857=CARTESIAN_POINT('Origin',(0.75,-0.3,-14.));
#41858=CARTESIAN_POINT('',(1.05830052442584,-0.3,-15.9));
#41859=CARTESIAN_POINT('',(1.05830052442584,-0.3,-14.));
#41860=CARTESIAN_POINT('',(1.05830052442584,-0.3,-14.75));
#41861=CARTESIAN_POINT('',(0.75,-0.3,-15.9));
#41862=CARTESIAN_POINT('',(0.75,-0.3,-15.9));
#41863=CARTESIAN_POINT('',(0.75,-0.3,-14.));
#41864=CARTESIAN_POINT('',(0.75,-0.3,-15.9));
#41865=CARTESIAN_POINT('',(0.75,-0.3,-14.));
#41866=CARTESIAN_POINT('Origin',(0.75,0.,-14.));
#41867=CARTESIAN_POINT('',(1.05830052442584,0.3,-14.));
#41868=CARTESIAN_POINT('Ctrl Pts',(1.05830052442584,-0.3,-14.));
#41869=CARTESIAN_POINT('Ctrl Pts',(1.05830052442584,-0.3,-13.9621197920773));
#41870=CARTESIAN_POINT('Ctrl Pts',(1.06054662122175,-0.292390180522678,
-13.9218545194158));
#41871=CARTESIAN_POINT('Ctrl Pts',(1.06852962982332,-0.261716593696817,
-13.8480027362622));
#41872=CARTESIAN_POINT('Ctrl Pts',(1.0741374678263,-0.238662416759524,-13.8143983480476));
#41873=CARTESIAN_POINT('Ctrl Pts',(1.0845648020257,-0.185606967199746,-13.7613428984878));
#41874=CARTESIAN_POINT('Ctrl Pts',(1.09008017269667,-0.152000388353929,
-13.7382845890765));
#41875=CARTESIAN_POINT('Ctrl Pts',(1.09784922615088,-0.07814075455321,-13.7076079715749));
#41876=CARTESIAN_POINT('Ctrl Pts',(1.1,-0.0378726187868804,-13.7));
#41877=CARTESIAN_POINT('Ctrl Pts',(1.1,0.0378726187868803,-13.7));
#41878=CARTESIAN_POINT('Ctrl Pts',(1.09784922615088,0.07814075455321,-13.7076079715749));
#41879=CARTESIAN_POINT('Ctrl Pts',(1.09008017269667,0.152000388353929,-13.7382845890765));
#41880=CARTESIAN_POINT('Ctrl Pts',(1.0845648020257,0.185606967199746,-13.7613428984878));
#41881=CARTESIAN_POINT('Ctrl Pts',(1.0741374678263,0.238662416759524,-13.8143983480476));
#41882=CARTESIAN_POINT('Ctrl Pts',(1.06852962982332,0.261716593696815,-13.8480027362621));
#41883=CARTESIAN_POINT('Ctrl Pts',(1.06054662122175,0.292390180522677,-13.9218545194158));
#41884=CARTESIAN_POINT('Ctrl Pts',(1.05830052442584,0.3,-13.9621197920773));
#41885=CARTESIAN_POINT('Ctrl Pts',(1.05830052442584,0.3,-14.));
#41886=CARTESIAN_POINT('',(0.75,0.3,-14.));
#41887=CARTESIAN_POINT('Origin',(0.75,0.,-14.));
#41888=CARTESIAN_POINT('',(0.75,0.3,-14.));
#41889=CARTESIAN_POINT('Origin',(0.75,0.3,-15.9));
#41890=CARTESIAN_POINT('',(1.05830052442584,0.3,-15.9));
#41891=CARTESIAN_POINT('',(1.05830052442584,0.3,-14.75));
#41892=CARTESIAN_POINT('',(0.75,0.3,-15.9));
#41893=CARTESIAN_POINT('',(0.75,0.3,-14.));
#41894=CARTESIAN_POINT('',(0.75,0.3,-15.9));
#41895=CARTESIAN_POINT('Origin',(0.75,0.,-15.9));
#41896=CARTESIAN_POINT('Ctrl Pts',(1.05830052442584,0.3,-15.9));
#41897=CARTESIAN_POINT('Ctrl Pts',(1.05830052442584,0.3,-15.9378802079227));
#41898=CARTESIAN_POINT('Ctrl Pts',(1.06054662122175,0.292390180522678,-15.9781454805842));
#41899=CARTESIAN_POINT('Ctrl Pts',(1.06852962982332,0.261716593696816,-16.0519972637378));
#41900=CARTESIAN_POINT('Ctrl Pts',(1.0741374678263,0.238662416759525,-16.0856016519524));
#41901=CARTESIAN_POINT('Ctrl Pts',(1.0845648020257,0.185606967199746,-16.1386571015122));
#41902=CARTESIAN_POINT('Ctrl Pts',(1.09008017269667,0.15200038835393,-16.1617154109235));
#41903=CARTESIAN_POINT('Ctrl Pts',(1.09784922615088,0.0781407545532106,
-16.1923920284251));
#41904=CARTESIAN_POINT('Ctrl Pts',(1.1,0.0378726187868802,-16.2));
#41905=CARTESIAN_POINT('Ctrl Pts',(1.1,-0.0378726187868802,-16.2));
#41906=CARTESIAN_POINT('Ctrl Pts',(1.09784922615088,-0.0781407545532106,
-16.1923920284251));
#41907=CARTESIAN_POINT('Ctrl Pts',(1.09008017269667,-0.152000388353928,
-16.1617154109235));
#41908=CARTESIAN_POINT('Ctrl Pts',(1.0845648020257,-0.185606967199746,-16.1386571015122));
#41909=CARTESIAN_POINT('Ctrl Pts',(1.0741374678263,-0.238662416759525,-16.0856016519524));
#41910=CARTESIAN_POINT('Ctrl Pts',(1.06852962982332,-0.261716593696816,
-16.0519972637378));
#41911=CARTESIAN_POINT('Ctrl Pts',(1.06054662122175,-0.292390180522678,
-15.9781454805842));
#41912=CARTESIAN_POINT('Ctrl Pts',(1.05830052442584,-0.3,-15.9378802079227));
#41913=CARTESIAN_POINT('Ctrl Pts',(1.05830052442584,-0.3,-15.9));
#41914=CARTESIAN_POINT('Origin',(0.75,0.,-15.9));
#41915=CARTESIAN_POINT('Origin',(0.75,0.,-14.95));
#41916=CARTESIAN_POINT('Origin',(0.85,-0.4,-0.6));
#41917=CARTESIAN_POINT('',(1.1842719282327,-0.4,-1.4));
#41918=CARTESIAN_POINT('',(1.1842719282327,-0.4,-0.6));
#41919=CARTESIAN_POINT('',(1.1842719282327,-0.4,-3.5525));
#41920=CARTESIAN_POINT('',(0.85,-0.4,-1.4));
#41921=CARTESIAN_POINT('',(0.85,-0.4,-1.4));
#41922=CARTESIAN_POINT('',(0.85,-0.4,-0.6));
#41923=CARTESIAN_POINT('',(0.85,-0.4,-1.4));
#41924=CARTESIAN_POINT('',(0.85,-0.4,-0.6));
#41925=CARTESIAN_POINT('Origin',(0.85,2.77555756156289E-17,-0.6));
#41926=CARTESIAN_POINT('',(1.1842719282327,0.4,-0.6));
#41927=CARTESIAN_POINT('Ctrl Pts',(1.1842719282327,-0.4,-0.6));
#41928=CARTESIAN_POINT('Ctrl Pts',(1.1842719282327,-0.4,-0.549378294110008));
#41929=CARTESIAN_POINT('Ctrl Pts',(1.18785814874083,-0.389809986586072,
-0.495648946446262));
#41930=CARTESIAN_POINT('Ctrl Pts',(1.20051612521885,-0.34888367623215,-0.39721643728222));
#41931=CARTESIAN_POINT('Ctrl Pts',(1.20937438602785,-0.318164321482014,
-0.352478896532776));
#41932=CARTESIAN_POINT('Ctrl Pts',(1.22578154244013,-0.247534895635844,
-0.281849470686606));
#41933=CARTESIAN_POINT('Ctrl Pts',(1.23443746535443,-0.202791815317204,
-0.251119471874504));
#41934=CARTESIAN_POINT('Ctrl Pts',(1.24662494888297,-0.10433893315722,-0.210185257163551));
#41935=CARTESIAN_POINT('Ctrl Pts',(1.25,-0.0506019394319205,-0.2));
#41936=CARTESIAN_POINT('Ctrl Pts',(1.25,0.0506019394319202,-0.2));
#41937=CARTESIAN_POINT('Ctrl Pts',(1.24662494888297,0.10433893315722,-0.210185257163551));
#41938=CARTESIAN_POINT('Ctrl Pts',(1.23443746535443,0.202791815317204,-0.251119471874504));
#41939=CARTESIAN_POINT('Ctrl Pts',(1.22578154244013,0.247534895635844,-0.281849470686606));
#41940=CARTESIAN_POINT('Ctrl Pts',(1.20937438602785,0.318164321482014,-0.352478896532776));
#41941=CARTESIAN_POINT('Ctrl Pts',(1.20051612521885,0.34888367623215,-0.39721643728222));
#41942=CARTESIAN_POINT('Ctrl Pts',(1.18785814874083,0.389809986586072,-0.495648946446262));
#41943=CARTESIAN_POINT('Ctrl Pts',(1.1842719282327,0.4,-0.549378294110007));
#41944=CARTESIAN_POINT('Ctrl Pts',(1.1842719282327,0.4,-0.6));
#41945=CARTESIAN_POINT('',(0.85,0.4,-0.6));
#41946=CARTESIAN_POINT('Origin',(0.85,2.77555756156289E-17,-0.6));
#41947=CARTESIAN_POINT('',(0.85,0.4,-0.6));
#41948=CARTESIAN_POINT('Origin',(0.85,0.4,-1.4));
#41949=CARTESIAN_POINT('',(1.1842719282327,0.4,-1.4));
#41950=CARTESIAN_POINT('',(1.1842719282327,0.4,-3.5525));
#41951=CARTESIAN_POINT('',(0.85,0.4,-1.4));
#41952=CARTESIAN_POINT('',(0.85,0.4,-0.6));
#41953=CARTESIAN_POINT('',(0.85,0.4,-1.4));
#41954=CARTESIAN_POINT('Origin',(0.85,2.77555756156289E-17,-1.4));
#41955=CARTESIAN_POINT('Ctrl Pts',(1.1842719282327,0.4,-1.4));
#41956=CARTESIAN_POINT('Ctrl Pts',(1.1842719282327,0.4,-1.45062170588999));
#41957=CARTESIAN_POINT('Ctrl Pts',(1.18785814874083,0.389809986586072,-1.50435105355374));
#41958=CARTESIAN_POINT('Ctrl Pts',(1.20051612521885,0.34888367623215,-1.60278356271778));
#41959=CARTESIAN_POINT('Ctrl Pts',(1.20937438602785,0.318164321482014,-1.64752110346722));
#41960=CARTESIAN_POINT('Ctrl Pts',(1.22578154244013,0.247534895635844,-1.71815052931339));
#41961=CARTESIAN_POINT('Ctrl Pts',(1.23443746535443,0.202791815317204,-1.7488805281255));
#41962=CARTESIAN_POINT('Ctrl Pts',(1.24662494888297,0.10433893315722,-1.78981474283645));
#41963=CARTESIAN_POINT('Ctrl Pts',(1.25,0.0506019394319202,-1.8));
#41964=CARTESIAN_POINT('Ctrl Pts',(1.25,-0.0506019394319203,-1.8));
#41965=CARTESIAN_POINT('Ctrl Pts',(1.24662494888297,-0.10433893315722,-1.78981474283645));
#41966=CARTESIAN_POINT('Ctrl Pts',(1.23443746535443,-0.202791815317204,
-1.7488805281255));
#41967=CARTESIAN_POINT('Ctrl Pts',(1.22578154244013,-0.247534895635844,
-1.71815052931339));
#41968=CARTESIAN_POINT('Ctrl Pts',(1.20937438602785,-0.318164321482014,
-1.64752110346722));
#41969=CARTESIAN_POINT('Ctrl Pts',(1.20051612521885,-0.34888367623215,-1.60278356271778));
#41970=CARTESIAN_POINT('Ctrl Pts',(1.18785814874083,-0.389809986586072,
-1.50435105355374));
#41971=CARTESIAN_POINT('Ctrl Pts',(1.1842719282327,-0.4,-1.45062170588999));
#41972=CARTESIAN_POINT('Ctrl Pts',(1.1842719282327,-0.4,-1.4));
#41973=CARTESIAN_POINT('Origin',(0.85,2.77555756156289E-17,-1.4));
#41974=CARTESIAN_POINT('Origin',(0.85,0.,-1.));
#41975=CARTESIAN_POINT('Origin',(1.,0.,-16.6));
#41976=CARTESIAN_POINT('',(-1.,-1.22464679914736E-16,-16.6));
#41977=CARTESIAN_POINT('Origin',(0.,0.,-16.6));
#41978=CARTESIAN_POINT('Origin',(0.,0.,-16.55));
#41979=CARTESIAN_POINT('',(-1.1,-1.34711147906209E-16,-16.5));
#41980=CARTESIAN_POINT('Origin',(0.,0.,-16.5));
#41981=CARTESIAN_POINT('',(-1.05,-1.28587913910472E-16,-16.55));
#41982=CARTESIAN_POINT('Origin',(0.,0.,-14.75));
#41983=CARTESIAN_POINT('',(-1.1,-1.34711147906209E-16,-13.));
#41984=CARTESIAN_POINT('Origin',(0.,0.,-13.));
#41985=CARTESIAN_POINT('',(-1.1,-1.34711147906209E-16,-14.75));
#41986=CARTESIAN_POINT('Origin',(1.2,0.,-13.));
#41987=CARTESIAN_POINT('',(-1.2,-1.46957615897682E-16,-13.));
#41988=CARTESIAN_POINT('Origin',(0.,0.,-13.));
#41989=CARTESIAN_POINT('Origin',(0.,0.,-12.975));
#41990=CARTESIAN_POINT('',(-1.25,-1.53080849893419E-16,-12.95));
#41991=CARTESIAN_POINT('Origin',(0.,0.,-12.95));
#41992=CARTESIAN_POINT('',(-1.225,-1.50019232895551E-16,-12.975));
#41993=CARTESIAN_POINT('Origin',(0.,0.,-12.1575));
#41994=CARTESIAN_POINT('',(-1.25,-1.53080849893419E-16,-11.365));
#41995=CARTESIAN_POINT('Origin',(0.,0.,-11.365));
#41996=CARTESIAN_POINT('',(-1.25,-1.53080849893419E-16,-12.1575));
#41997=CARTESIAN_POINT('Origin',(1.195,0.,-11.365));
#41998=CARTESIAN_POINT('',(-1.195,-1.46345292498109E-16,-11.365));
#41999=CARTESIAN_POINT('Origin',(0.,0.,-11.365));
#42000=CARTESIAN_POINT('Origin',(0.,0.,-11.3));
#42001=CARTESIAN_POINT('',(-1.195,-1.46345292498109E-16,-11.235));
#42002=CARTESIAN_POINT('Origin',(0.,0.,-11.235));
#42003=CARTESIAN_POINT('',(-1.195,-1.46345292498109E-16,-11.3));
#42004=CARTESIAN_POINT('Origin',(1.25,0.,-11.235));
#42005=CARTESIAN_POINT('',(-1.25,-1.53080849893419E-16,-11.235));
#42006=CARTESIAN_POINT('Origin',(0.,0.,-11.235));
#42007=CARTESIAN_POINT('Origin',(0.,0.,-3.5525));
#42008=CARTESIAN_POINT('',(-1.25,-1.53080849893419E-16,4.13));
#42009=CARTESIAN_POINT('Origin',(0.,0.,4.13));
#42010=CARTESIAN_POINT('',(-1.25,-1.53080849893419E-16,-3.5525));
#42011=CARTESIAN_POINT('Origin',(1.195,0.,4.13));
#42012=CARTESIAN_POINT('',(-1.195,-1.46345292498109E-16,4.13));
#42013=CARTESIAN_POINT('Origin',(0.,0.,4.13));
#42014=CARTESIAN_POINT('Origin',(0.,0.,4.195));
#42015=CARTESIAN_POINT('',(-1.195,-1.46345292498109E-16,4.26));
#42016=CARTESIAN_POINT('Origin',(0.,0.,4.26));
#42017=CARTESIAN_POINT('',(-1.195,-1.46345292498109E-16,4.195));
#42018=CARTESIAN_POINT('Origin',(1.25,0.,4.26));
#42019=CARTESIAN_POINT('',(-1.25,-1.53080849893419E-16,4.26));
#42020=CARTESIAN_POINT('Origin',(0.,0.,4.26));
#42021=CARTESIAN_POINT('Origin',(0.,0.,4.28));
#42022=CARTESIAN_POINT('',(-1.25,-1.53080849893419E-16,4.3));
#42023=CARTESIAN_POINT('Origin',(0.,0.,4.3));
#42024=CARTESIAN_POINT('',(-1.25,-1.53080849893419E-16,4.28));
#42025=CARTESIAN_POINT('Origin',(0.,0.,4.35));
#42026=CARTESIAN_POINT('',(-1.15,-1.40834381901946E-16,4.4));
#42027=CARTESIAN_POINT('Origin',(0.,0.,4.4));
#42028=CARTESIAN_POINT('',(-1.2,-1.46957615897682E-16,4.35));
#42029=CARTESIAN_POINT('Origin',(0.,0.,4.4));
#42030=CARTESIAN_POINT('',(0.,0.,0.));
#42031=CARTESIAN_POINT('Origin',(3.6,0.,-2.4));
#42032=CARTESIAN_POINT('',(-3.7,-4.53119315684521E-16,-2.4));
#42033=CARTESIAN_POINT('Origin',(0.,0.,-2.4));
#42034=CARTESIAN_POINT('',(-3.6,-4.40872847693047E-16,-2.4));
#42035=CARTESIAN_POINT('Origin',(0.,0.,-2.4));
#42036=CARTESIAN_POINT('Origin',(0.,0.,-2.55));
#42037=CARTESIAN_POINT('',(-3.6,-4.40872847693047E-16,-2.7));
#42038=CARTESIAN_POINT('Origin',(0.,0.,-2.7));
#42039=CARTESIAN_POINT('',(-3.6,-4.40872847693047E-16,-2.55));
#42040=CARTESIAN_POINT('Origin',(3.8,0.,-2.7));
#42041=CARTESIAN_POINT('',(-3.7,4.53119315684521E-16,-2.7));
#42042=CARTESIAN_POINT('Origin',(0.,0.,-2.7));
#42043=CARTESIAN_POINT('Origin',(0.,0.,-2.5425));
#42044=CARTESIAN_POINT('',(-3.7,-4.53119315684521E-16,-5.));
#42045=CARTESIAN_POINT('',(-3.7,-4.53119315684521E-16,-2.5425));
#42046=CARTESIAN_POINT('Origin',(0.,0.,-5.));
#42047=CARTESIAN_POINT('Origin',(1.58,0.402,-2.));
#42048=CARTESIAN_POINT('',(1.18570654042221,0.402,-2.));
#42049=CARTESIAN_POINT('',(1.18570654042221,0.402,-0.00499999999999989));
#42050=CARTESIAN_POINT('',(1.18570654042221,0.402,-1.0025));
#42051=CARTESIAN_POINT('',(1.58,0.402,-2.));
#42052=CARTESIAN_POINT('',(1.64,0.402,-2.));
#42053=CARTESIAN_POINT('',(1.58,0.402,-0.00499999999999989));
#42054=CARTESIAN_POINT('',(1.58,0.402,-2.));
#42055=CARTESIAN_POINT('',(1.416,0.402,-0.005));
#42056=CARTESIAN_POINT('Origin',(1.58,-0.402,-2.));
#42057=CARTESIAN_POINT('',(1.58,-0.402,-0.00499999999999989));
#42058=CARTESIAN_POINT('',(1.58,-0.201,-0.005));
#42059=CARTESIAN_POINT('',(1.58,-0.402,-2.));
#42060=CARTESIAN_POINT('',(1.58,-0.201,-2.));
#42061=CARTESIAN_POINT('',(1.58,-0.402,-2.));
#42062=CARTESIAN_POINT('Origin',(1.1,-0.402,-2.));
#42063=CARTESIAN_POINT('',(1.18570654042221,-0.402,-0.00499999999999989));
#42064=CARTESIAN_POINT('',(1.18570654042221,-0.402,-2.));
#42065=CARTESIAN_POINT('',(1.18570654042221,-0.402,-1.0025));
#42066=CARTESIAN_POINT('',(1.176,-0.402,-0.005));
#42067=CARTESIAN_POINT('',(1.4,-0.402,-2.));
#42068=CARTESIAN_POINT('Origin',(1.7,0.,-2.));
#42069=CARTESIAN_POINT('',(-1.7,-2.0818995585505E-16,-2.));
#42070=CARTESIAN_POINT('Origin',(0.,0.,-2.));
#42071=CARTESIAN_POINT('Origin',(0.,0.,-2.));
#42072=CARTESIAN_POINT('Origin',(0.451485261934018,-2.56050015783174,-1.2));
#42073=CARTESIAN_POINT('',(0.101485261934018,-2.56050015783174,-1.2));
#42074=CARTESIAN_POINT('Origin',(0.451485261934018,-2.56050015783174,-1.2));
#42075=CARTESIAN_POINT('',(0.101485261934018,-2.56050015783174,-0.00499999999999989));
#42076=CARTESIAN_POINT('',(0.101485261934018,-2.56050015783174,-1.2));
#42077=CARTESIAN_POINT('Origin',(0.451485261934018,-2.56050015783174,-0.00499999999999989));
#42078=CARTESIAN_POINT('Origin',(-2.44320081404336,-0.889252372646739,-1.2));
#42079=CARTESIAN_POINT('',(-2.79320081404336,-0.889252372646739,-1.2));
#42080=CARTESIAN_POINT('Origin',(-2.44320081404336,-0.889252372646739,-1.2));
#42081=CARTESIAN_POINT('',(-2.79320081404336,-0.889252372646739,-0.00499999999999989));
#42082=CARTESIAN_POINT('',(-2.79320081404336,-0.889252372646739,-1.2));
#42083=CARTESIAN_POINT('Origin',(-2.44320081404336,-0.889252372646739,-0.00499999999999989));
#42084=CARTESIAN_POINT('Origin',(-2.44320081404336,0.889252372646739,-1.2));
#42085=CARTESIAN_POINT('',(-2.79320081404336,0.889252372646739,-1.2));
#42086=CARTESIAN_POINT('Origin',(-2.44320081404336,0.889252372646739,-1.2));
#42087=CARTESIAN_POINT('',(-2.79320081404336,0.889252372646739,-0.00499999999999989));
#42088=CARTESIAN_POINT('',(-2.79320081404336,0.889252372646739,-1.2));
#42089=CARTESIAN_POINT('Origin',(-2.44320081404336,0.889252372646739,-0.00499999999999989));
#42090=CARTESIAN_POINT('Origin',(0.451485261934019,2.56050015783174,-1.2));
#42091=CARTESIAN_POINT('',(0.101485261934019,2.56050015783174,-1.2));
#42092=CARTESIAN_POINT('Origin',(0.451485261934019,2.56050015783174,-1.2));
#42093=CARTESIAN_POINT('',(0.101485261934019,2.56050015783174,-0.00499999999999989));
#42094=CARTESIAN_POINT('',(0.101485261934019,2.56050015783174,-1.2));
#42095=CARTESIAN_POINT('Origin',(0.451485261934019,2.56050015783174,-0.00499999999999989));
#42096=CARTESIAN_POINT('Origin',(1.99171555210934,1.671247785185,-1.2));
#42097=CARTESIAN_POINT('',(1.64171555210934,1.671247785185,-1.2));
#42098=CARTESIAN_POINT('Origin',(1.99171555210934,1.671247785185,-1.2));
#42099=CARTESIAN_POINT('',(1.64171555210934,1.671247785185,-0.00499999999999989));
#42100=CARTESIAN_POINT('',(1.64171555210934,1.671247785185,-1.2));
#42101=CARTESIAN_POINT('Origin',(1.99171555210934,1.671247785185,-0.00499999999999989));
#42102=CARTESIAN_POINT('Origin',(-1.3,2.25166604983954,-1.2));
#42103=CARTESIAN_POINT('',(-1.65,2.25166604983954,-1.2));
#42104=CARTESIAN_POINT('Origin',(-1.3,2.25166604983954,-1.2));
#42105=CARTESIAN_POINT('',(-1.65,2.25166604983954,-0.00499999999999989));
#42106=CARTESIAN_POINT('',(-1.65,2.25166604983954,-1.2));
#42107=CARTESIAN_POINT('Origin',(-1.3,2.25166604983954,-0.00499999999999989));
#42108=CARTESIAN_POINT('Origin',(2.6,0.,-1.2));
#42109=CARTESIAN_POINT('',(2.25,-4.28626379701574E-17,-1.2));
#42110=CARTESIAN_POINT('Origin',(2.6,0.,-1.2));
#42111=CARTESIAN_POINT('',(2.25,4.28626379701574E-17,-0.00499999999999989));
#42112=CARTESIAN_POINT('',(2.25,-4.28626379701574E-17,-1.2));
#42113=CARTESIAN_POINT('Origin',(2.6,0.,-0.00499999999999989));
#42114=CARTESIAN_POINT('Origin',(-1.3,-2.25166604983954,-1.2));
#42115=CARTESIAN_POINT('',(-1.65,-2.25166604983954,-1.2));
#42116=CARTESIAN_POINT('Origin',(-1.3,-2.25166604983954,-1.2));
#42117=CARTESIAN_POINT('',(-1.65,-2.25166604983954,-0.00499999999999989));
#42118=CARTESIAN_POINT('',(-1.65,-2.25166604983954,-1.2));
#42119=CARTESIAN_POINT('Origin',(-1.3,-2.25166604983954,-0.00499999999999989));
#42120=CARTESIAN_POINT('Origin',(1.99171555210934,-1.671247785185,-1.2));
#42121=CARTESIAN_POINT('',(1.64171555210934,-1.671247785185,-1.2));
#42122=CARTESIAN_POINT('Origin',(1.99171555210934,-1.671247785185,-1.2));
#42123=CARTESIAN_POINT('',(1.64171555210934,-1.671247785185,-0.00499999999999989));
#42124=CARTESIAN_POINT('',(1.64171555210934,-1.671247785185,-1.2));
#42125=CARTESIAN_POINT('Origin',(1.99171555210934,-1.671247785185,-0.00499999999999989));
#42126=CARTESIAN_POINT('Origin',(0.451485261934018,-2.56050015783174,-5.5));
#42127=CARTESIAN_POINT('',(0.517772072056189,-3.15783344738108,-5.5));
#42128=CARTESIAN_POINT('',(0.593496052911633,-3.14448126646961,-5.5));
#42129=CARTESIAN_POINT('Ctrl Pts',(0.517772072056188,-3.15783344738107,
-5.5));
#42130=CARTESIAN_POINT('Ctrl Pts',(0.530527217850702,-3.15641799315786,
-5.49933297200685));
#42131=CARTESIAN_POINT('Ctrl Pts',(0.543231868402549,-3.15459414946623,
-5.499));
#42132=CARTESIAN_POINT('Ctrl Pts',(0.568463765021136,-3.15014508531793,
-5.499));
#42133=CARTESIAN_POINT('Ctrl Pts',(0.581026022675185,-3.14751369137377,
-5.49933297200685));
#42134=CARTESIAN_POINT('Ctrl Pts',(0.593496052911633,-3.14448126646961,
-5.5));
#42135=CARTESIAN_POINT('',(-0.149514738065982,-2.56050015783174,-5.5));
#42136=CARTESIAN_POINT('Origin',(0.451485261934018,-2.56050015783174,-5.5));
#42137=CARTESIAN_POINT('',(-0.149514738065982,-2.56050015783174,-1.2));
#42138=CARTESIAN_POINT('',(-0.149514738065982,-2.56050015783174,-5.5));
#42139=CARTESIAN_POINT('Origin',(0.451485261934018,-2.56050015783174,-1.2));
#42140=CARTESIAN_POINT('Origin',(0.451485261934018,-2.56050015783174,-5.5));
#42141=CARTESIAN_POINT('Origin',(0.451485261934018,-2.56050015783174,-1.2));
#42142=CARTESIAN_POINT('Origin',(-2.44320081404336,-0.889252372646739,-5.5));
#42143=CARTESIAN_POINT('',(-3.01994868494276,-1.05825797436754,-5.5));
#42144=CARTESIAN_POINT('',(-2.9936500223803,-1.13051295591977,-5.5));
#42145=CARTESIAN_POINT('Ctrl Pts',(-3.01994868494276,-1.05825797436754,
-5.5));
#42146=CARTESIAN_POINT('Ctrl Pts',(-3.01633982682661,-1.07057354979034,
-5.49933297200685));
#42147=CARTESIAN_POINT('Ctrl Pts',(-3.01233755200259,-1.08276848101971,
-5.499));
#42148=CARTESIAN_POINT('Ctrl Pts',(-3.00357460626879,-1.10684447655122,
-5.499));
#42149=CARTESIAN_POINT('Ctrl Pts',(-2.99880177596235,-1.11875894852114,
-5.49933297200685));
#42150=CARTESIAN_POINT('Ctrl Pts',(-2.9936500223803,-1.13051295591977,-5.5));
#42151=CARTESIAN_POINT('',(-3.04420081404336,-0.889252372646739,-5.5));
#42152=CARTESIAN_POINT('Origin',(-2.44320081404336,-0.889252372646739,-5.5));
#42153=CARTESIAN_POINT('',(-3.04420081404336,-0.889252372646739,-1.2));
#42154=CARTESIAN_POINT('',(-3.04420081404336,-0.889252372646739,-5.5));
#42155=CARTESIAN_POINT('Origin',(-2.44320081404336,-0.889252372646739,-1.2));
#42156=CARTESIAN_POINT('Origin',(-2.44320081404336,-0.889252372646739,-5.5));
#42157=CARTESIAN_POINT('Origin',(-2.44320081404336,-0.889252372646739,-1.2));
#42158=CARTESIAN_POINT('Origin',(-2.44320081404336,0.889252372646739,-5.5));
#42159=CARTESIAN_POINT('',(-2.9936500223803,1.13051295591977,-5.5));
#42160=CARTESIAN_POINT('',(-3.01994868494276,1.05825797436754,-5.5));
#42161=CARTESIAN_POINT('Ctrl Pts',(-2.9936500223803,1.13051295591977,-5.5));
#42162=CARTESIAN_POINT('Ctrl Pts',(-2.99880177596235,1.11875894852114,-5.49933297200685));
#42163=CARTESIAN_POINT('Ctrl Pts',(-3.00357460626879,1.10684447655122,-5.499));
#42164=CARTESIAN_POINT('Ctrl Pts',(-3.01233755200259,1.08276848101971,-5.499));
#42165=CARTESIAN_POINT('Ctrl Pts',(-3.01633982682661,1.07057354979034,-5.49933297200685));
#42166=CARTESIAN_POINT('Ctrl Pts',(-3.01994868494276,1.05825797436754,-5.5));
#42167=CARTESIAN_POINT('',(-3.04420081404336,0.889252372646739,-5.5));
#42168=CARTESIAN_POINT('Origin',(-2.44320081404336,0.889252372646739,-5.5));
#42169=CARTESIAN_POINT('',(-3.04420081404336,0.889252372646739,-1.2));
#42170=CARTESIAN_POINT('',(-3.04420081404336,0.889252372646739,-5.5));
#42171=CARTESIAN_POINT('Origin',(-2.44320081404336,0.889252372646739,-1.2));
#42172=CARTESIAN_POINT('Origin',(-2.44320081404336,0.889252372646739,-5.5));
#42173=CARTESIAN_POINT('Origin',(-2.44320081404336,0.889252372646739,-1.2));
#42174=CARTESIAN_POINT('Origin',(0.451485261934019,2.56050015783174,-5.5));
#42175=CARTESIAN_POINT('',(0.593496052911635,3.14448126646961,-5.5));
#42176=CARTESIAN_POINT('',(0.51777207205619,3.15783344738107,-5.5));
#42177=CARTESIAN_POINT('Ctrl Pts',(0.593496052911635,3.14448126646961,-5.5));
#42178=CARTESIAN_POINT('Ctrl Pts',(0.581026022675186,3.14751369137377,-5.49933297200685));
#42179=CARTESIAN_POINT('Ctrl Pts',(0.568463765021138,3.15014508531793,-5.499));
#42180=CARTESIAN_POINT('Ctrl Pts',(0.543231868402551,3.15459414946623,-5.499));
#42181=CARTESIAN_POINT('Ctrl Pts',(0.530527217850703,3.15641799315786,-5.49933297200685));
#42182=CARTESIAN_POINT('Ctrl Pts',(0.51777207205619,3.15783344738107,-5.5));
#42183=CARTESIAN_POINT('',(-0.149514738065981,2.56050015783174,-5.5));
#42184=CARTESIAN_POINT('Origin',(0.451485261934019,2.56050015783174,-5.5));
#42185=CARTESIAN_POINT('',(-0.149514738065981,2.56050015783174,-1.2));
#42186=CARTESIAN_POINT('',(-0.149514738065981,2.56050015783174,-5.5));
#42187=CARTESIAN_POINT('Origin',(0.451485261934019,2.56050015783174,-1.2));
#42188=CARTESIAN_POINT('Origin',(0.451485261934019,2.56050015783174,-5.5));
#42189=CARTESIAN_POINT('Origin',(0.451485261934019,2.56050015783174,-1.2));
#42190=CARTESIAN_POINT('Origin',(1.99171555210934,1.671247785185,-5.5));
#42191=CARTESIAN_POINT('',(2.47587795032411,2.0273204914613,-5.5));
#42192=CARTESIAN_POINT('',(2.42645263203113,2.08622329210207,-5.5));
#42193=CARTESIAN_POINT('Ctrl Pts',(2.47587795032411,2.0273204914613,-5.5));
#42194=CARTESIAN_POINT('Ctrl Pts',(2.46827455811165,2.03765904463672,-5.49933297200685));
#42195=CARTESIAN_POINT('Ctrl Pts',(2.46034273786624,2.04774967291501,-5.499));
#42196=CARTESIAN_POINT('Ctrl Pts',(2.44387378698146,2.06737660429821,-5.499));
#42197=CARTESIAN_POINT('Ctrl Pts',(2.43531380415142,2.07694014158343,-5.49933297200685));
#42198=CARTESIAN_POINT('Ctrl Pts',(2.42645263203113,2.08622329210207,-5.5));
#42199=CARTESIAN_POINT('',(1.39071555210934,1.671247785185,-5.5));
#42200=CARTESIAN_POINT('Origin',(1.99171555210934,1.671247785185,-5.5));
#42201=CARTESIAN_POINT('',(1.39071555210934,1.671247785185,-1.2));
#42202=CARTESIAN_POINT('',(1.39071555210934,1.671247785185,-5.5));
#42203=CARTESIAN_POINT('Origin',(1.99171555210934,1.671247785185,-1.2));
#42204=CARTESIAN_POINT('Origin',(1.99171555210934,1.671247785185,-5.5));
#42205=CARTESIAN_POINT('Origin',(1.99171555210934,1.671247785185,-1.2));
#42206=CARTESIAN_POINT('Origin',(-1.3,2.25166604983954,-5.5));
#42207=CARTESIAN_POINT('',(-1.5665892436321,2.79030430988024,-5.5));
#42208=CARTESIAN_POINT('',(-1.63317979482944,2.75185823722096,-5.5));
#42209=CARTESIAN_POINT('Ctrl Pts',(-1.5665892436321,2.79030430988024,-5.5));
#42210=CARTESIAN_POINT('Ctrl Pts',(-1.57809104615595,2.78461170119884,-5.49933297200685));
#42211=CARTESIAN_POINT('Ctrl Pts',(-1.58940572124837,2.7785526023377,-5.499));
#42212=CARTESIAN_POINT('Ctrl Pts',(-1.61159427875162,2.76574203269027,-5.499));
#42213=CARTESIAN_POINT('Ctrl Pts',(-1.62249894983562,2.75897278605524,-5.49933297200685));
#42214=CARTESIAN_POINT('Ctrl Pts',(-1.63317979482944,2.75185823722096,-5.5));
#42215=CARTESIAN_POINT('',(-1.901,2.25166604983954,-5.5));
#42216=CARTESIAN_POINT('Origin',(-1.3,2.25166604983954,-5.5));
#42217=CARTESIAN_POINT('',(-1.901,2.25166604983954,-1.2));
#42218=CARTESIAN_POINT('',(-1.901,2.25166604983954,-5.5));
#42219=CARTESIAN_POINT('Origin',(-1.3,2.25166604983954,-1.2));
#42220=CARTESIAN_POINT('Origin',(-1.3,2.25166604983954,-5.5));
#42221=CARTESIAN_POINT('Origin',(-1.3,2.25166604983954,-1.2));
#42222=CARTESIAN_POINT('Origin',(2.6,0.,-5.5));
#42223=CARTESIAN_POINT('',(3.19976903846154,-0.0384460726592727,-5.5));
#42224=CARTESIAN_POINT('',(3.19976903846154,0.0384460726592727,-5.5));
#42225=CARTESIAN_POINT('Ctrl Pts',(3.19976903846154,-0.0384460726592726,
-5.5));
#42226=CARTESIAN_POINT('Ctrl Pts',(3.20058999599157,-0.0256389151436019,
-5.49933297200685));
#42227=CARTESIAN_POINT('Ctrl Pts',(3.201,-0.0128105696474314,-5.499));
#42228=CARTESIAN_POINT('Ctrl Pts',(3.201,0.0128105696474314,-5.499));
#42229=CARTESIAN_POINT('Ctrl Pts',(3.20058999599157,0.0256389151436019,
-5.49933297200685));
#42230=CARTESIAN_POINT('Ctrl Pts',(3.19976903846154,0.0384460726592726,
-5.5));
#42231=CARTESIAN_POINT('',(1.999,-7.36012726287559E-17,-5.5));
#42232=CARTESIAN_POINT('Origin',(2.6,0.,-5.5));
#42233=CARTESIAN_POINT('',(1.999,-7.36012726287559E-17,-1.2));
#42234=CARTESIAN_POINT('',(1.999,-7.36012726287559E-17,-5.5));
#42235=CARTESIAN_POINT('Origin',(2.6,0.,-1.2));
#42236=CARTESIAN_POINT('Origin',(2.6,0.,-5.5));
#42237=CARTESIAN_POINT('Origin',(2.6,0.,-1.2));
#42238=CARTESIAN_POINT('Origin',(-1.3,-2.25166604983954,-5.5));
#42239=CARTESIAN_POINT('',(-1.63317979482944,-2.75185823722096,-5.5));
#42240=CARTESIAN_POINT('',(-1.5665892436321,-2.79030430988023,-5.5));
#42241=CARTESIAN_POINT('Ctrl Pts',(-1.63317979482944,-2.75185823722096,
-5.5));
#42242=CARTESIAN_POINT('Ctrl Pts',(-1.62249894983562,-2.75897278605523,
-5.49933297200685));
#42243=CARTESIAN_POINT('Ctrl Pts',(-1.61159427875163,-2.76574203269027,
-5.499));
#42244=CARTESIAN_POINT('Ctrl Pts',(-1.58940572124838,-2.7785526023377,-5.499));
#42245=CARTESIAN_POINT('Ctrl Pts',(-1.57809104615595,-2.78461170119884,
-5.49933297200685));
#42246=CARTESIAN_POINT('Ctrl Pts',(-1.5665892436321,-2.79030430988023,-5.5));
#42247=CARTESIAN_POINT('',(-1.901,-2.25166604983954,-5.5));
#42248=CARTESIAN_POINT('Origin',(-1.3,-2.25166604983954,-5.5));
#42249=CARTESIAN_POINT('',(-1.901,-2.25166604983954,-1.2));
#42250=CARTESIAN_POINT('',(-1.901,-2.25166604983954,-5.5));
#42251=CARTESIAN_POINT('Origin',(-1.3,-2.25166604983954,-1.2));
#42252=CARTESIAN_POINT('Origin',(-1.3,-2.25166604983954,-5.5));
#42253=CARTESIAN_POINT('Origin',(-1.3,-2.25166604983954,-1.2));
#42254=CARTESIAN_POINT('Origin',(1.99171555210934,-1.671247785185,-5.5));
#42255=CARTESIAN_POINT('',(2.42645263203113,-2.08622329210207,-5.5));
#42256=CARTESIAN_POINT('',(2.47587795032411,-2.02732049146131,-5.5));
#42257=CARTESIAN_POINT('Ctrl Pts',(2.42645263203113,-2.08622329210207,-5.5));
#42258=CARTESIAN_POINT('Ctrl Pts',(2.43531380415142,-2.07694014158343,-5.49933297200685));
#42259=CARTESIAN_POINT('Ctrl Pts',(2.44387378698145,-2.06737660429822,-5.499));
#42260=CARTESIAN_POINT('Ctrl Pts',(2.46034273786624,-2.04774967291501,-5.499));
#42261=CARTESIAN_POINT('Ctrl Pts',(2.46827455811165,-2.03765904463672,-5.49933297200685));
#42262=CARTESIAN_POINT('Ctrl Pts',(2.4758779503241,-2.02732049146131,-5.5));
#42263=CARTESIAN_POINT('',(1.39071555210934,-1.671247785185,-5.5));
#42264=CARTESIAN_POINT('Origin',(1.99171555210934,-1.671247785185,-5.5));
#42265=CARTESIAN_POINT('',(1.39071555210934,-1.671247785185,-1.2));
#42266=CARTESIAN_POINT('',(1.39071555210934,-1.671247785185,-5.5));
#42267=CARTESIAN_POINT('Origin',(1.99171555210934,-1.671247785185,-1.2));
#42268=CARTESIAN_POINT('Origin',(1.99171555210934,-1.671247785185,-5.5));
#42269=CARTESIAN_POINT('Origin',(1.99171555210934,-1.671247785185,-1.2));
#42270=CARTESIAN_POINT('Origin',(3.2,0.,-5.5));
#42271=CARTESIAN_POINT('Origin',(0.,0.,-5.5));
#42272=CARTESIAN_POINT('Origin',(0.,0.,-5.5));
#42273=CARTESIAN_POINT('',(-3.2,-3.91886975727153E-16,-5.5));
#42274=CARTESIAN_POINT('Origin',(0.,0.,-5.5));
#42275=CARTESIAN_POINT('Origin',(0.,0.,-5.5));
#42276=CARTESIAN_POINT('Origin',(0.,0.,-5.5));
#42277=CARTESIAN_POINT('Origin',(0.,0.,-5.5));
#42278=CARTESIAN_POINT('Origin',(0.,0.,-5.5));
#42279=CARTESIAN_POINT('Origin',(0.,0.,-5.5));
#42280=CARTESIAN_POINT('Origin',(0.,0.,-5.5));
#42281=CARTESIAN_POINT('Origin',(0.,0.,-5.5));
#42282=CARTESIAN_POINT('',(-1.76,-2.15537836649934E-16,-5.5));
#42283=CARTESIAN_POINT('Origin',(0.,0.,-5.5));
#42284=CARTESIAN_POINT('Origin',(0.,0.,-3.72));
#42285=CARTESIAN_POINT('',(-1.7,-2.0818995585505E-16,-5.44));
#42286=CARTESIAN_POINT('',(-1.7,-2.0818995585505E-16,-3.72));
#42287=CARTESIAN_POINT('Origin',(0.,0.,-5.44));
#42288=CARTESIAN_POINT('Origin',(0.,0.,-5.47));
#42289=CARTESIAN_POINT('',(-1.73,-2.11863896252492E-16,-5.47));
#42290=CARTESIAN_POINT('Origin',(0.,0.,-5.25));
#42291=CARTESIAN_POINT('',(-3.45,-4.22503145705837E-16,-5.25));
#42292=CARTESIAN_POINT('Origin',(0.,0.,-2.5425));
#42293=CARTESIAN_POINT('',(-3.7,-4.53119315684521E-16,-0.085));
#42294=CARTESIAN_POINT('Origin',(0.,0.,-0.085));
#42295=CARTESIAN_POINT('',(-3.7,-4.53119315684521E-16,-2.5425));
#42296=CARTESIAN_POINT('Origin',(0.,0.,-0.0449999999999999));
#42297=CARTESIAN_POINT('',(-3.62,-4.43322141291342E-16,-0.00499999999999991));
#42298=CARTESIAN_POINT('Origin',(0.,0.,-0.00499999999999989));
#42299=CARTESIAN_POINT('',(-3.66,-4.48220728487931E-16,-0.0449999999999999));
#42300=CARTESIAN_POINT('Origin',(1.252,0.,-0.005));
#42301=CARTESIAN_POINT('Origin',(0.,0.,-0.00499999999999989));
#42302=CARTESIAN_POINT('Origin',(0.,0.,-1.0025));
#42303=CARTESIAN_POINT('',(0.,0.,0.));
#42304=CARTESIAN_POINT('Origin',(2.16374675043084,2.16374675043084,-12.4));
#42305=CARTESIAN_POINT('',(2.16374675043084,2.16374675043084,-12.4));
#42306=CARTESIAN_POINT('',(2.00818325856979,2.00818325856979,-12.4));
#42307=CARTESIAN_POINT('',(1.85687337521542,1.85687337521542,-12.4));
#42308=CARTESIAN_POINT('',(2.16374675043084,2.16374675043084,-12.36));
#42309=CARTESIAN_POINT('',(2.16374675043084,2.16374675043084,-12.4));
#42310=CARTESIAN_POINT('',(2.00818325856979,2.00818325856979,-12.36));
#42311=CARTESIAN_POINT('',(2.00818325856979,2.00818325856979,-12.36));
#42312=CARTESIAN_POINT('',(2.00818325856979,2.00818325856979,-12.4));
#42313=CARTESIAN_POINT('Origin',(2.33826859021798,1.35,-12.4));
#42314=CARTESIAN_POINT('',(2.33826859021798,1.35,-12.4));
#42315=CARTESIAN_POINT('',(2.49341599027072,0.62659086802724,-12.4));
#42316=CARTESIAN_POINT('',(2.33826859021798,1.35,-12.36));
#42317=CARTESIAN_POINT('',(2.33826859021798,1.35,-12.4));
#42318=CARTESIAN_POINT('',(2.16374675043084,2.16374675043084,-12.36));
#42319=CARTESIAN_POINT('Origin',(1.65462986797652,1.65462986797652,-12.4));
#42320=CARTESIAN_POINT('',(1.65462986797652,1.65462986797652,-12.4));
#42321=CARTESIAN_POINT('',(2.56517017788785,1.2488925020676,-12.4));
#42322=CARTESIAN_POINT('',(1.65462986797652,1.65462986797652,-12.36));
#42323=CARTESIAN_POINT('',(1.65462986797652,1.65462986797652,-12.4));
#42324=CARTESIAN_POINT('',(2.33826859021798,1.35,-12.36));
#42325=CARTESIAN_POINT('Origin',(1.81019335983756,1.81019335983756,-12.4));
#42326=CARTESIAN_POINT('',(1.81019335983756,1.81019335983756,-12.4));
#42327=CARTESIAN_POINT('',(1.68009667991878,1.68009667991878,-12.4));
#42328=CARTESIAN_POINT('',(1.81019335983756,1.81019335983756,-12.36));
#42329=CARTESIAN_POINT('',(1.81019335983756,1.81019335983756,-12.4));
#42330=CARTESIAN_POINT('',(1.65462986797652,1.65462986797652,-12.36));
#42331=CARTESIAN_POINT('Origin',(0.,-8.88178419700125E-16,-12.4));
#42332=CARTESIAN_POINT('',(-1.81019335983756,1.81019335983756,-12.4));
#42333=CARTESIAN_POINT('Origin',(0.,-8.88178419700125E-16,-12.4));
#42334=CARTESIAN_POINT('',(-1.81019335983756,1.81019335983756,-12.36));
#42335=CARTESIAN_POINT('',(-1.81019335983756,1.81019335983756,-12.4));
#42336=CARTESIAN_POINT('Origin',(0.,-8.88178419700125E-16,-12.36));
#42337=CARTESIAN_POINT('Origin',(-2.00818325856979,2.00818325856979,-12.4));
#42338=CARTESIAN_POINT('',(-2.00818325856979,2.00818325856979,-12.4));
#42339=CARTESIAN_POINT('',(-0.229091629284896,0.229091629284898,-12.4));
#42340=CARTESIAN_POINT('',(-2.00818325856979,2.00818325856979,-12.36));
#42341=CARTESIAN_POINT('',(-2.00818325856979,2.00818325856979,-12.4));
#42342=CARTESIAN_POINT('',(-1.81019335983756,1.81019335983756,-12.36));
#42343=CARTESIAN_POINT('Origin',(2.22044604925031E-16,4.44089209850063E-16,
-12.4));
#42344=CARTESIAN_POINT('Origin',(2.22044604925031E-16,4.44089209850063E-16,
-12.4));
#42345=CARTESIAN_POINT('Origin',(2.22044604925031E-16,4.44089209850063E-16,
-12.36));
#42346=CARTESIAN_POINT('Origin',(0.165042665824095,2.095,-12.36));
#42347=CARTESIAN_POINT('Origin',(6.,0.,-0.5275));
#42348=CARTESIAN_POINT('',(6.475,-5.81707229594993E-17,-0.54));
#42349=CARTESIAN_POINT('Origin',(6.,0.,-0.54));
#42350=CARTESIAN_POINT('',(6.45,5.51091059616309E-17,-0.515));
#42351=CARTESIAN_POINT('',(6.4625,-5.66399144605651E-17,-0.5275));
#42352=CARTESIAN_POINT('',(5.55,-5.51091059616309E-17,-0.515));
#42353=CARTESIAN_POINT('Origin',(6.,0.,-0.515));
#42354=CARTESIAN_POINT('Origin',(6.,0.,-0.515));
#42355=CARTESIAN_POINT('Origin',(6.45,0.,-0.54));
#42356=CARTESIAN_POINT('',(5.3,-8.57252759403147E-17,-0.54));
#42357=CARTESIAN_POINT('Origin',(6.,0.,-0.54));
#42358=CARTESIAN_POINT('Origin',(6.,0.,-0.22));
#42359=CARTESIAN_POINT('',(5.55,5.51091059616309E-17,0.));
#42360=CARTESIAN_POINT('',(5.55,-5.51091059616309E-17,-0.22));
#42361=CARTESIAN_POINT('Origin',(6.,0.,0.));
#42362=CARTESIAN_POINT('Origin',(3.,5.19615242270663,-0.5275));
#42363=CARTESIAN_POINT('',(3.475,5.19615242270663,-0.54));
#42364=CARTESIAN_POINT('Origin',(3.,5.19615242270663,-0.54));
#42365=CARTESIAN_POINT('',(3.45,5.19615242270663,-0.515));
#42366=CARTESIAN_POINT('',(3.4625,5.19615242270663,-0.5275));
#42367=CARTESIAN_POINT('',(2.55,5.19615242270663,-0.515));
#42368=CARTESIAN_POINT('Origin',(3.,5.19615242270663,-0.515));
#42369=CARTESIAN_POINT('Origin',(3.,5.19615242270663,-0.515));
#42370=CARTESIAN_POINT('Origin',(3.45,5.19615242270663,-0.54));
#42371=CARTESIAN_POINT('',(2.3,5.19615242270663,-0.54));
#42372=CARTESIAN_POINT('Origin',(3.,5.19615242270663,-0.54));
#42373=CARTESIAN_POINT('Origin',(3.,5.19615242270663,-0.22));
#42374=CARTESIAN_POINT('',(2.55,5.19615242270663,0.));
#42375=CARTESIAN_POINT('',(2.55,5.19615242270663,-0.22));
#42376=CARTESIAN_POINT('Origin',(3.,5.19615242270663,0.));
#42377=CARTESIAN_POINT('Origin',(-3.,5.19615242270663,-0.5275));
#42378=CARTESIAN_POINT('',(-2.525,5.19615242270663,-0.54));
#42379=CARTESIAN_POINT('Origin',(-3.,5.19615242270663,-0.54));
#42380=CARTESIAN_POINT('',(-2.55,5.19615242270663,-0.515));
#42381=CARTESIAN_POINT('',(-2.5375,5.19615242270663,-0.5275));
#42382=CARTESIAN_POINT('',(-3.45,5.19615242270663,-0.515));
#42383=CARTESIAN_POINT('Origin',(-3.,5.19615242270663,-0.515));
#42384=CARTESIAN_POINT('Origin',(-3.,5.19615242270663,-0.515));
#42385=CARTESIAN_POINT('Origin',(-2.55,5.19615242270663,-0.54));
#42386=CARTESIAN_POINT('',(-3.7,5.19615242270663,-0.54));
#42387=CARTESIAN_POINT('Origin',(-3.,5.19615242270663,-0.54));
#42388=CARTESIAN_POINT('Origin',(-3.,5.19615242270663,-0.22));
#42389=CARTESIAN_POINT('',(-3.45,5.19615242270663,0.));
#42390=CARTESIAN_POINT('',(-3.45,5.19615242270663,-0.22));
#42391=CARTESIAN_POINT('Origin',(-3.,5.19615242270663,0.));
#42392=CARTESIAN_POINT('Origin',(-6.,7.34788079488412E-16,-0.5275));
#42393=CARTESIAN_POINT('',(-5.525,6.76617356528913E-16,-0.54));
#42394=CARTESIAN_POINT('Origin',(-6.,7.34788079488412E-16,-0.54));
#42395=CARTESIAN_POINT('',(-5.55,7.89897185450043E-16,-0.515));
#42396=CARTESIAN_POINT('',(-5.5375,6.78148165027847E-16,-0.5275));
#42397=CARTESIAN_POINT('',(-6.45,6.79678973526781E-16,-0.515));
#42398=CARTESIAN_POINT('Origin',(-6.,7.34788079488412E-16,-0.515));
#42399=CARTESIAN_POINT('Origin',(-6.,7.34788079488412E-16,-0.515));
#42400=CARTESIAN_POINT('Origin',(-5.55,7.34788079488412E-16,-0.54));
#42401=CARTESIAN_POINT('',(-6.7,6.49062803548097E-16,-0.54));
#42402=CARTESIAN_POINT('Origin',(-6.,7.34788079488412E-16,-0.54));
#42403=CARTESIAN_POINT('Origin',(-6.,7.34788079488412E-16,-0.22));
#42404=CARTESIAN_POINT('',(-6.45,7.89897185450043E-16,0.));
#42405=CARTESIAN_POINT('',(-6.45,6.79678973526781E-16,-0.22));
#42406=CARTESIAN_POINT('Origin',(-6.,7.34788079488412E-16,0.));
#42407=CARTESIAN_POINT('Origin',(-3.,-5.19615242270663,-0.5275));
#42408=CARTESIAN_POINT('',(-2.525,-5.19615242270663,-0.54));
#42409=CARTESIAN_POINT('Origin',(-3.,-5.19615242270663,-0.54));
#42410=CARTESIAN_POINT('',(-2.55,-5.19615242270663,-0.515));
#42411=CARTESIAN_POINT('',(-2.5375,-5.19615242270663,-0.5275));
#42412=CARTESIAN_POINT('',(-3.45,-5.19615242270663,-0.515));
#42413=CARTESIAN_POINT('Origin',(-3.,-5.19615242270663,-0.515));
#42414=CARTESIAN_POINT('Origin',(-3.,-5.19615242270663,-0.515));
#42415=CARTESIAN_POINT('Origin',(-2.55,-5.19615242270663,-0.54));
#42416=CARTESIAN_POINT('',(-3.7,-5.19615242270663,-0.54));
#42417=CARTESIAN_POINT('Origin',(-3.,-5.19615242270663,-0.54));
#42418=CARTESIAN_POINT('Origin',(-3.,-5.19615242270663,-0.22));
#42419=CARTESIAN_POINT('',(-3.45,-5.19615242270663,0.));
#42420=CARTESIAN_POINT('',(-3.45,-5.19615242270663,-0.22));
#42421=CARTESIAN_POINT('Origin',(-3.,-5.19615242270663,0.));
#42422=CARTESIAN_POINT('Origin',(3.,-5.19615242270663,-0.5275));
#42423=CARTESIAN_POINT('',(3.475,-5.19615242270663,-0.54));
#42424=CARTESIAN_POINT('Origin',(3.,-5.19615242270663,-0.54));
#42425=CARTESIAN_POINT('',(3.45,-5.19615242270663,-0.515));
#42426=CARTESIAN_POINT('',(3.4625,-5.19615242270663,-0.5275));
#42427=CARTESIAN_POINT('',(2.55,-5.19615242270663,-0.515));
#42428=CARTESIAN_POINT('Origin',(3.,-5.19615242270663,-0.515));
#42429=CARTESIAN_POINT('Origin',(3.,-5.19615242270663,-0.515));
#42430=CARTESIAN_POINT('Origin',(3.45,-5.19615242270663,-0.54));
#42431=CARTESIAN_POINT('',(2.3,-5.19615242270663,-0.54));
#42432=CARTESIAN_POINT('Origin',(3.,-5.19615242270663,-0.54));
#42433=CARTESIAN_POINT('Origin',(3.,-5.19615242270663,-0.22));
#42434=CARTESIAN_POINT('',(2.55,-5.19615242270663,0.));
#42435=CARTESIAN_POINT('',(2.55,-5.19615242270663,-0.22));
#42436=CARTESIAN_POINT('Origin',(3.,-5.19615242270663,0.));
#42437=CARTESIAN_POINT('Origin',(3.,-5.19615242270663,-0.985));
#42438=CARTESIAN_POINT('',(2.398505676009,-4.83809575371888,-1.4));
#42439=CARTESIAN_POINT('',(2.3,-5.19615242270663,-1.4));
#42440=CARTESIAN_POINT('Origin',(3.,-5.19615242270663,-1.4));
#42441=CARTESIAN_POINT('',(2.99066099065767,-4.4962147234044,-1.4));
#42442=CARTESIAN_POINT('Ctrl Pts',(2.99066099065767,-4.4962147234044,-1.4));
#42443=CARTESIAN_POINT('Ctrl Pts',(2.94435268993459,-4.49683259790025,-1.4));
#42444=CARTESIAN_POINT('Ctrl Pts',(2.89813146126322,-4.50204848216744,-1.40231938147182));
#42445=CARTESIAN_POINT('Ctrl Pts',(2.81323479915933,-4.52031941214783,-1.40701255737455));
#42446=CARTESIAN_POINT('Ctrl Pts',(2.77447068348404,-4.53224035984442,-1.40932756283484));
#42447=CARTESIAN_POINT('Ctrl Pts',(2.71745752705182,-4.55536347077066,-1.41160495505446));
#42448=CARTESIAN_POINT('Ctrl Pts',(2.6983740351221,-4.56412140103041,-1.41217031646736));
#42449=CARTESIAN_POINT('Ctrl Pts',(2.66481875075551,-4.5813895902509,-1.41269782155031));
#42450=CARTESIAN_POINT('Ctrl Pts',(2.65023281412281,-4.58956955455007,-1.41275985502411));
#42451=CARTESIAN_POINT('Ctrl Pts',(2.6199950909463,-4.60798156330058,-1.41251886218627));
#42452=CARTESIAN_POINT('Ctrl Pts',(2.6044553894058,-4.61831783859573,-1.41217237294443));
#42453=CARTESIAN_POINT('Ctrl Pts',(2.5646618286732,-4.64714483808501,-1.41075856218782));
#42454=CARTESIAN_POINT('Ctrl Pts',(2.54121423306641,-4.66658595835824,-1.40936726373267));
#42455=CARTESIAN_POINT('Ctrl Pts',(2.47069726020893,-4.73325103677911,-1.40429573999265));
#42456=CARTESIAN_POINT('Ctrl Pts',(2.43054124554308,-4.78427965445435,-1.4));
#42457=CARTESIAN_POINT('Ctrl Pts',(2.398505676009,-4.83809575371887,-1.4));
#42458=CARTESIAN_POINT('Origin',(3.,-5.19615242270663,-1.4));
#42459=CARTESIAN_POINT('',(2.3,-5.19615242270663,-0.985));
#42460=CARTESIAN_POINT('Origin',(0.,0.,-1.8));
#42461=CARTESIAN_POINT('',(-5.,-6.12323399573677E-16,-1.8));
#42462=CARTESIAN_POINT('Origin',(0.,0.,-1.8));
#42463=CARTESIAN_POINT('',(-5.3,-6.34179542235909E-16,-1.41270166537926));
#42464=CARTESIAN_POINT('Origin',(-5.4,-6.61309271539571E-16,-1.8));
#42465=CARTESIAN_POINT('',(-5.38916666666667,0.341881030314489,-1.4));
#42466=CARTESIAN_POINT('Ctrl Pts',(-5.3,-6.09688915147857E-16,-1.41270166537926));
#42467=CARTESIAN_POINT('Ctrl Pts',(-5.3,0.00489840697065965,-1.41270166537926));
#42468=CARTESIAN_POINT('Ctrl Pts',(-5.30005141287727,0.00979759623850979,
-1.41268662310038));
#42469=CARTESIAN_POINT('Ctrl Pts',(-5.30057443545454,0.0347025480229719,
-1.41253403311749));
#42470=CARTESIAN_POINT('Ctrl Pts',(-5.30185082372053,0.0546596314022927,
-1.41215873854401));
#42471=CARTESIAN_POINT('Ctrl Pts',(-5.30735883827001,0.106087707237653,
-1.41062705709453));
#42472=CARTESIAN_POINT('Ctrl Pts',(-5.3128706815181,0.137315022342647,-1.40913458836236));
#42473=CARTESIAN_POINT('Ctrl Pts',(-5.33593994566315,0.230600777255617,
-1.4040421544805));
#42474=CARTESIAN_POINT('Ctrl Pts',(-5.35950446427729,0.288884050801338,
-1.4));
#42475=CARTESIAN_POINT('Ctrl Pts',(-5.38916666666667,0.341881030314486,
-1.4));
#42476=CARTESIAN_POINT('',(-2.99066099065768,4.49621472340439,-1.4));
#42477=CARTESIAN_POINT('Origin',(0.,0.,-1.4));
#42478=CARTESIAN_POINT('',(-2.39850567600899,4.83809575371888,-1.4));
#42479=CARTESIAN_POINT('Ctrl Pts',(-2.99066099065768,4.4962147234044,-1.4));
#42480=CARTESIAN_POINT('Ctrl Pts',(-2.9443526899346,4.49683259790024,-1.4));
#42481=CARTESIAN_POINT('Ctrl Pts',(-2.89813146126323,4.50204848216743,-1.40231938147182));
#42482=CARTESIAN_POINT('Ctrl Pts',(-2.81323479915932,4.52031941214783,-1.40701255737455));
#42483=CARTESIAN_POINT('Ctrl Pts',(-2.77447068348403,4.53224035984442,-1.40932756283484));
#42484=CARTESIAN_POINT('Ctrl Pts',(-2.71745752705178,4.55536347077068,-1.41160495505446));
#42485=CARTESIAN_POINT('Ctrl Pts',(-2.69837403512208,4.56412140103042,-1.41217031646737));
#42486=CARTESIAN_POINT('Ctrl Pts',(-2.66481875075553,4.58138959025089,-1.41269782155031));
#42487=CARTESIAN_POINT('Ctrl Pts',(-2.65023281412282,4.58956955455007,-1.41275985502411));
#42488=CARTESIAN_POINT('Ctrl Pts',(-2.61999509094628,4.60798156330059,-1.41251886218627));
#42489=CARTESIAN_POINT('Ctrl Pts',(-2.60445538940576,4.61831783859576,-1.41217237294442));
#42490=CARTESIAN_POINT('Ctrl Pts',(-2.56466182867321,4.64714483808501,-1.41075856218782));
#42491=CARTESIAN_POINT('Ctrl Pts',(-2.54121423306642,4.66658595835823,-1.40936726373267));
#42492=CARTESIAN_POINT('Ctrl Pts',(-2.47069726020893,4.73325103677911,-1.40429573999265));
#42493=CARTESIAN_POINT('Ctrl Pts',(-2.43054124554308,4.78427965445436,-1.4));
#42494=CARTESIAN_POINT('Ctrl Pts',(-2.39850567600899,4.83809575371888,-1.4));
#42495=CARTESIAN_POINT('',(2.398505676009,4.83809575371888,-1.4));
#42496=CARTESIAN_POINT('Origin',(0.,0.,-1.4));
#42497=CARTESIAN_POINT('',(2.99066099065767,4.4962147234044,-1.4));
#42498=CARTESIAN_POINT('Ctrl Pts',(2.398505676009,4.83809575371888,-1.4));
#42499=CARTESIAN_POINT('Ctrl Pts',(2.42219492138029,4.79830052613452,-1.4));
#42500=CARTESIAN_POINT('Ctrl Pts',(2.44982262399457,4.76087971004458,-1.40231938147182));
#42501=CARTESIAN_POINT('Ctrl Pts',(2.5080940445603,4.69649250895631,-1.40701255737455));
#42502=CARTESIAN_POINT('Ctrl Pts',(2.53779994594037,4.66888227387456,-1.40932756283484));
#42503=CARTESIAN_POINT('Ctrl Pts',(2.58633172563316,4.63106898751742,-1.41160495505446));
#42504=CARTESIAN_POINT('Ctrl Pts',(2.60345806168753,4.61892116384326,-1.41217031646736));
#42505=CARTESIAN_POINT('Ctrl Pts',(2.63519039441309,4.59849552976084,-1.41269782155031));
#42506=CARTESIAN_POINT('Ctrl Pts',(2.64956741961458,4.58995372024851,-1.41275985502411));
#42507=CARTESIAN_POINT('Ctrl Pts',(2.6806315485155,4.5729730882003,-1.41251886218627));
#42508=CARTESIAN_POINT('Ctrl Pts',(2.69735287627189,4.56468344954656,-1.41217237294442));
#42509=CARTESIAN_POINT('Ctrl Pts',(2.74221457051073,4.54463471478976,-1.41075856218782));
#42510=CARTESIAN_POINT('Ctrl Pts',(2.77077487234875,4.53404906147323,-1.40936726373267));
#42511=CARTESIAN_POINT('Ctrl Pts',(2.86376701023529,4.5063121107911,-1.40429573999265));
#42512=CARTESIAN_POINT('Ctrl Pts',(2.92803709679497,4.49705029081335,-1.4));
#42513=CARTESIAN_POINT('Ctrl Pts',(2.99066099065767,4.4962147234044,-1.4));
#42514=CARTESIAN_POINT('',(5.38916666666667,0.341881030314488,-1.4));
#42515=CARTESIAN_POINT('Origin',(0.,0.,-1.4));
#42516=CARTESIAN_POINT('',(5.3,-7.14855753237747E-17,-1.41270166537926));
#42517=CARTESIAN_POINT('Ctrl Pts',(5.38916666666667,0.341881030314486,-1.4));
#42518=CARTESIAN_POINT('Ctrl Pts',(5.37147004253223,0.310262756850054,-1.4));
#42519=CARTESIAN_POINT('Ctrl Pts',(5.35620231261546,0.277219041062471,-1.40143366869053));
#42520=CARTESIAN_POINT('Ctrl Pts',(5.32761567846875,0.200017956511915,-1.40554873470576));
#42521=CARTESIAN_POINT('Ctrl Pts',(5.31589717989396,0.155336805463026,-1.40841107882748));
#42522=CARTESIAN_POINT('Ctrl Pts',(5.30499765049498,0.086708007070014,-1.4112618373153));
#42523=CARTESIAN_POINT('Ctrl Pts',(5.30248948591046,0.0634567556288577,
-1.41198187968474));
#42524=CARTESIAN_POINT('Ctrl Pts',(5.300382961066,0.0267381544766715,-1.41258893738177));
#42525=CARTESIAN_POINT('Ctrl Pts',(5.3,0.0133719921338023,-1.41270166537926));
#42526=CARTESIAN_POINT('Ctrl Pts',(5.3,-4.5102810375397E-17,-1.41270166537926));
#42527=CARTESIAN_POINT('',(5.38916666666667,-0.341881030314488,-1.4));
#42528=CARTESIAN_POINT('Ctrl Pts',(5.3,-4.60309413329061E-17,-1.41270166537926));
#42529=CARTESIAN_POINT('Ctrl Pts',(5.3,-0.00489840697065912,-1.41270166537926));
#42530=CARTESIAN_POINT('Ctrl Pts',(5.30005141287727,-0.00979759623850861,
-1.41268662310038));
#42531=CARTESIAN_POINT('Ctrl Pts',(5.30057443545454,-0.0347025480229614,
-1.41253403311749));
#42532=CARTESIAN_POINT('Ctrl Pts',(5.30185082372053,-0.0546596314022734,
-1.41215873854401));
#42533=CARTESIAN_POINT('Ctrl Pts',(5.30735883827001,-0.10608770723766,-1.41062705709453));
#42534=CARTESIAN_POINT('Ctrl Pts',(5.31287068151811,-0.137315022342663,
-1.40913458836236));
#42535=CARTESIAN_POINT('Ctrl Pts',(5.33593994566315,-0.230600777255612,
-1.4040421544805));
#42536=CARTESIAN_POINT('Ctrl Pts',(5.35950446427729,-0.288884050801334,
-1.4));
#42537=CARTESIAN_POINT('Ctrl Pts',(5.38916666666667,-0.341881030314486,
-1.4));
#42538=CARTESIAN_POINT('Origin',(0.,0.,-1.4));
#42539=CARTESIAN_POINT('',(-2.398505676009,-4.83809575371888,-1.4));
#42540=CARTESIAN_POINT('Origin',(0.,0.,-1.4));
#42541=CARTESIAN_POINT('',(-2.99066099065767,-4.4962147234044,-1.4));
#42542=CARTESIAN_POINT('Ctrl Pts',(-2.398505676009,-4.83809575371888,-1.4));
#42543=CARTESIAN_POINT('Ctrl Pts',(-2.4221949213803,-4.79830052613452,-1.4));
#42544=CARTESIAN_POINT('Ctrl Pts',(-2.44982262399457,-4.76087971004458,
-1.40231938147182));
#42545=CARTESIAN_POINT('Ctrl Pts',(-2.5080940445603,-4.6964925089563,-1.40701255737455));
#42546=CARTESIAN_POINT('Ctrl Pts',(-2.53779994594038,-4.66888227387456,
-1.40932756283484));
#42547=CARTESIAN_POINT('Ctrl Pts',(-2.58633172563316,-4.63106898751742,
-1.41160495505446));
#42548=CARTESIAN_POINT('Ctrl Pts',(-2.60345806168753,-4.61892116384326,
-1.41217031646736));
#42549=CARTESIAN_POINT('Ctrl Pts',(-2.6351903944131,-4.59849552976084,-1.41269782155031));
#42550=CARTESIAN_POINT('Ctrl Pts',(-2.64956741961458,-4.58995372024851,
-1.41275985502411));
#42551=CARTESIAN_POINT('Ctrl Pts',(-2.6806315485155,-4.5729730882003,-1.41251886218627));
#42552=CARTESIAN_POINT('Ctrl Pts',(-2.69735287627188,-4.56468344954657,
-1.41217237294442));
#42553=CARTESIAN_POINT('Ctrl Pts',(-2.74221457051074,-4.54463471478975,
-1.41075856218782));
#42554=CARTESIAN_POINT('Ctrl Pts',(-2.77077487234877,-4.53404906147323,
-1.40936726373267));
#42555=CARTESIAN_POINT('Ctrl Pts',(-2.86376701023528,-4.5063121107911,-1.40429573999265));
#42556=CARTESIAN_POINT('Ctrl Pts',(-2.92803709679497,-4.49705029081335,
-1.4));
#42557=CARTESIAN_POINT('Ctrl Pts',(-2.99066099065767,-4.4962147234044,-1.4));
#42558=CARTESIAN_POINT('',(-5.38916666666667,-0.341881030314487,-1.4));
#42559=CARTESIAN_POINT('Origin',(0.,0.,-1.4));
#42560=CARTESIAN_POINT('Ctrl Pts',(-5.38916666666667,-0.341881030314485,
-1.4));
#42561=CARTESIAN_POINT('Ctrl Pts',(-5.37147004253223,-0.310262756850051,
-1.4));
#42562=CARTESIAN_POINT('Ctrl Pts',(-5.35620231261545,-0.277219041062467,
-1.40143366869053));
#42563=CARTESIAN_POINT('Ctrl Pts',(-5.32761567846876,-0.200017956511921,
-1.40554873470576));
#42564=CARTESIAN_POINT('Ctrl Pts',(-5.31589717989396,-0.155336805463029,
-1.40841107882748));
#42565=CARTESIAN_POINT('Ctrl Pts',(-5.30499765049498,-0.0867080070700145,
-1.4112618373153));
#42566=CARTESIAN_POINT('Ctrl Pts',(-5.30248948591046,-0.0634567556288565,
-1.41198187968474));
#42567=CARTESIAN_POINT('Ctrl Pts',(-5.300382961066,-0.0267381544766586,
-1.41258893738177));
#42568=CARTESIAN_POINT('Ctrl Pts',(-5.3,-0.0133719921337942,-1.41270166537926));
#42569=CARTESIAN_POINT('Ctrl Pts',(-5.3,-6.1409211049579E-16,-1.41270166537926));
#42570=CARTESIAN_POINT('Origin',(-3.,-5.19615242270663,-0.985));
#42571=CARTESIAN_POINT('',(-3.7,-5.19615242270663,-1.4));
#42572=CARTESIAN_POINT('Origin',(-3.,-5.19615242270663,-1.4));
#42573=CARTESIAN_POINT('',(-3.7,-5.19615242270663,-0.985));
#42574=CARTESIAN_POINT('Origin',(-3.,-5.19615242270663,-1.4));
#42575=CARTESIAN_POINT('Origin',(6.9,0.,-1.4));
#42576=CARTESIAN_POINT('',(-6.9,-8.45006291411674E-16,-1.4));
#42577=CARTESIAN_POINT('Origin',(0.,0.,-1.4));
#42578=CARTESIAN_POINT('Origin',(6.,0.,-1.4));
#42579=CARTESIAN_POINT('',(2.3,5.19615242270663,-1.4));
#42580=CARTESIAN_POINT('Origin',(3.,5.19615242270663,-1.4));
#42581=CARTESIAN_POINT('Origin',(3.,5.19615242270663,-1.4));
#42582=CARTESIAN_POINT('',(-3.7,5.19615242270663,-1.4));
#42583=CARTESIAN_POINT('Origin',(-3.,5.19615242270663,-1.4));
#42584=CARTESIAN_POINT('Origin',(-3.,5.19615242270663,-1.4));
#42585=CARTESIAN_POINT('',(-6.7,6.49062803548097E-16,-1.4));
#42586=CARTESIAN_POINT('Origin',(-6.,7.34788079488412E-16,-1.4));
#42587=CARTESIAN_POINT('Origin',(-6.,7.34788079488412E-16,-1.4));
#42588=CARTESIAN_POINT('Origin',(-6.,7.34788079488412E-16,-0.985));
#42589=CARTESIAN_POINT('',(-6.7,6.49062803548097E-16,-0.985));
#42590=CARTESIAN_POINT('Origin',(-3.,5.19615242270663,-0.985));
#42591=CARTESIAN_POINT('',(-3.7,5.19615242270663,-0.985));
#42592=CARTESIAN_POINT('Origin',(3.,5.19615242270663,-0.985));
#42593=CARTESIAN_POINT('',(2.3,5.19615242270663,-0.985));
#42594=CARTESIAN_POINT('Origin',(6.,0.,-0.985));
#42595=CARTESIAN_POINT('',(5.3,-8.57252759403147E-17,-0.985));
#42596=CARTESIAN_POINT('Origin',(5.16,0.,-4.));
#42597=CARTESIAN_POINT('',(5.2,9.09728874746612E-17,-4.74285));
#42598=CARTESIAN_POINT('Origin',(5.2,0.,-4.));
#42599=CARTESIAN_POINT('',(5.12,-8.11757130814823E-17,-4.66285));
#42600=CARTESIAN_POINT('',(5.16,8.60743002780717E-17,-4.70285));
#42601=CARTESIAN_POINT('Origin',(5.12,0.,-4.));
#42602=CARTESIAN_POINT('Origin',(4.615,0.,-4.));
#42603=CARTESIAN_POINT('',(4.3,-9.6099007771999E-17,-4.66285));
#42604=CARTESIAN_POINT('',(4.615,-8.11757130814823E-17,-4.66285));
#42605=CARTESIAN_POINT('',(4.24860328549277,-0.66285,-4.));
#42606=CARTESIAN_POINT('Ctrl Pts',(4.24860328549277,-0.66285,-4.));
#42607=CARTESIAN_POINT('Ctrl Pts',(4.24860328549277,-0.66285,-4.08337270554936));
#42608=CARTESIAN_POINT('Ctrl Pts',(4.25131103029984,-0.646160681103361,
-4.17221014517061));
#42609=CARTESIAN_POINT('Ctrl Pts',(4.26104887749279,-0.578473468430526,
-4.33548236983766));
#42610=CARTESIAN_POINT('Ctrl Pts',(4.26793372257373,-0.527482714273786,
-4.40992874554522));
#42611=CARTESIAN_POINT('Ctrl Pts',(4.28082394210211,-0.409929889997929,
-4.52748156982108));
#42612=CARTESIAN_POINT('Ctrl Pts',(4.28767291694093,-0.335483021085273,
-4.57847322173307));
#42613=CARTESIAN_POINT('Ctrl Pts',(4.29732846342061,-0.172209109236183,
-4.64616108727907));
#42614=CARTESIAN_POINT('Ctrl Pts',(4.3,-0.0833710821908396,-4.66285));
#42615=CARTESIAN_POINT('Ctrl Pts',(4.3,-5.55111512312578E-17,-4.66285));
#42616=CARTESIAN_POINT('Ctrl Pts',(4.3,-1.11022302462516E-16,-4.66285));
#42617=CARTESIAN_POINT('Ctrl Pts',(4.3,0.0833710821908394,-4.66285));
#42618=CARTESIAN_POINT('Ctrl Pts',(4.29732846342061,0.172209109236183,-4.64616108727907));
#42619=CARTESIAN_POINT('Ctrl Pts',(4.28767291694093,0.335483021085273,-4.57847322173307));
#42620=CARTESIAN_POINT('Ctrl Pts',(4.28082394210211,0.409929889997929,-4.52748156982108));
#42621=CARTESIAN_POINT('Ctrl Pts',(4.26793372257373,0.527482714273785,-4.40992874554522));
#42622=CARTESIAN_POINT('Ctrl Pts',(4.26104887749279,0.578473468430526,-4.33548236983766));
#42623=CARTESIAN_POINT('Ctrl Pts',(4.25131103029984,0.646160681103361,-4.17221014517061));
#42624=CARTESIAN_POINT('Ctrl Pts',(4.24860328549277,0.66285,-4.08337270554937));
#42625=CARTESIAN_POINT('Ctrl Pts',(4.24860328549277,0.66285,-3.91662729445063));
#42626=CARTESIAN_POINT('Ctrl Pts',(4.25131103029984,0.646160681103361,-3.82778985482939));
#42627=CARTESIAN_POINT('Ctrl Pts',(4.26104887749279,0.578473468430526,-3.66451763016234));
#42628=CARTESIAN_POINT('Ctrl Pts',(4.26793372257373,0.527482714273786,-3.59007125445478));
#42629=CARTESIAN_POINT('Ctrl Pts',(4.28082394210211,0.40992988999793,-3.47251843017892));
#42630=CARTESIAN_POINT('Ctrl Pts',(4.28767291694093,0.335483021085274,-3.42152677826693));
#42631=CARTESIAN_POINT('Ctrl Pts',(4.29732846342061,0.172209109236183,-3.35383891272093));
#42632=CARTESIAN_POINT('Ctrl Pts',(4.3,0.0833710821908397,-3.33715));
#42633=CARTESIAN_POINT('Ctrl Pts',(4.3,-0.0833710821908394,-3.33715));
#42634=CARTESIAN_POINT('Ctrl Pts',(4.29732846342061,-0.172209109236183,
-3.35383891272093));
#42635=CARTESIAN_POINT('Ctrl Pts',(4.28767291694093,-0.335483021085273,
-3.42152677826693));
#42636=CARTESIAN_POINT('Ctrl Pts',(4.28082394210211,-0.409929889997929,
-3.47251843017892));
#42637=CARTESIAN_POINT('Ctrl Pts',(4.26793372257373,-0.527482714273785,
-3.59007125445478));
#42638=CARTESIAN_POINT('Ctrl Pts',(4.26104887749279,-0.578473468430526,
-3.66451763016234));
#42639=CARTESIAN_POINT('Ctrl Pts',(4.25131103029984,-0.646160681103361,
-3.82778985482939));
#42640=CARTESIAN_POINT('Ctrl Pts',(4.24860328549277,-0.66285,-3.91662729445063));
#42641=CARTESIAN_POINT('Ctrl Pts',(4.24860328549277,-0.66285,-4.));
#42642=CARTESIAN_POINT('Origin',(5.2,0.,-4.));
#42643=CARTESIAN_POINT('',(5.2,1.46957615897682E-16,-2.8));
#42644=CARTESIAN_POINT('Origin',(5.2,0.,-4.));
#42645=CARTESIAN_POINT('Origin',(5.15,0.,-4.));
#42646=CARTESIAN_POINT('',(5.1,-1.59204083889156E-16,-2.7));
#42647=CARTESIAN_POINT('',(5.15,-1.53080849893419E-16,-2.75));
#42648=CARTESIAN_POINT('Origin',(5.1,0.,-4.));
#42649=CARTESIAN_POINT('Origin',(4.4,0.,-4.));
#42650=CARTESIAN_POINT('',(5.,-1.62868768791465E-16,-2.7));
#42651=CARTESIAN_POINT('',(4.4,-1.59204083889156E-16,-2.7));
#42652=CARTESIAN_POINT('',(4.82804308182932,1.3,-4.));
#42653=CARTESIAN_POINT('Ctrl Pts',(4.82804308182932,1.3,-4.));
#42654=CARTESIAN_POINT('Ctrl Pts',(4.82804308182932,1.3,-4.16405971768551));
#42655=CARTESIAN_POINT('Ctrl Pts',(4.83727716857535,1.26705769140541,-4.33850900708893));
#42656=CARTESIAN_POINT('Ctrl Pts',(4.87015028662769,1.13416120781459,-4.65856059831929));
#42657=CARTESIAN_POINT('Ctrl Pts',(4.89326334703746,1.03424511530045,-4.80423251578458));
#42658=CARTESIAN_POINT('Ctrl Pts',(4.93628041072499,0.804251421167127,-5.0342262099179));
#42659=CARTESIAN_POINT('Ctrl Pts',(4.95904761708503,0.658571665059363,-5.1341570251573));
#42660=CARTESIAN_POINT('Ctrl Pts',(4.99112141383552,0.338492152411535,-5.26706427740736));
#42661=CARTESIAN_POINT('Ctrl Pts',(5.,0.164032748626163,-5.3));
#42662=CARTESIAN_POINT('Ctrl Pts',(5.,-0.164032748626163,-5.3));
#42663=CARTESIAN_POINT('Ctrl Pts',(4.99112141383552,-0.338492152411536,
-5.26706427740737));
#42664=CARTESIAN_POINT('Ctrl Pts',(4.95904761708503,-0.658571665059363,
-5.1341570251573));
#42665=CARTESIAN_POINT('Ctrl Pts',(4.93628041072499,-0.804251421167127,
-5.0342262099179));
#42666=CARTESIAN_POINT('Ctrl Pts',(4.89326334703746,-1.03424511530045,-4.80423251578458));
#42667=CARTESIAN_POINT('Ctrl Pts',(4.87015028662769,-1.13416120781459,-4.65856059831929));
#42668=CARTESIAN_POINT('Ctrl Pts',(4.83727716857535,-1.26705769140541,-4.33850900708893));
#42669=CARTESIAN_POINT('Ctrl Pts',(4.82804308182932,-1.3,-4.16405971768551));
#42670=CARTESIAN_POINT('Ctrl Pts',(4.82804308182932,-1.3,-3.83594028231449));
#42671=CARTESIAN_POINT('Ctrl Pts',(4.83727716857535,-1.26705769140541,-3.66149099291107));
#42672=CARTESIAN_POINT('Ctrl Pts',(4.87015028662769,-1.13416120781459,-3.34143940168072));
#42673=CARTESIAN_POINT('Ctrl Pts',(4.89326334703746,-1.03424511530045,-3.19576748421542));
#42674=CARTESIAN_POINT('Ctrl Pts',(4.93628041072499,-0.804251421167127,
-2.9657737900821));
#42675=CARTESIAN_POINT('Ctrl Pts',(4.95904761708503,-0.658571665059362,
-2.8658429748427));
#42676=CARTESIAN_POINT('Ctrl Pts',(4.99112141383552,-0.338492152411535,
-2.73293572259264));
#42677=CARTESIAN_POINT('Ctrl Pts',(5.,-0.164032748626163,-2.7));
#42678=CARTESIAN_POINT('Ctrl Pts',(5.,-2.22044604925031E-16,-2.7));
#42679=CARTESIAN_POINT('Ctrl Pts',(5.,-1.66533453693773E-16,-2.7));
#42680=CARTESIAN_POINT('Ctrl Pts',(5.,0.164032748626162,-2.7));
#42681=CARTESIAN_POINT('Ctrl Pts',(4.99112141383552,0.338492152411535,-2.73293572259263));
#42682=CARTESIAN_POINT('Ctrl Pts',(4.95904761708503,0.658571665059362,-2.8658429748427));
#42683=CARTESIAN_POINT('Ctrl Pts',(4.93628041072499,0.804251421167127,-2.9657737900821));
#42684=CARTESIAN_POINT('Ctrl Pts',(4.89326334703746,1.03424511530045,-3.19576748421542));
#42685=CARTESIAN_POINT('Ctrl Pts',(4.87015028662769,1.13416120781459,-3.34143940168072));
#42686=CARTESIAN_POINT('Ctrl Pts',(4.83727716857535,1.26705769140541,-3.66149099291107));
#42687=CARTESIAN_POINT('Ctrl Pts',(4.82804308182932,1.3,-3.83594028231449));
#42688=CARTESIAN_POINT('Ctrl Pts',(4.82804308182932,1.3,-4.));
#42689=CARTESIAN_POINT('Origin',(0.,0.,-0.0249999999999999));
#42690=CARTESIAN_POINT('',(4.3,-5.26598123633362E-16,-0.0499999999999998));
#42691=CARTESIAN_POINT('',(-4.3,-5.26598123633362E-16,-0.0499999999999998));
#42692=CARTESIAN_POINT('Origin',(0.,0.,-0.0499999999999998));
#42693=CARTESIAN_POINT('Origin',(0.,0.,-0.0499999999999998));
#42694=CARTESIAN_POINT('',(4.35,5.32721357629099E-16,0.));
#42695=CARTESIAN_POINT('',(4.325,-5.2965974063123E-16,-0.0249999999999999));
#42696=CARTESIAN_POINT('Origin',(0.,0.,0.));
#42697=CARTESIAN_POINT('Origin',(4.3,0.,0.));
#42698=CARTESIAN_POINT('',(-6.95,-8.5112952540741E-16,-3.19189119579733E-16));
#42699=CARTESIAN_POINT('Origin',(0.,0.,0.));
#42700=CARTESIAN_POINT('Origin',(0.,0.,-2.9));
#42701=CARTESIAN_POINT('',(-4.3,-5.26598123633362E-16,-5.8));
#42702=CARTESIAN_POINT('',(-4.3,-5.26598123633362E-16,-2.9));
#42703=CARTESIAN_POINT('Origin',(0.,0.,-5.8));
#42704=CARTESIAN_POINT('Origin',(0.,0.,-12.35));
#42705=CARTESIAN_POINT('',(2.1,-2.57175827820944E-16,-12.4));
#42706=CARTESIAN_POINT('Origin',(0.,0.,-12.4));
#42707=CARTESIAN_POINT('',(2.,2.44929359829471E-16,-12.3));
#42708=CARTESIAN_POINT('',(2.05,-2.51052593825207E-16,-12.35));
#42709=CARTESIAN_POINT('',(-2.,-2.44929359829471E-16,-12.3));
#42710=CARTESIAN_POINT('Origin',(0.,0.,-12.3));
#42711=CARTESIAN_POINT('Origin',(0.,0.,-12.3));
#42712=CARTESIAN_POINT('Origin',(0.,0.,-12.025));
#42713=CARTESIAN_POINT('',(-2.,-2.44929359829471E-16,-11.65));
#42714=CARTESIAN_POINT('Origin',(0.,0.,-11.65));
#42715=CARTESIAN_POINT('',(-2.,-2.44929359829471E-16,-12.025));
#42716=CARTESIAN_POINT('Origin',(3.1,0.,-12.4));
#42717=CARTESIAN_POINT('',(-3.1,-3.7964050773568E-16,-12.4));
#42718=CARTESIAN_POINT('Origin',(0.,0.,-12.4));
#42719=CARTESIAN_POINT('Origin',(0.,0.,-8.63617976663963));
#42720=CARTESIAN_POINT('',(-5.,-6.12323399573677E-16,-8.63617976663963));
#42721=CARTESIAN_POINT('Origin',(0.,0.,-8.63617976663963));
#42722=CARTESIAN_POINT('',(-4.74223748569721,-5.80756595765568E-16,-9.12900174604361));
#42723=CARTESIAN_POINT('Origin',(-4.4,-5.38844591624835E-16,-8.63617976663963));
#42724=CARTESIAN_POINT('Origin',(0.,-5.80756595765568E-16,-9.12900174604361));
#42725=CARTESIAN_POINT('Origin',(0.,0.,-5.175));
#42726=CARTESIAN_POINT('',(-5.,-6.12323399573677E-16,-5.175));
#42727=CARTESIAN_POINT('Origin',(0.,0.,-9.575));
#42728=CARTESIAN_POINT('',(-3.2,-3.91886975727153E-16,-10.2));
#42729=CARTESIAN_POINT('',(-4.1,-5.02105187650415E-16,-9.575));
#42730=CARTESIAN_POINT('Origin',(0.,0.,-10.2));
#42731=CARTESIAN_POINT('Origin',(0.,0.,-12.35));
#42732=CARTESIAN_POINT('',(-3.2,-3.91886975727153E-16,-12.3));
#42733=CARTESIAN_POINT('Origin',(0.,0.,-12.3));
#42734=CARTESIAN_POINT('',(-3.15,-3.85763741731416E-16,-12.35));
#42735=CARTESIAN_POINT('Origin',(0.,0.,-11.25));
#42736=CARTESIAN_POINT('',(-3.2,-3.91886975727153E-16,-11.25));
#42737=CARTESIAN_POINT('Origin',(0.,0.,-1.35));
#42738=CARTESIAN_POINT('',(-7.,-8.57252759403147E-16,-1.3));
#42739=CARTESIAN_POINT('Origin',(0.,0.,-1.3));
#42740=CARTESIAN_POINT('',(-6.95,-8.51129525407411E-16,-1.35));
#42741=CARTESIAN_POINT('Origin',(0.,0.,-0.699999999999999));
#42742=CARTESIAN_POINT('',(-7.,-8.57252759403147E-16,-0.0999999999999996));
#42743=CARTESIAN_POINT('Origin',(0.,0.,-0.0999999999999996));
#42744=CARTESIAN_POINT('',(-7.,-8.57252759403147E-16,-0.699999999999999));
#42745=CARTESIAN_POINT('Origin',(0.,0.,-0.0500000000000007));
#42746=CARTESIAN_POINT('',(-6.975,-8.54191142405279E-16,-0.0500000000000007));
#42747=CARTESIAN_POINT('Origin',(4.005,0.,-5.8));
#42748=CARTESIAN_POINT('',(-4.005,-4.90471043058515E-16,-5.8));
#42749=CARTESIAN_POINT('Origin',(0.,0.,-5.8));
#42750=CARTESIAN_POINT('Origin',(0.,0.,-7.5));
#42751=CARTESIAN_POINT('',(-4.005,-4.90471043058515E-16,-9.2));
#42752=CARTESIAN_POINT('',(-4.005,-4.90471043058515E-16,-7.5));
#42753=CARTESIAN_POINT('Origin',(0.,0.,-9.2));
#42754=CARTESIAN_POINT('Origin',(2.2,0.,-9.2));
#42755=CARTESIAN_POINT('',(-2.2,-2.69422295812418E-16,-9.2));
#42756=CARTESIAN_POINT('Origin',(0.,0.,-9.2));
#42757=CARTESIAN_POINT('Origin',(0.,0.,-9.4));
#42758=CARTESIAN_POINT('',(-2.2,-2.69422295812418E-16,-9.6));
#42759=CARTESIAN_POINT('',(-2.2,-2.69422295812418E-16,-9.4));
#42760=CARTESIAN_POINT('Origin',(0.,0.,-9.6));
#42761=CARTESIAN_POINT('Origin',(2.6,0.,-9.6));
#42762=CARTESIAN_POINT('',(-2.6,-3.18408167778312E-16,-9.6));
#42763=CARTESIAN_POINT('Origin',(0.,0.,-9.6));
#42764=CARTESIAN_POINT('Origin',(0.,0.,-10.25));
#42765=CARTESIAN_POINT('',(-2.6,-3.18408167778312E-16,-10.9));
#42766=CARTESIAN_POINT('',(-2.6,-3.18408167778312E-16,-10.25));
#42767=CARTESIAN_POINT('Origin',(0.,0.,-10.9));
#42768=CARTESIAN_POINT('Origin',(2.4,0.,-10.9));
#42769=CARTESIAN_POINT('',(-2.4,-2.93915231795365E-16,-10.9));
#42770=CARTESIAN_POINT('Origin',(0.,0.,-10.9));
#42771=CARTESIAN_POINT('Origin',(0.,0.,-11.275));
#42772=CARTESIAN_POINT('',(-2.4,-2.93915231795365E-16,-11.65));
#42773=CARTESIAN_POINT('',(-2.4,-2.93915231795365E-16,-11.275));
#42774=CARTESIAN_POINT('Origin',(0.,0.,-11.65));
#42775=CARTESIAN_POINT('Origin',(2.,0.,-11.65));
#42776=CARTESIAN_POINT('',(0.,0.,0.));
#42777=CARTESIAN_POINT('Origin',(6.,0.,2.385));
#42778=CARTESIAN_POINT('',(5.52,-5.8783046359073E-17,2.4));
#42779=CARTESIAN_POINT('Origin',(6.,0.,2.4));
#42780=CARTESIAN_POINT('',(5.55,5.51091059616309E-17,2.37));
#42781=CARTESIAN_POINT('',(5.535,-5.6946076160352E-17,2.385));
#42782=CARTESIAN_POINT('Origin',(6.,0.,2.37));
#42783=CARTESIAN_POINT('Origin',(6.,0.,1.21));
#42784=CARTESIAN_POINT('',(5.55,-5.51091059616309E-17,0.03));
#42785=CARTESIAN_POINT('Origin',(6.,0.,0.03));
#42786=CARTESIAN_POINT('',(5.55,-5.51091059616309E-17,1.21));
#42787=CARTESIAN_POINT('Origin',(1.5,0.,2.4));
#42788=CARTESIAN_POINT('',(-1.17046999107197,-6.8,2.4));
#42789=CARTESIAN_POINT('',(1.17046999107197,-6.8,2.4));
#42790=CARTESIAN_POINT('',(0.75,-6.8,2.4));
#42791=CARTESIAN_POINT('',(1.17046999107197,6.8,2.4));
#42792=CARTESIAN_POINT('Origin',(0.,0.,2.4));
#42793=CARTESIAN_POINT('',(-1.17046999107197,6.8,2.4));
#42794=CARTESIAN_POINT('',(0.75,6.8,2.4));
#42795=CARTESIAN_POINT('Origin',(0.,0.,2.4));
#42796=CARTESIAN_POINT('',(2.52,5.19615242270663,2.4));
#42797=CARTESIAN_POINT('Origin',(3.,5.19615242270663,2.4));
#42798=CARTESIAN_POINT('',(-6.48,6.76005033129339E-16,2.4));
#42799=CARTESIAN_POINT('Origin',(-6.,7.34788079488412E-16,2.4));
#42800=CARTESIAN_POINT('',(2.52,-5.19615242270663,2.4));
#42801=CARTESIAN_POINT('Origin',(3.,-5.19615242270663,2.4));
#42802=CARTESIAN_POINT('',(1.55,1.8982025386784E-16,2.4));
#42803=CARTESIAN_POINT('Origin',(0.,0.,2.4));
#42804=CARTESIAN_POINT('',(-0.3,4.8,2.4));
#42805=CARTESIAN_POINT('Origin',(0.,4.8,2.4));
#42806=CARTESIAN_POINT('',(-3.48,-5.19615242270663,2.4));
#42807=CARTESIAN_POINT('Origin',(-3.,-5.19615242270663,2.4));
#42808=CARTESIAN_POINT('',(-3.48,5.19615242270663,2.4));
#42809=CARTESIAN_POINT('Origin',(-3.,5.19615242270663,2.4));
#42810=CARTESIAN_POINT('Origin',(6.,0.,0.015));
#42811=CARTESIAN_POINT('',(5.52,5.8783046359073E-17,0.));
#42812=CARTESIAN_POINT('Origin',(6.,0.,0.));
#42813=CARTESIAN_POINT('',(5.535,5.6946076160352E-17,0.015));
#42814=CARTESIAN_POINT('Origin',(6.9,0.,0.));
#42815=CARTESIAN_POINT('',(1.17046999107197,-6.8,0.));
#42816=CARTESIAN_POINT('',(-1.17046999107197,-6.8,0.));
#42817=CARTESIAN_POINT('',(3.45,-6.8,0.));
#42818=CARTESIAN_POINT('',(-1.17046999107197,6.8,0.));
#42819=CARTESIAN_POINT('Origin',(0.,0.,0.));
#42820=CARTESIAN_POINT('',(1.17046999107197,6.8,0.));
#42821=CARTESIAN_POINT('',(3.45,6.8,0.));
#42822=CARTESIAN_POINT('Origin',(0.,0.,0.));
#42823=CARTESIAN_POINT('',(2.52,5.19615242270663,0.));
#42824=CARTESIAN_POINT('Origin',(3.,5.19615242270663,0.));
#42825=CARTESIAN_POINT('',(-6.48,7.93571125847485E-16,0.));
#42826=CARTESIAN_POINT('Origin',(-6.,7.34788079488412E-16,0.));
#42827=CARTESIAN_POINT('',(2.52,-5.19615242270663,0.));
#42828=CARTESIAN_POINT('Origin',(3.,-5.19615242270663,0.));
#42829=CARTESIAN_POINT('',(-1.84309209965023,1.29054698178985,0.));
#42830=CARTESIAN_POINT('',(1.84309209965023,1.29054698178985,0.));
#42831=CARTESIAN_POINT('Origin',(-2.22044604925031E-16,-4.44089209850063E-16,
0.));
#42832=CARTESIAN_POINT('',(2.41649853065253,1.69205048723559,0.));
#42833=CARTESIAN_POINT('Origin',(2.12979531515138,1.49129873451272,0.));
#42834=CARTESIAN_POINT('',(-2.41649853065253,1.69205048723559,0.));
#42835=CARTESIAN_POINT('Origin',(0.,8.88178419700125E-16,0.));
#42836=CARTESIAN_POINT('Origin',(-2.12979531515138,1.49129873451272,0.));
#42837=CARTESIAN_POINT('',(1.84309209965023,-1.29054698178985,0.));
#42838=CARTESIAN_POINT('',(-1.84309209965023,-1.29054698178985,0.));
#42839=CARTESIAN_POINT('Origin',(0.,0.,0.));
#42840=CARTESIAN_POINT('',(-2.41649853065253,-1.69205048723559,0.));
#42841=CARTESIAN_POINT('Origin',(-2.12979531515138,-1.49129873451272,0.));
#42842=CARTESIAN_POINT('',(2.41649853065253,-1.69205048723559,0.));
#42843=CARTESIAN_POINT('Origin',(0.,0.,0.));
#42844=CARTESIAN_POINT('Origin',(2.12979531515138,-1.49129873451272,0.));
#42845=CARTESIAN_POINT('',(1.55,-1.8982025386784E-16,0.));
#42846=CARTESIAN_POINT('Origin',(0.,0.,0.));
#42847=CARTESIAN_POINT('',(-3.48,-5.19615242270663,0.));
#42848=CARTESIAN_POINT('Origin',(-3.,-5.19615242270663,0.));
#42849=CARTESIAN_POINT('',(-3.48,5.19615242270663,0.));
#42850=CARTESIAN_POINT('Origin',(-3.,5.19615242270663,0.));
#42851=CARTESIAN_POINT('Origin',(3.,5.19615242270663,2.385));
#42852=CARTESIAN_POINT('',(2.55,5.19615242270663,2.37));
#42853=CARTESIAN_POINT('',(2.535,5.19615242270663,2.385));
#42854=CARTESIAN_POINT('Origin',(3.,5.19615242270663,2.37));
#42855=CARTESIAN_POINT('Origin',(3.,5.19615242270663,1.21));
#42856=CARTESIAN_POINT('',(2.55,5.19615242270663,0.03));
#42857=CARTESIAN_POINT('Origin',(3.,5.19615242270663,0.03));
#42858=CARTESIAN_POINT('',(2.55,5.19615242270663,1.21));
#42859=CARTESIAN_POINT('Origin',(3.,5.19615242270663,0.015));
#42860=CARTESIAN_POINT('',(2.535,5.19615242270663,0.015));
#42861=CARTESIAN_POINT('Origin',(-3.,5.19615242270663,2.385));
#42862=CARTESIAN_POINT('',(-3.45,5.19615242270663,2.37));
#42863=CARTESIAN_POINT('',(-3.465,5.19615242270663,2.385));
#42864=CARTESIAN_POINT('Origin',(-3.,5.19615242270663,2.37));
#42865=CARTESIAN_POINT('Origin',(-3.,5.19615242270663,1.21));
#42866=CARTESIAN_POINT('',(-3.45,5.19615242270663,0.03));
#42867=CARTESIAN_POINT('Origin',(-3.,5.19615242270663,0.03));
#42868=CARTESIAN_POINT('',(-3.45,5.19615242270663,1.21));
#42869=CARTESIAN_POINT('Origin',(-3.,5.19615242270663,0.015));
#42870=CARTESIAN_POINT('',(-3.465,5.19615242270663,0.015));
#42871=CARTESIAN_POINT('Origin',(-6.,7.34788079488412E-16,2.385));
#42872=CARTESIAN_POINT('',(-6.45,7.89897185450043E-16,2.37));
#42873=CARTESIAN_POINT('',(-6.465,6.7784200332806E-16,2.385));
#42874=CARTESIAN_POINT('Origin',(-6.,7.34788079488412E-16,2.37));
#42875=CARTESIAN_POINT('Origin',(-6.,7.34788079488412E-16,1.21));
#42876=CARTESIAN_POINT('',(-6.45,6.79678973526781E-16,0.03));
#42877=CARTESIAN_POINT('Origin',(-6.,7.34788079488412E-16,0.03));
#42878=CARTESIAN_POINT('',(-6.45,6.79678973526781E-16,1.21));
#42879=CARTESIAN_POINT('Origin',(-6.,7.34788079488412E-16,0.015));
#42880=CARTESIAN_POINT('',(-6.465,7.91734155648764E-16,0.015));
#42881=CARTESIAN_POINT('Origin',(-3.,-5.19615242270663,2.385));
#42882=CARTESIAN_POINT('',(-3.45,-5.19615242270663,2.37));
#42883=CARTESIAN_POINT('',(-3.465,-5.19615242270663,2.385));
#42884=CARTESIAN_POINT('Origin',(-3.,-5.19615242270663,2.37));
#42885=CARTESIAN_POINT('Origin',(-3.,-5.19615242270663,1.21));
#42886=CARTESIAN_POINT('',(-3.45,-5.19615242270663,0.03));
#42887=CARTESIAN_POINT('Origin',(-3.,-5.19615242270663,0.03));
#42888=CARTESIAN_POINT('',(-3.45,-5.19615242270663,1.21));
#42889=CARTESIAN_POINT('Origin',(-3.,-5.19615242270663,0.015));
#42890=CARTESIAN_POINT('',(-3.465,-5.19615242270663,0.015));
#42891=CARTESIAN_POINT('Origin',(3.,-5.19615242270663,2.385));
#42892=CARTESIAN_POINT('',(2.55,-5.19615242270663,2.37));
#42893=CARTESIAN_POINT('',(2.535,-5.19615242270663,2.385));
#42894=CARTESIAN_POINT('Origin',(3.,-5.19615242270663,2.37));
#42895=CARTESIAN_POINT('Origin',(3.,-5.19615242270663,1.21));
#42896=CARTESIAN_POINT('',(2.55,-5.19615242270663,0.03));
#42897=CARTESIAN_POINT('Origin',(3.,-5.19615242270663,0.03));
#42898=CARTESIAN_POINT('',(2.55,-5.19615242270663,1.21));
#42899=CARTESIAN_POINT('Origin',(3.,-5.19615242270663,0.015));
#42900=CARTESIAN_POINT('',(2.535,-5.19615242270663,0.015));
#42901=CARTESIAN_POINT('Origin',(0.,4.8,1.715));
#42902=CARTESIAN_POINT('',(0.3,4.8,1.71961524227066));
#42903=CARTESIAN_POINT('',(-0.3,4.8,1.71961524227066));
#42904=CARTESIAN_POINT('Ctrl Pts',(0.3,4.8,1.71961524227066));
#42905=CARTESIAN_POINT('Ctrl Pts',(0.3,4.83849152008815,1.71961524227066));
#42906=CARTESIAN_POINT('Ctrl Pts',(0.292165675343028,4.87894158037899,1.72434763078588));
#42907=CARTESIAN_POINT('Ctrl Pts',(0.261368612920868,4.95257470785234,1.7403588037382));
#42908=CARTESIAN_POINT('Ctrl Pts',(0.23842674843931,4.98583732027262,1.75131014026465));
#42909=CARTESIAN_POINT('Ctrl Pts',(0.185909000941879,5.03835506777005,1.77115998302115));
#42910=CARTESIAN_POINT('Ctrl Pts',(0.152622227434313,5.06134952397737,1.78147945231184));
#42911=CARTESIAN_POINT('Ctrl Pts',(0.0788835226466574,5.09218917176074,
1.7959775905052));
#42912=CARTESIAN_POINT('Ctrl Pts',(0.0383865903326067,5.1,1.8));
#42913=CARTESIAN_POINT('Ctrl Pts',(-0.0383865903326067,5.1,1.8));
#42914=CARTESIAN_POINT('Ctrl Pts',(-0.078883522646657,5.09218917176074,
1.7959775905052));
#42915=CARTESIAN_POINT('Ctrl Pts',(-0.152622227434313,5.06134952397737,
1.78147945231184));
#42916=CARTESIAN_POINT('Ctrl Pts',(-0.185909000941879,5.03835506777005,
1.77115998302115));
#42917=CARTESIAN_POINT('Ctrl Pts',(-0.23842674843931,4.98583732027262,1.75131014026465));
#42918=CARTESIAN_POINT('Ctrl Pts',(-0.261368612920868,4.95257470785235,
1.7403588037382));
#42919=CARTESIAN_POINT('Ctrl Pts',(-0.292165675343028,4.87894158037899,
1.72434763078588));
#42920=CARTESIAN_POINT('Ctrl Pts',(-0.3,4.83849152008815,1.71961524227066));
#42921=CARTESIAN_POINT('Ctrl Pts',(-0.3,4.8,1.71961524227066));
#42922=CARTESIAN_POINT('Ctrl Pts',(-0.3,4.8,1.71961524227066));
#42923=CARTESIAN_POINT('Ctrl Pts',(-0.3,4.76150847991185,1.71961524227066));
#42924=CARTESIAN_POINT('Ctrl Pts',(-0.292165675343028,4.72105841962101,
1.72434763078588));
#42925=CARTESIAN_POINT('Ctrl Pts',(-0.261368612920868,4.64742529214765,
1.7403588037382));
#42926=CARTESIAN_POINT('Ctrl Pts',(-0.23842674843931,4.61416267972738,1.75131014026465));
#42927=CARTESIAN_POINT('Ctrl Pts',(-0.185909000941879,4.56164493222995,
1.77115998302115));
#42928=CARTESIAN_POINT('Ctrl Pts',(-0.152622227434313,4.53865047602263,
1.78147945231184));
#42929=CARTESIAN_POINT('Ctrl Pts',(-0.0788835226466568,4.50781082823926,
1.7959775905052));
#42930=CARTESIAN_POINT('Ctrl Pts',(-0.0383865903326067,4.5,1.8));
#42931=CARTESIAN_POINT('Ctrl Pts',(0.0383865903326067,4.5,1.8));
#42932=CARTESIAN_POINT('Ctrl Pts',(0.0788835226466565,4.50781082823926,
1.7959775905052));
#42933=CARTESIAN_POINT('Ctrl Pts',(0.152622227434312,4.53865047602263,1.78147945231184));
#42934=CARTESIAN_POINT('Ctrl Pts',(0.185909000941879,4.56164493222995,1.77115998302115));
#42935=CARTESIAN_POINT('Ctrl Pts',(0.23842674843931,4.61416267972738,1.75131014026465));
#42936=CARTESIAN_POINT('Ctrl Pts',(0.261368612920868,4.64742529214765,1.7403588037382));
#42937=CARTESIAN_POINT('Ctrl Pts',(0.292165675343028,4.72105841962101,1.72434763078588));
#42938=CARTESIAN_POINT('Ctrl Pts',(0.3,4.76150847991185,1.71961524227066));
#42939=CARTESIAN_POINT('Ctrl Pts',(0.3,4.8,1.71961524227066));
#42940=CARTESIAN_POINT('',(-0.3,4.8,1.715));
#42941=CARTESIAN_POINT('Origin',(0.,6.76,1.2));
#42942=CARTESIAN_POINT('',(-1.12434822629719E-16,6.8,0.2819));
#42943=CARTESIAN_POINT('Origin',(0.,6.8,1.2));
#42944=CARTESIAN_POINT('',(1.0263764823654E-16,6.72,0.3619));
#42945=CARTESIAN_POINT('',(-1.07536235433129E-16,6.76,0.3219));
#42946=CARTESIAN_POINT('Origin',(0.,6.72,1.2));
#42947=CARTESIAN_POINT('Origin',(0.,6.115,1.2));
#42948=CARTESIAN_POINT('',(-1.0263764823654E-16,5.4,0.3619));
#42949=CARTESIAN_POINT('Origin',(0.,5.4,1.2));
#42950=CARTESIAN_POINT('',(-1.0263764823654E-16,6.115,0.3619));
#42951=CARTESIAN_POINT('Origin',(0.,6.8,1.2));
#42952=CARTESIAN_POINT('',(1.66132477258362,6.8,2.3));
#42953=CARTESIAN_POINT('Ctrl Pts',(1.66132477258361,6.8,2.3));
#42954=CARTESIAN_POINT('Ctrl Pts',(1.41413171714607,6.8,2.35866684951557));
#42955=CARTESIAN_POINT('Ctrl Pts',(1.17046999107197,6.8,2.4));
#42956=CARTESIAN_POINT('',(1.66132477258362,6.8,0.1));
#42957=CARTESIAN_POINT('',(1.66132477258362,6.8,1.2));
#42958=CARTESIAN_POINT('Ctrl Pts',(1.17046999107197,6.8,-1.11022302462516E-16));
#42959=CARTESIAN_POINT('Ctrl Pts',(1.4141317171461,6.8,0.0413331504844302));
#42960=CARTESIAN_POINT('Ctrl Pts',(1.66132477258362,6.8,0.1));
#42961=CARTESIAN_POINT('',(-1.66132477258362,6.8,0.1));
#42962=CARTESIAN_POINT('Ctrl Pts',(-1.66132477258362,6.8,0.1));
#42963=CARTESIAN_POINT('Ctrl Pts',(-1.4141317171461,6.8,0.0413331504844302));
#42964=CARTESIAN_POINT('Ctrl Pts',(-1.17046999107197,6.8,-1.11022302462516E-16));
#42965=CARTESIAN_POINT('',(-1.66132477258362,6.8,2.3));
#42966=CARTESIAN_POINT('',(-1.66132477258362,6.8,1.2));
#42967=CARTESIAN_POINT('Ctrl Pts',(-1.17046999107197,6.8,2.4));
#42968=CARTESIAN_POINT('Ctrl Pts',(-1.41413171714607,6.8,2.35866684951557));
#42969=CARTESIAN_POINT('Ctrl Pts',(-1.66132477258361,6.8,2.3));
#42970=CARTESIAN_POINT('Origin',(0.,-6.76,1.2));
#42971=CARTESIAN_POINT('',(1.12434822629719E-16,-6.8,0.2819));
#42972=CARTESIAN_POINT('Origin',(0.,-6.8,1.2));
#42973=CARTESIAN_POINT('',(-1.0263764823654E-16,-6.72,0.3619));
#42974=CARTESIAN_POINT('',(1.07536235433129E-16,-6.76,0.3219));
#42975=CARTESIAN_POINT('Origin',(0.,-6.72,1.2));
#42976=CARTESIAN_POINT('Origin',(0.,-6.115,1.2));
#42977=CARTESIAN_POINT('',(-1.0263764823654E-16,-5.4,0.3619));
#42978=CARTESIAN_POINT('',(-1.0263764823654E-16,-6.115,0.3619));
#42979=CARTESIAN_POINT('Origin',(0.,-5.4,1.2));
#42980=CARTESIAN_POINT('Origin',(0.,-6.8,1.2));
#42981=CARTESIAN_POINT('',(-1.66132477258362,-6.8,2.3));
#42982=CARTESIAN_POINT('Ctrl Pts',(-1.66132477258361,-6.8,2.3));
#42983=CARTESIAN_POINT('Ctrl Pts',(-1.41413171714607,-6.8,2.35866684951557));
#42984=CARTESIAN_POINT('Ctrl Pts',(-1.17046999107197,-6.8,2.4));
#42985=CARTESIAN_POINT('',(-1.66132477258362,-6.8,0.1));
#42986=CARTESIAN_POINT('',(-1.66132477258362,-6.8,1.2));
#42987=CARTESIAN_POINT('Ctrl Pts',(-1.17046999107197,-6.8,-1.52655665885959E-16));
#42988=CARTESIAN_POINT('Ctrl Pts',(-1.4141317171461,-6.8,0.04133315048443));
#42989=CARTESIAN_POINT('Ctrl Pts',(-1.66132477258362,-6.8,0.1));
#42990=CARTESIAN_POINT('',(1.66132477258362,-6.8,0.1));
#42991=CARTESIAN_POINT('Ctrl Pts',(1.66132477258362,-6.8,0.1));
#42992=CARTESIAN_POINT('Ctrl Pts',(1.4141317171461,-6.8,0.04133315048443));
#42993=CARTESIAN_POINT('Ctrl Pts',(1.17046999107197,-6.8,-1.52655665885959E-16));
#42994=CARTESIAN_POINT('',(1.66132477258362,-6.8,2.3));
#42995=CARTESIAN_POINT('',(1.66132477258362,-6.8,1.2));
#42996=CARTESIAN_POINT('Ctrl Pts',(1.17046999107197,-6.8,2.4));
#42997=CARTESIAN_POINT('Ctrl Pts',(1.41413171714607,-6.8,2.35866684951557));
#42998=CARTESIAN_POINT('Ctrl Pts',(1.66132477258361,-6.8,2.3));
#42999=CARTESIAN_POINT('Origin',(0.,-3.8,1.2));
#43000=CARTESIAN_POINT('',(-7.34788079488412E-17,-5.4,0.6));
#43001=CARTESIAN_POINT('Origin',(0.,-5.4,1.2));
#43002=CARTESIAN_POINT('',(-5.75560856861423E-17,-2.95,0.6));
#43003=CARTESIAN_POINT('',(-7.34788079488412E-17,-3.8,0.6));
#43004=CARTESIAN_POINT('',(-0.565685424949239,-2.89525473836069,1.));
#43005=CARTESIAN_POINT('Ctrl Pts',(-0.565685424949238,-2.89525473836069,
1.));
#43006=CARTESIAN_POINT('Ctrl Pts',(-0.562127356844792,-2.89594992667728,
0.98993626366169));
#43007=CARTESIAN_POINT('Ctrl Pts',(-0.558298097879191,-2.89669131763276,
0.979960768047715));
#43008=CARTESIAN_POINT('Ctrl Pts',(-0.523558121743437,-2.90333610967591,
0.896216130064144));
#43009=CARTESIAN_POINT('Ctrl Pts',(-0.477417986945562,-2.91160730139143,
0.828889849521705));
#43010=CARTESIAN_POINT('Ctrl Pts',(-0.371113340250497,-2.92705646583967,
0.722585202826639));
#43011=CARTESIAN_POINT('Ctrl Pts',(-0.303785706689727,-2.93525235179074,
0.676442570241645));
#43012=CARTESIAN_POINT('Ctrl Pts',(-0.156018762471502,-2.94680339855193,
0.615144217035157));
#43013=CARTESIAN_POINT('Ctrl Pts',(-0.0755623283236566,-2.95,0.6));
#43014=CARTESIAN_POINT('Ctrl Pts',(-1.38777878078145E-17,-2.95,0.6));
#43015=CARTESIAN_POINT('',(-0.565685424949238,-2.2,1.));
#43016=CARTESIAN_POINT('',(-0.565685424949238,-3.8,1.));
#43017=CARTESIAN_POINT('',(0.565685424949238,-2.2,1.));
#43018=CARTESIAN_POINT('Origin',(0.,-2.2,1.2));
#43019=CARTESIAN_POINT('',(0.565685424949239,-2.89525473836069,1.));
#43020=CARTESIAN_POINT('',(0.565685424949238,-3.8,1.));
#43021=CARTESIAN_POINT('Ctrl Pts',(-1.38777878078145E-17,-2.95,0.6));
#43022=CARTESIAN_POINT('Ctrl Pts',(0.0755623283236566,-2.95,0.6));
#43023=CARTESIAN_POINT('Ctrl Pts',(0.156018762471502,-2.94680339855193,
0.615144217035157));
#43024=CARTESIAN_POINT('Ctrl Pts',(0.303785706689727,-2.93525235179075,
0.676442570241645));
#43025=CARTESIAN_POINT('Ctrl Pts',(0.371113340250496,-2.92705646583967,
0.722585202826639));
#43026=CARTESIAN_POINT('Ctrl Pts',(0.477417986945562,-2.91160730139143,
0.828889849521705));
#43027=CARTESIAN_POINT('Ctrl Pts',(0.523558121743436,-2.90333610967591,
0.896216130064144));
#43028=CARTESIAN_POINT('Ctrl Pts',(0.55829809787919,-2.89669131763276,0.979960768047715));
#43029=CARTESIAN_POINT('Ctrl Pts',(0.562127356844792,-2.89594992667728,
0.98993626366169));
#43030=CARTESIAN_POINT('Ctrl Pts',(0.565685424949238,-2.89525473836069,
1.));
#43031=CARTESIAN_POINT('Origin',(0.,-3.8,1.2));
#43032=CARTESIAN_POINT('',(0.47169905660283,-2.2,0.829190075645216));
#43033=CARTESIAN_POINT('',(-0.47169905660283,-2.2,0.829190075645216));
#43034=CARTESIAN_POINT('Ctrl Pts',(0.47169905660283,-2.2,0.829190075645216));
#43035=CARTESIAN_POINT('Ctrl Pts',(0.456732221663335,-2.20320901905513,
0.810151097835833));
#43036=CARTESIAN_POINT('Ctrl Pts',(0.44080709474806,-2.20646161675427,0.792278957324203));
#43037=CARTESIAN_POINT('Ctrl Pts',(0.371203803057213,-2.21982587642206,
0.722675665633356));
#43038=CARTESIAN_POINT('Ctrl Pts',(0.303979231951913,-2.2306075153835,0.676556496463189));
#43039=CARTESIAN_POINT('Ctrl Pts',(0.156255272557804,-2.24579552733492,
0.615208780719168));
#43040=CARTESIAN_POINT('Ctrl Pts',(0.0757269887719169,-2.25,0.6));
#43041=CARTESIAN_POINT('Ctrl Pts',(-0.0757269887719168,-2.25,0.6));
#43042=CARTESIAN_POINT('Ctrl Pts',(-0.156255272557804,-2.24579552733492,
0.615208780719168));
#43043=CARTESIAN_POINT('Ctrl Pts',(-0.303979231951912,-2.2306075153835,
0.676556496463189));
#43044=CARTESIAN_POINT('Ctrl Pts',(-0.371203803057213,-2.21982587642206,
0.722675665633356));
#43045=CARTESIAN_POINT('Ctrl Pts',(-0.44080709474806,-2.20646161675427,
0.792278957324203));
#43046=CARTESIAN_POINT('Ctrl Pts',(-0.456732221663335,-2.20320901905513,
0.810151097835833));
#43047=CARTESIAN_POINT('Ctrl Pts',(-0.47169905660283,-2.2,0.829190075645216));
#43048=CARTESIAN_POINT('',(-7.34788079488412E-17,-2.2,0.6));
#43049=CARTESIAN_POINT('Origin',(0.,-2.2,1.2));
#43050=CARTESIAN_POINT('Origin',(0.,-2.2,1.2));
#43051=CARTESIAN_POINT('Origin',(0.,-5.4,1.8));
#43052=CARTESIAN_POINT('Origin',(0.,-2.2,1.2));
#43053=CARTESIAN_POINT('',(0.538458996921356,-2.18461939674499,1.));
#43054=CARTESIAN_POINT('Ctrl Pts',(0.538458996921356,-2.18461939674499,
1.));
#43055=CARTESIAN_POINT('Ctrl Pts',(0.535129652878092,-2.18544000433303,
0.987114058586867));
#43056=CARTESIAN_POINT('Ctrl Pts',(0.531468422935026,-2.18633440357531,
0.974298290302466));
#43057=CARTESIAN_POINT('Ctrl Pts',(0.512986185718411,-2.1907915344852,0.915394770294079));
#43058=CARTESIAN_POINT('Ctrl Pts',(0.494116619449461,-2.19519348034269,
0.870650612337028));
#43059=CARTESIAN_POINT('Ctrl Pts',(0.471699056602829,-2.2,0.829190075645216));
#43060=CARTESIAN_POINT('Ctrl Pts',(0.565685424949238,-2.2,1.));
#43061=CARTESIAN_POINT('Ctrl Pts',(0.551775493286436,-2.1921200678861,1.));
#43062=CARTESIAN_POINT('Ctrl Pts',(0.538458996921356,-2.18461939674499,
1.));
#43063=CARTESIAN_POINT('',(-0.538458996921356,-2.18461939674499,1.));
#43064=CARTESIAN_POINT('Ctrl Pts',(-0.538458996921356,-2.18461939674499,
1.));
#43065=CARTESIAN_POINT('Ctrl Pts',(-0.551775493286438,-2.1921200678861,
1.));
#43066=CARTESIAN_POINT('Ctrl Pts',(-0.565685424949238,-2.2,1.));
#43067=CARTESIAN_POINT('Ctrl Pts',(-0.471699056602829,-2.2,0.829190075645216));
#43068=CARTESIAN_POINT('Ctrl Pts',(-0.494116619449461,-2.19519348034269,
0.870650612337028));
#43069=CARTESIAN_POINT('Ctrl Pts',(-0.512986185718411,-2.1907915344852,
0.915394770294079));
#43070=CARTESIAN_POINT('Ctrl Pts',(-0.531468422935026,-2.18633440357531,
0.974298290302465));
#43071=CARTESIAN_POINT('Ctrl Pts',(-0.535129652878092,-2.18544000433303,
0.987114058586867));
#43072=CARTESIAN_POINT('Ctrl Pts',(-0.538458996921356,-2.18461939674499,
1.));
#43073=CARTESIAN_POINT('',(0.,-1.83948362858346,1.2));
#43074=CARTESIAN_POINT('',(-7.34788079488412E-17,-2.2,0.6));
#43075=CARTESIAN_POINT('Origin',(0.,0.,0.));
#43076=CARTESIAN_POINT('',(-1.84309209965023,-1.29054698178985,1.));
#43077=CARTESIAN_POINT('Origin',(0.,0.,1.));
#43078=CARTESIAN_POINT('',(-1.84309209965023,-1.29054698178985,0.));
#43079=CARTESIAN_POINT('',(1.84309209965023,-1.29054698178985,1.));
#43080=CARTESIAN_POINT('',(1.84309209965023,-1.29054698178985,0.));
#43081=CARTESIAN_POINT('Origin',(0.,0.,1.));
#43082=CARTESIAN_POINT('Origin',(0.,-2.04564936725636,1.));
#43083=CARTESIAN_POINT('',(-2.41649853065253,-1.69205048723559,1.));
#43084=CARTESIAN_POINT('Origin',(0.,0.,1.));
#43085=CARTESIAN_POINT('Origin',(-2.12979531515138,-1.49129873451272,1.));
#43086=CARTESIAN_POINT('Origin',(0.,0.,0.0499999999999998));
#43087=CARTESIAN_POINT('Origin',(0.,0.,0.1));
#43088=CARTESIAN_POINT('Origin',(0.,0.,1.2));
#43089=CARTESIAN_POINT('Origin',(0.,0.,2.3));
#43090=CARTESIAN_POINT('Origin',(0.,0.,2.35));
#43091=CARTESIAN_POINT('Origin',(0.,3.8,1.2));
#43092=CARTESIAN_POINT('',(-0.565685424949238,2.89525473836069,1.));
#43093=CARTESIAN_POINT('',(-0.565685424949238,2.2,1.));
#43094=CARTESIAN_POINT('',(-0.565685424949238,3.8,1.));
#43095=CARTESIAN_POINT('',(-2.04493445488446E-18,2.95,0.6));
#43096=CARTESIAN_POINT('Ctrl Pts',(4.16333634234434E-17,2.95,0.6));
#43097=CARTESIAN_POINT('Ctrl Pts',(-0.0755623283236565,2.95,0.6));
#43098=CARTESIAN_POINT('Ctrl Pts',(-0.156018762471502,2.94680339855193,
0.615144217035157));
#43099=CARTESIAN_POINT('Ctrl Pts',(-0.303785706689727,2.93525235179075,
0.676442570241645));
#43100=CARTESIAN_POINT('Ctrl Pts',(-0.371113340250496,2.92705646583967,
0.722585202826639));
#43101=CARTESIAN_POINT('Ctrl Pts',(-0.477417986945562,2.91160730139143,
0.828889849521705));
#43102=CARTESIAN_POINT('Ctrl Pts',(-0.523558121743437,2.90333610967591,
0.896216130064144));
#43103=CARTESIAN_POINT('Ctrl Pts',(-0.558298097879191,2.89669131763276,
0.979960768047715));
#43104=CARTESIAN_POINT('Ctrl Pts',(-0.562127356844792,2.89594992667728,
0.989936263661689));
#43105=CARTESIAN_POINT('Ctrl Pts',(-0.565685424949238,2.89525473836069,
1.));
#43106=CARTESIAN_POINT('',(-7.34788079488412E-17,5.4,0.6));
#43107=CARTESIAN_POINT('',(-7.34788079488412E-17,3.8,0.6));
#43108=CARTESIAN_POINT('Origin',(0.,5.4,1.2));
#43109=CARTESIAN_POINT('',(0.565685424949238,2.89525473836069,1.));
#43110=CARTESIAN_POINT('Ctrl Pts',(0.565685424949238,2.89525473836069,1.));
#43111=CARTESIAN_POINT('Ctrl Pts',(0.562127356844792,2.89594992667728,0.98993626366169));
#43112=CARTESIAN_POINT('Ctrl Pts',(0.55829809787919,2.89669131763276,0.979960768047715));
#43113=CARTESIAN_POINT('Ctrl Pts',(0.523558121743437,2.90333610967591,0.896216130064144));
#43114=CARTESIAN_POINT('Ctrl Pts',(0.477417986945562,2.91160730139143,0.828889849521705));
#43115=CARTESIAN_POINT('Ctrl Pts',(0.371113340250497,2.92705646583967,0.722585202826639));
#43116=CARTESIAN_POINT('Ctrl Pts',(0.303785706689727,2.93525235179075,0.676442570241645));
#43117=CARTESIAN_POINT('Ctrl Pts',(0.156018762471502,2.94680339855193,0.615144217035157));
#43118=CARTESIAN_POINT('Ctrl Pts',(0.0755623283236566,2.95,0.6));
#43119=CARTESIAN_POINT('Ctrl Pts',(4.16333634234434E-17,2.95,0.6));
#43120=CARTESIAN_POINT('',(0.565685424949238,2.2,1.));
#43121=CARTESIAN_POINT('',(0.565685424949238,3.8,1.));
#43122=CARTESIAN_POINT('Origin',(0.,2.2,1.2));
#43123=CARTESIAN_POINT('Origin',(0.,3.8,1.2));
#43124=CARTESIAN_POINT('',(-0.47169905660283,2.2,0.829190075645216));
#43125=CARTESIAN_POINT('',(0.471699056602829,2.2,0.829190075645216));
#43126=CARTESIAN_POINT('Ctrl Pts',(-0.47169905660283,2.2,0.829190075645216));
#43127=CARTESIAN_POINT('Ctrl Pts',(-0.456732221663335,2.20320901905513,
0.810151097835833));
#43128=CARTESIAN_POINT('Ctrl Pts',(-0.44080709474806,2.20646161675427,0.792278957324203));
#43129=CARTESIAN_POINT('Ctrl Pts',(-0.371203803057213,2.21982587642206,
0.722675665633356));
#43130=CARTESIAN_POINT('Ctrl Pts',(-0.303979231951913,2.2306075153835,0.676556496463189));
#43131=CARTESIAN_POINT('Ctrl Pts',(-0.156255272557804,2.24579552733492,
0.615208780719168));
#43132=CARTESIAN_POINT('Ctrl Pts',(-0.0757269887719169,2.25,0.6));
#43133=CARTESIAN_POINT('Ctrl Pts',(0.0757269887719168,2.25,0.6));
#43134=CARTESIAN_POINT('Ctrl Pts',(0.156255272557804,2.24579552733492,0.615208780719168));
#43135=CARTESIAN_POINT('Ctrl Pts',(0.303979231951912,2.2306075153835,0.676556496463189));
#43136=CARTESIAN_POINT('Ctrl Pts',(0.371203803057213,2.21982587642206,0.722675665633356));
#43137=CARTESIAN_POINT('Ctrl Pts',(0.44080709474806,2.20646161675427,0.792278957324203));
#43138=CARTESIAN_POINT('Ctrl Pts',(0.456732221663335,2.20320901905513,0.810151097835833));
#43139=CARTESIAN_POINT('Ctrl Pts',(0.471699056602829,2.2,0.829190075645216));
#43140=CARTESIAN_POINT('',(-7.34788079488413E-17,2.2,0.599999999999999));
#43141=CARTESIAN_POINT('Origin',(0.,2.2,1.2));
#43142=CARTESIAN_POINT('Origin',(0.,2.2,1.2));
#43143=CARTESIAN_POINT('Origin',(0.,2.01974181429173,1.2));
#43144=CARTESIAN_POINT('',(0.,1.83948362858346,1.2));
#43145=CARTESIAN_POINT('',(-3.67394039744206E-17,2.01974181429173,0.9));
#43146=CARTESIAN_POINT('',(-0.538458996921356,2.18461939674499,1.));
#43147=CARTESIAN_POINT('Ctrl Pts',(-0.538458996921356,2.18461939674499,
1.));
#43148=CARTESIAN_POINT('Ctrl Pts',(-0.535129652878092,2.18544000433303,
0.987114058586867));
#43149=CARTESIAN_POINT('Ctrl Pts',(-0.531468422935027,2.18633440357531,
0.974298290302465));
#43150=CARTESIAN_POINT('Ctrl Pts',(-0.512986185718411,2.1907915344852,0.915394770294079));
#43151=CARTESIAN_POINT('Ctrl Pts',(-0.494116619449461,2.19519348034269,
0.870650612337029));
#43152=CARTESIAN_POINT('Ctrl Pts',(-0.47169905660283,2.2,0.829190075645216));
#43153=CARTESIAN_POINT('Ctrl Pts',(-0.565685424949238,2.2,1.));
#43154=CARTESIAN_POINT('Ctrl Pts',(-0.551775493286436,2.1921200678861,1.));
#43155=CARTESIAN_POINT('Ctrl Pts',(-0.538458996921356,2.18461939674499,
1.));
#43156=CARTESIAN_POINT('',(0.538458996921356,2.18461939674499,1.));
#43157=CARTESIAN_POINT('Ctrl Pts',(0.538458996921356,2.18461939674499,1.));
#43158=CARTESIAN_POINT('Ctrl Pts',(0.551775493286434,2.1921200678861,1.));
#43159=CARTESIAN_POINT('Ctrl Pts',(0.565685424949238,2.2,1.));
#43160=CARTESIAN_POINT('Ctrl Pts',(0.47169905660283,2.2,0.829190075645216));
#43161=CARTESIAN_POINT('Ctrl Pts',(0.494116619449461,2.19519348034269,0.870650612337028));
#43162=CARTESIAN_POINT('Ctrl Pts',(0.51298618571841,2.1907915344852,0.915394770294079));
#43163=CARTESIAN_POINT('Ctrl Pts',(0.531468422935026,2.18633440357531,0.974298290302465));
#43164=CARTESIAN_POINT('Ctrl Pts',(0.535129652878092,2.18544000433303,0.987114058586867));
#43165=CARTESIAN_POINT('Ctrl Pts',(0.538458996921356,2.18461939674499,1.));
#43166=CARTESIAN_POINT('Origin',(0.,5.4,2.0381));
#43167=CARTESIAN_POINT('Origin',(-2.22044604925031E-16,-4.44089209850063E-16,
0.));
#43168=CARTESIAN_POINT('',(1.84309209965023,1.29054698178985,1.));
#43169=CARTESIAN_POINT('Origin',(-2.22044604925031E-16,-4.44089209850063E-16,
1.));
#43170=CARTESIAN_POINT('',(1.84309209965023,1.29054698178985,0.));
#43171=CARTESIAN_POINT('',(-1.84309209965023,1.29054698178985,1.));
#43172=CARTESIAN_POINT('',(-1.84309209965023,1.29054698178985,0.));
#43173=CARTESIAN_POINT('Origin',(-2.22044604925031E-16,-4.44089209850063E-16,
1.));
#43174=CARTESIAN_POINT('Origin',(-4.44089209850063E-16,2.04564936725636,
1.));
#43175=CARTESIAN_POINT('',(2.41649853065253,1.69205048723559,1.));
#43176=CARTESIAN_POINT('Origin',(0.,8.88178419700125E-16,1.));
#43177=CARTESIAN_POINT('Origin',(2.12979531515138,1.49129873451272,1.));
#43178=CARTESIAN_POINT('Origin',(-2.12979531515138,1.49129873451272,0.));
#43179=CARTESIAN_POINT('',(-2.41649853065253,1.69205048723559,1.));
#43180=CARTESIAN_POINT('',(-2.41649853065253,1.69205048723559,0.));
#43181=CARTESIAN_POINT('Origin',(-2.12979531515138,1.49129873451272,1.));
#43182=CARTESIAN_POINT('Origin',(0.,8.88178419700125E-16,0.));
#43183=CARTESIAN_POINT('Origin',(0.,8.88178419700125E-16,1.));
#43184=CARTESIAN_POINT('',(2.41649853065253,1.69205048723559,0.));
#43185=CARTESIAN_POINT('Origin',(2.12979531515138,1.49129873451272,0.));
#43186=CARTESIAN_POINT('Origin',(-4.44089209850063E-16,2.04564936725636,
1.));
#43187=CARTESIAN_POINT('Origin',(2.12979531515138,-1.49129873451272,0.));
#43188=CARTESIAN_POINT('',(2.41649853065253,-1.69205048723559,1.));
#43189=CARTESIAN_POINT('',(2.41649853065253,-1.69205048723559,0.));
#43190=CARTESIAN_POINT('Origin',(2.12979531515138,-1.49129873451272,1.));
#43191=CARTESIAN_POINT('Origin',(0.,0.,0.));
#43192=CARTESIAN_POINT('Origin',(0.,0.,1.));
#43193=CARTESIAN_POINT('',(-2.41649853065253,-1.69205048723559,0.));
#43194=CARTESIAN_POINT('Origin',(-2.12979531515138,-1.49129873451272,0.));
#43195=CARTESIAN_POINT('Origin',(0.,-2.04564936725636,1.));
#43196=CARTESIAN_POINT('Origin',(0.,0.,0.025));
#43197=CARTESIAN_POINT('',(1.5,1.83697019872103E-16,0.05));
#43198=CARTESIAN_POINT('',(1.525,-1.86758636869971E-16,0.025));
#43199=CARTESIAN_POINT('',(-1.5,-1.83697019872103E-16,0.05));
#43200=CARTESIAN_POINT('Origin',(0.,0.,0.05));
#43201=CARTESIAN_POINT('Origin',(0.,0.,0.05));
#43202=CARTESIAN_POINT('Origin',(0.,0.,1.2));
#43203=CARTESIAN_POINT('',(1.5,-1.83697019872103E-16,2.35));
#43204=CARTESIAN_POINT('',(-1.5,-1.83697019872103E-16,2.35));
#43205=CARTESIAN_POINT('Origin',(0.,0.,2.35));
#43206=CARTESIAN_POINT('Origin',(0.,0.,2.35));
#43207=CARTESIAN_POINT('',(-1.5,-1.83697019872103E-16,1.2));
#43208=CARTESIAN_POINT('Origin',(0.,0.,2.375));
#43209=CARTESIAN_POINT('',(1.525,-1.86758636869971E-16,2.375));
#43210=CARTESIAN_POINT('Origin',(0.,0.,0.0499999999999998));
#43211=CARTESIAN_POINT('Origin',(0.,0.,0.1));
#43212=CARTESIAN_POINT('Origin',(0.,0.,1.2));
#43213=CARTESIAN_POINT('Origin',(0.,0.,2.3));
#43214=CARTESIAN_POINT('Origin',(0.,0.,2.35));
#43215=CARTESIAN_POINT('',(0.,0.,0.));
#43216=CARTESIAN_POINT('Ctrl Pts',(0.156070932745934,-0.596521174907684,
5.4));
#43217=CARTESIAN_POINT('Ctrl Pts',(0.156070932745934,-0.596521174907684,
5.37));
#43218=CARTESIAN_POINT('Ctrl Pts',(0.166950926184654,-0.573635852336884,
5.4));
#43219=CARTESIAN_POINT('Ctrl Pts',(0.166950926184654,-0.573635852336884,
5.37));
#43220=CARTESIAN_POINT('Ctrl Pts',(0.166950926184654,-0.528990542888641,
5.4));
#43221=CARTESIAN_POINT('Ctrl Pts',(0.166950926184654,-0.528990542888641,
5.37));
#43222=CARTESIAN_POINT('',(0.156070932745934,-0.596521174907684,5.4));
#43223=CARTESIAN_POINT('',(0.166950926184654,-0.528990542888641,5.4));
#43224=CARTESIAN_POINT('Ctrl Pts',(0.156070932745934,-0.596521174907684,
5.4));
#43225=CARTESIAN_POINT('Ctrl Pts',(0.166950926184654,-0.573635852336884,
5.4));
#43226=CARTESIAN_POINT('Ctrl Pts',(0.166950926184654,-0.528990542888641,
5.4));
#43227=CARTESIAN_POINT('',(0.156070932745934,-0.596521174907684,5.37));
#43228=CARTESIAN_POINT('',(0.156070932745934,-0.596521174907684,5.4));
#43229=CARTESIAN_POINT('',(0.166950926184654,-0.528990542888641,5.37));
#43230=CARTESIAN_POINT('Ctrl Pts',(0.156070932745934,-0.596521174907684,
5.37));
#43231=CARTESIAN_POINT('Ctrl Pts',(0.166950926184654,-0.573635852336884,
5.37));
#43232=CARTESIAN_POINT('Ctrl Pts',(0.166950926184654,-0.528990542888641,
5.37));
#43233=CARTESIAN_POINT('',(0.166950926184654,-0.528990542888641,5.4));
#43234=CARTESIAN_POINT('Ctrl Pts',(0.111425623297691,-0.643229997158051,
5.4));
#43235=CARTESIAN_POINT('Ctrl Pts',(0.111425623297691,-0.643229997158051,
5.37));
#43236=CARTESIAN_POINT('Ctrl Pts',(0.141814455389977,-0.626159703731537,
5.4));
#43237=CARTESIAN_POINT('Ctrl Pts',(0.141814455389977,-0.626159703731537,
5.37));
#43238=CARTESIAN_POINT('Ctrl Pts',(0.156070932745934,-0.596521174907684,
5.4));
#43239=CARTESIAN_POINT('Ctrl Pts',(0.156070932745934,-0.596521174907684,
5.37));
#43240=CARTESIAN_POINT('',(0.111425623297691,-0.643229997158051,5.4));
#43241=CARTESIAN_POINT('Ctrl Pts',(0.111425623297691,-0.643229997158051,
5.4));
#43242=CARTESIAN_POINT('Ctrl Pts',(0.141814455389977,-0.626159703731537,
5.4));
#43243=CARTESIAN_POINT('Ctrl Pts',(0.156070932745934,-0.596521174907684,
5.4));
#43244=CARTESIAN_POINT('',(0.111425623297691,-0.643229997158051,5.37));
#43245=CARTESIAN_POINT('',(0.111425623297691,-0.643229997158051,5.4));
#43246=CARTESIAN_POINT('Ctrl Pts',(0.111425623297691,-0.643229997158051,
5.37));
#43247=CARTESIAN_POINT('Ctrl Pts',(0.141814455389977,-0.626159703731537,
5.37));
#43248=CARTESIAN_POINT('Ctrl Pts',(0.156070932745934,-0.596521174907684,
5.37));
#43249=CARTESIAN_POINT('Ctrl Pts',(0.0420191138982773,-0.660300171375275,
5.4));
#43250=CARTESIAN_POINT('Ctrl Pts',(0.0420191138982773,-0.660300171375275,
5.37));
#43251=CARTESIAN_POINT('Ctrl Pts',(0.0810367912054062,-0.660300171375275,
5.4));
#43252=CARTESIAN_POINT('Ctrl Pts',(0.0810367912054062,-0.660300171375275,
5.37));
#43253=CARTESIAN_POINT('Ctrl Pts',(0.111425623297691,-0.643229997158051,
5.4));
#43254=CARTESIAN_POINT('Ctrl Pts',(0.111425623297691,-0.643229997158051,
5.37));
#43255=CARTESIAN_POINT('',(0.0420191138982773,-0.660300171375275,5.4));
#43256=CARTESIAN_POINT('Ctrl Pts',(0.0420191138982773,-0.660300171375275,
5.4));
#43257=CARTESIAN_POINT('Ctrl Pts',(0.0810367912054062,-0.660300171375275,
5.4));
#43258=CARTESIAN_POINT('Ctrl Pts',(0.111425623297691,-0.643229997158051,
5.4));
#43259=CARTESIAN_POINT('',(0.0420191138982773,-0.660300171375275,5.37));
#43260=CARTESIAN_POINT('',(0.0420191138982773,-0.660300171375275,5.4));
#43261=CARTESIAN_POINT('Ctrl Pts',(0.0420191138982773,-0.660300171375275,
5.37));
#43262=CARTESIAN_POINT('Ctrl Pts',(0.0810367912054062,-0.660300171375275,
5.37));
#43263=CARTESIAN_POINT('Ctrl Pts',(0.111425623297691,-0.643229997158051,
5.37));
#43264=CARTESIAN_POINT('Ctrl Pts',(-0.0178206115961075,-0.642292058467865,
5.4));
#43265=CARTESIAN_POINT('Ctrl Pts',(-0.0178206115961075,-0.642292058467865,
5.37));
#43266=CARTESIAN_POINT('Ctrl Pts',(0.00262616574764252,-0.660300171375275,
5.4));
#43267=CARTESIAN_POINT('Ctrl Pts',(0.00262616574764252,-0.660300171375275,
5.37));
#43268=CARTESIAN_POINT('Ctrl Pts',(0.0420191138982773,-0.660300171375275,
5.4));
#43269=CARTESIAN_POINT('Ctrl Pts',(0.0420191138982773,-0.660300171375275,
5.37));
#43270=CARTESIAN_POINT('',(-0.0178206115961075,-0.642292058467865,5.4));
#43271=CARTESIAN_POINT('Ctrl Pts',(-0.0178206115961075,-0.642292058467865,
5.4));
#43272=CARTESIAN_POINT('Ctrl Pts',(0.00262616574764252,-0.660300171375275,
5.4));
#43273=CARTESIAN_POINT('Ctrl Pts',(0.0420191138982773,-0.660300171375275,
5.4));
#43274=CARTESIAN_POINT('',(-0.0178206115961075,-0.642292058467865,5.37));
#43275=CARTESIAN_POINT('',(-0.0178206115961075,-0.642292058467865,5.4));
#43276=CARTESIAN_POINT('Ctrl Pts',(-0.0178206115961075,-0.642292058467865,
5.37));
#43277=CARTESIAN_POINT('Ctrl Pts',(0.00262616574764252,-0.660300171375275,
5.37));
#43278=CARTESIAN_POINT('Ctrl Pts',(0.0420191138982773,-0.660300171375275,
5.37));
#43279=CARTESIAN_POINT('Ctrl Pts',(-0.0382673889398575,-0.597271597385406,
5.4));
#43280=CARTESIAN_POINT('Ctrl Pts',(-0.0382673889398575,-0.597271597385406,
5.37));
#43281=CARTESIAN_POINT('Ctrl Pts',(-0.0382673889398575,-0.624283826351166,
5.4));
#43282=CARTESIAN_POINT('Ctrl Pts',(-0.0382673889398575,-0.624283826351166,
5.37));
#43283=CARTESIAN_POINT('Ctrl Pts',(-0.0178206115961075,-0.642292058467865,
5.4));
#43284=CARTESIAN_POINT('Ctrl Pts',(-0.0178206115961075,-0.642292058467865,
5.37));
#43285=CARTESIAN_POINT('',(-0.0382673889398575,-0.597271597385406,5.4));
#43286=CARTESIAN_POINT('Ctrl Pts',(-0.0382673889398575,-0.597271597385406,
5.4));
#43287=CARTESIAN_POINT('Ctrl Pts',(-0.0382673889398575,-0.624283826351166,
5.4));
#43288=CARTESIAN_POINT('Ctrl Pts',(-0.0178206115961075,-0.642292058467865,
5.4));
#43289=CARTESIAN_POINT('',(-0.0382673889398575,-0.597271597385406,5.37));
#43290=CARTESIAN_POINT('',(-0.0382673889398575,-0.597271597385406,5.4));
#43291=CARTESIAN_POINT('Ctrl Pts',(-0.0382673889398575,-0.597271597385406,
5.37));
#43292=CARTESIAN_POINT('Ctrl Pts',(-0.0382673889398575,-0.624283826351166,
5.37));
#43293=CARTESIAN_POINT('Ctrl Pts',(-0.0178206115961075,-0.642292058467865,
5.37));
#43294=CARTESIAN_POINT('Ctrl Pts',(-0.0288882404565811,-0.565194523334503,
5.4));
#43295=CARTESIAN_POINT('Ctrl Pts',(-0.0288882404565811,-0.565194523334503,
5.37));
#43296=CARTESIAN_POINT('Ctrl Pts',(-0.0382673889398575,-0.579638516902924,
5.4));
#43297=CARTESIAN_POINT('Ctrl Pts',(-0.0382673889398575,-0.579638516902924,
5.37));
#43298=CARTESIAN_POINT('Ctrl Pts',(-0.0382673889398575,-0.597271597385406,
5.4));
#43299=CARTESIAN_POINT('Ctrl Pts',(-0.0382673889398575,-0.597271597385406,
5.37));
#43300=CARTESIAN_POINT('',(-0.0288882404565811,-0.565194523334503,5.4));
#43301=CARTESIAN_POINT('Ctrl Pts',(-0.0288882404565811,-0.565194523334503,
5.4));
#43302=CARTESIAN_POINT('Ctrl Pts',(-0.0382673889398575,-0.579638516902924,
5.4));
#43303=CARTESIAN_POINT('Ctrl Pts',(-0.0382673889398575,-0.597271597385406,
5.4));
#43304=CARTESIAN_POINT('',(-0.0288882404565811,-0.565194523334503,5.37));
#43305=CARTESIAN_POINT('',(-0.0288882404565811,-0.565194523334503,5.4));
#43306=CARTESIAN_POINT('Ctrl Pts',(-0.0288882404565811,-0.565194523334503,
5.37));
#43307=CARTESIAN_POINT('Ctrl Pts',(-0.0382673889398575,-0.579638516902924,
5.37));
#43308=CARTESIAN_POINT('Ctrl Pts',(-0.0382673889398575,-0.597271597385406,
5.37));
#43309=CARTESIAN_POINT('Ctrl Pts',(-0.00225116312503815,-0.543247020244598,
5.4));
#43310=CARTESIAN_POINT('Ctrl Pts',(-0.00225116312503815,-0.543247020244598,
5.37));
#43311=CARTESIAN_POINT('Ctrl Pts',(-0.0195088535547256,-0.550750410556793,
5.4));
#43312=CARTESIAN_POINT('Ctrl Pts',(-0.0195088535547256,-0.550750410556793,
5.37));
#43313=CARTESIAN_POINT('Ctrl Pts',(-0.0288882404565811,-0.565194523334503,
5.4));
#43314=CARTESIAN_POINT('Ctrl Pts',(-0.0288882404565811,-0.565194523334503,
5.37));
#43315=CARTESIAN_POINT('',(-0.00225116312503815,-0.543247020244598,5.4));
#43316=CARTESIAN_POINT('Ctrl Pts',(-0.00225116312503815,-0.543247020244598,
5.4));
#43317=CARTESIAN_POINT('Ctrl Pts',(-0.0195088535547256,-0.550750410556793,
5.4));
#43318=CARTESIAN_POINT('Ctrl Pts',(-0.0288882404565811,-0.565194523334503,
5.4));
#43319=CARTESIAN_POINT('',(-0.00225116312503815,-0.543247020244598,5.37));
#43320=CARTESIAN_POINT('',(-0.00225116312503815,-0.543247020244598,5.4));
#43321=CARTESIAN_POINT('Ctrl Pts',(-0.00225116312503815,-0.543247020244598,
5.37));
#43322=CARTESIAN_POINT('Ctrl Pts',(-0.0195088535547256,-0.550750410556793,
5.37));
#43323=CARTESIAN_POINT('Ctrl Pts',(-0.0288882404565811,-0.565194523334503,
5.37));
#43324=CARTESIAN_POINT('Ctrl Pts',(0.0566506236791611,-0.529740846157074,
5.4));
#43325=CARTESIAN_POINT('Ctrl Pts',(0.0566506236791611,-0.529740846157074,
5.37));
#43326=CARTESIAN_POINT('Ctrl Pts',(0.0150067657232285,-0.535743629932404,
5.4));
#43327=CARTESIAN_POINT('Ctrl Pts',(0.0150067657232285,-0.535743629932404,
5.37));
#43328=CARTESIAN_POINT('Ctrl Pts',(-0.00225116312503815,-0.543247020244598,
5.4));
#43329=CARTESIAN_POINT('Ctrl Pts',(-0.00225116312503815,-0.543247020244598,
5.37));
#43330=CARTESIAN_POINT('',(0.0566506236791611,-0.529740846157074,5.4));
#43331=CARTESIAN_POINT('Ctrl Pts',(0.0566506236791611,-0.529740846157074,
5.4));
#43332=CARTESIAN_POINT('Ctrl Pts',(0.0150067657232285,-0.535743629932404,
5.4));
#43333=CARTESIAN_POINT('Ctrl Pts',(-0.00225116312503815,-0.543247020244598,
5.4));
#43334=CARTESIAN_POINT('',(0.0566506236791611,-0.529740846157074,5.37));
#43335=CARTESIAN_POINT('',(0.0566506236791611,-0.529740846157074,5.4));
#43336=CARTESIAN_POINT('Ctrl Pts',(0.0566506236791611,-0.529740846157074,
5.37));
#43337=CARTESIAN_POINT('Ctrl Pts',(0.0150067657232285,-0.535743629932404,
5.37));
#43338=CARTESIAN_POINT('Ctrl Pts',(-0.00225116312503815,-0.543247020244598,
5.37));
#43339=CARTESIAN_POINT('Ctrl Pts',(0.166950926184654,-0.50422922372818,
5.4));
#43340=CARTESIAN_POINT('Ctrl Pts',(0.166950926184654,-0.50422922372818,
5.37));
#43341=CARTESIAN_POINT('Ctrl Pts',(0.130184158682823,-0.519236123561859,
5.4));
#43342=CARTESIAN_POINT('Ctrl Pts',(0.130184158682823,-0.519236123561859,
5.37));
#43343=CARTESIAN_POINT('Ctrl Pts',(0.0566506236791611,-0.529740846157074,
5.4));
#43344=CARTESIAN_POINT('Ctrl Pts',(0.0566506236791611,-0.529740846157074,
5.37));
#43345=CARTESIAN_POINT('',(0.166950926184654,-0.50422922372818,5.4));
#43346=CARTESIAN_POINT('Ctrl Pts',(0.166950926184654,-0.50422922372818,
5.4));
#43347=CARTESIAN_POINT('Ctrl Pts',(0.130184158682823,-0.519236123561859,
5.4));
#43348=CARTESIAN_POINT('Ctrl Pts',(0.0566506236791611,-0.529740846157074,
5.4));
#43349=CARTESIAN_POINT('',(0.166950926184654,-0.50422922372818,5.37));
#43350=CARTESIAN_POINT('',(0.166950926184654,-0.50422922372818,5.4));
#43351=CARTESIAN_POINT('Ctrl Pts',(0.166950926184654,-0.50422922372818,
5.37));
#43352=CARTESIAN_POINT('Ctrl Pts',(0.130184158682823,-0.519236123561859,
5.37));
#43353=CARTESIAN_POINT('Ctrl Pts',(0.0566506236791611,-0.529740846157074,
5.37));
#43354=CARTESIAN_POINT('Origin',(0.166950926184654,-0.528990542888641,5.4));
#43355=CARTESIAN_POINT('',(0.166950926184654,-0.264495271444321,5.4));
#43356=CARTESIAN_POINT('',(0.166950926184654,-0.528990542888641,5.37));
#43357=CARTESIAN_POINT('Ctrl Pts',(0.239546284079552,-0.656360900402069,
5.4));
#43358=CARTESIAN_POINT('Ctrl Pts',(0.239546284079552,-0.656360900402069,
5.37));
#43359=CARTESIAN_POINT('Ctrl Pts',(0.243860706686974,-0.681309735774994,
5.4));
#43360=CARTESIAN_POINT('Ctrl Pts',(0.243860706686974,-0.681309735774994,
5.37));
#43361=CARTESIAN_POINT('Ctrl Pts',(0.256616577506065,-0.704195177555084,
5.4));
#43362=CARTESIAN_POINT('Ctrl Pts',(0.256616577506065,-0.704195177555084,
5.37));
#43363=CARTESIAN_POINT('',(0.239546284079552,-0.656360900402069,5.4));
#43364=CARTESIAN_POINT('',(0.256616577506065,-0.704195177555084,5.4));
#43365=CARTESIAN_POINT('Ctrl Pts',(0.239546284079552,-0.656360900402069,
5.4));
#43366=CARTESIAN_POINT('Ctrl Pts',(0.243860706686974,-0.681309735774994,
5.4));
#43367=CARTESIAN_POINT('Ctrl Pts',(0.256616577506065,-0.704195177555084,
5.4));
#43368=CARTESIAN_POINT('',(0.239546284079552,-0.656360900402069,5.37));
#43369=CARTESIAN_POINT('',(0.239546284079552,-0.656360900402069,5.4));
#43370=CARTESIAN_POINT('',(0.256616577506065,-0.704195177555084,5.37));
#43371=CARTESIAN_POINT('Ctrl Pts',(0.239546284079552,-0.656360900402069,
5.37));
#43372=CARTESIAN_POINT('Ctrl Pts',(0.243860706686974,-0.681309735774994,
5.37));
#43373=CARTESIAN_POINT('Ctrl Pts',(0.256616577506065,-0.704195177555084,
5.37));
#43374=CARTESIAN_POINT('',(0.256616577506065,-0.704195177555084,5.4));
#43375=CARTESIAN_POINT('Ctrl Pts',(0.23523186147213,-0.537244236469269,
5.4));
#43376=CARTESIAN_POINT('Ctrl Pts',(0.23523186147213,-0.537244236469269,
5.37));
#43377=CARTESIAN_POINT('Ctrl Pts',(0.23523186147213,-0.631412065029144,
5.4));
#43378=CARTESIAN_POINT('Ctrl Pts',(0.23523186147213,-0.631412065029144,
5.37));
#43379=CARTESIAN_POINT('Ctrl Pts',(0.239546284079552,-0.656360900402069,
5.4));
#43380=CARTESIAN_POINT('Ctrl Pts',(0.239546284079552,-0.656360900402069,
5.37));
#43381=CARTESIAN_POINT('',(0.23523186147213,-0.537244236469269,5.4));
#43382=CARTESIAN_POINT('Ctrl Pts',(0.23523186147213,-0.537244236469269,
5.4));
#43383=CARTESIAN_POINT('Ctrl Pts',(0.23523186147213,-0.631412065029144,
5.4));
#43384=CARTESIAN_POINT('Ctrl Pts',(0.239546284079552,-0.656360900402069,
5.4));
#43385=CARTESIAN_POINT('',(0.23523186147213,-0.537244236469269,5.37));
#43386=CARTESIAN_POINT('',(0.23523186147213,-0.537244236469269,5.4));
#43387=CARTESIAN_POINT('Ctrl Pts',(0.23523186147213,-0.537244236469269,
5.37));
#43388=CARTESIAN_POINT('Ctrl Pts',(0.23523186147213,-0.631412065029144,
5.37));
#43389=CARTESIAN_POINT('Ctrl Pts',(0.239546284079552,-0.656360900402069,
5.37));
#43390=CARTESIAN_POINT('Origin',(0.23523186147213,-0.447203314304352,5.4));
#43391=CARTESIAN_POINT('',(0.23523186147213,-0.447203314304352,5.4));
#43392=CARTESIAN_POINT('',(0.23523186147213,-0.223601657152176,5.4));
#43393=CARTESIAN_POINT('',(0.23523186147213,-0.447203314304352,5.37));
#43394=CARTESIAN_POINT('',(0.23523186147213,-0.447203314304352,5.4));
#43395=CARTESIAN_POINT('',(0.23523186147213,-0.447203314304352,5.37));
#43396=CARTESIAN_POINT('Ctrl Pts',(0.231855377554893,-0.384925043582916,
5.4));
#43397=CARTESIAN_POINT('Ctrl Pts',(0.231855377554893,-0.384925043582916,
5.37));
#43398=CARTESIAN_POINT('Ctrl Pts',(0.23523186147213,-0.402182853221893,
5.4));
#43399=CARTESIAN_POINT('Ctrl Pts',(0.23523186147213,-0.402182853221893,
5.37));
#43400=CARTESIAN_POINT('Ctrl Pts',(0.23523186147213,-0.447203314304352,
5.4));
#43401=CARTESIAN_POINT('Ctrl Pts',(0.23523186147213,-0.447203314304352,
5.37));
#43402=CARTESIAN_POINT('',(0.231855377554893,-0.384925043582916,5.4));
#43403=CARTESIAN_POINT('Ctrl Pts',(0.231855377554893,-0.384925043582916,
5.4));
#43404=CARTESIAN_POINT('Ctrl Pts',(0.23523186147213,-0.402182853221893,
5.4));
#43405=CARTESIAN_POINT('Ctrl Pts',(0.23523186147213,-0.447203314304352,
5.4));
#43406=CARTESIAN_POINT('',(0.231855377554893,-0.384925043582916,5.37));
#43407=CARTESIAN_POINT('',(0.231855377554893,-0.384925043582916,5.4));
#43408=CARTESIAN_POINT('Ctrl Pts',(0.231855377554893,-0.384925043582916,
5.37));
#43409=CARTESIAN_POINT('Ctrl Pts',(0.23523186147213,-0.402182853221893,
5.37));
#43410=CARTESIAN_POINT('Ctrl Pts',(0.23523186147213,-0.447203314304352,
5.37));
#43411=CARTESIAN_POINT('Ctrl Pts',(0.210845932364464,-0.338966643810272,
5.4));
#43412=CARTESIAN_POINT('Ctrl Pts',(0.210845932364464,-0.338966643810272,
5.37));
#43413=CARTESIAN_POINT('Ctrl Pts',(0.225852712988853,-0.357162392139435,
5.4));
#43414=CARTESIAN_POINT('Ctrl Pts',(0.225852712988853,-0.357162392139435,
5.37));
#43415=CARTESIAN_POINT('Ctrl Pts',(0.231855377554893,-0.384925043582916,
5.4));
#43416=CARTESIAN_POINT('Ctrl Pts',(0.231855377554893,-0.384925043582916,
5.37));
#43417=CARTESIAN_POINT('',(0.210845932364464,-0.338966643810272,5.4));
#43418=CARTESIAN_POINT('Ctrl Pts',(0.210845932364464,-0.338966643810272,
5.4));
#43419=CARTESIAN_POINT('Ctrl Pts',(0.225852712988853,-0.357162392139435,
5.4));
#43420=CARTESIAN_POINT('Ctrl Pts',(0.231855377554893,-0.384925043582916,
5.4));
#43421=CARTESIAN_POINT('',(0.210845932364464,-0.338966643810272,5.37));
#43422=CARTESIAN_POINT('',(0.210845932364464,-0.338966643810272,5.4));
#43423=CARTESIAN_POINT('Ctrl Pts',(0.210845932364464,-0.338966643810272,
5.37));
#43424=CARTESIAN_POINT('Ctrl Pts',(0.225852712988853,-0.357162392139435,
5.37));
#43425=CARTESIAN_POINT('Ctrl Pts',(0.231855377554893,-0.384925043582916,
5.37));
#43426=CARTESIAN_POINT('Ctrl Pts',(0.163949474692345,-0.30876544713974,
5.4));
#43427=CARTESIAN_POINT('Ctrl Pts',(0.163949474692345,-0.30876544713974,
5.37));
#43428=CARTESIAN_POINT('Ctrl Pts',(0.195838913321495,-0.32077089548111,
5.4));
#43429=CARTESIAN_POINT('Ctrl Pts',(0.195838913321495,-0.32077089548111,
5.37));
#43430=CARTESIAN_POINT('Ctrl Pts',(0.210845932364464,-0.338966643810272,
5.4));
#43431=CARTESIAN_POINT('Ctrl Pts',(0.210845932364464,-0.338966643810272,
5.37));
#43432=CARTESIAN_POINT('',(0.163949474692345,-0.30876544713974,5.4));
#43433=CARTESIAN_POINT('Ctrl Pts',(0.163949474692345,-0.30876544713974,
5.4));
#43434=CARTESIAN_POINT('Ctrl Pts',(0.195838913321495,-0.32077089548111,
5.4));
#43435=CARTESIAN_POINT('Ctrl Pts',(0.210845932364464,-0.338966643810272,
5.4));
#43436=CARTESIAN_POINT('',(0.163949474692345,-0.30876544713974,5.37));
#43437=CARTESIAN_POINT('',(0.163949474692345,-0.30876544713974,5.4));
#43438=CARTESIAN_POINT('Ctrl Pts',(0.163949474692345,-0.30876544713974,
5.37));
#43439=CARTESIAN_POINT('Ctrl Pts',(0.195838913321495,-0.32077089548111,
5.37));
#43440=CARTESIAN_POINT('Ctrl Pts',(0.210845932364464,-0.338966643810272,
5.37));
#43441=CARTESIAN_POINT('Ctrl Pts',(0.0810367912054062,-0.296759939193726,
5.4));
#43442=CARTESIAN_POINT('Ctrl Pts',(0.0810367912054062,-0.296759939193726,
5.37));
#43443=CARTESIAN_POINT('Ctrl Pts',(0.132060036063194,-0.296759939193726,
5.4));
#43444=CARTESIAN_POINT('Ctrl Pts',(0.132060036063194,-0.296759939193726,
5.37));
#43445=CARTESIAN_POINT('Ctrl Pts',(0.163949474692345,-0.30876544713974,
5.4));
#43446=CARTESIAN_POINT('Ctrl Pts',(0.163949474692345,-0.30876544713974,
5.37));
#43447=CARTESIAN_POINT('',(0.0810367912054062,-0.296759939193726,5.4));
#43448=CARTESIAN_POINT('Ctrl Pts',(0.0810367912054062,-0.296759939193726,
5.4));
#43449=CARTESIAN_POINT('Ctrl Pts',(0.132060036063194,-0.296759939193726,
5.4));
#43450=CARTESIAN_POINT('Ctrl Pts',(0.163949474692345,-0.30876544713974,
5.4));
#43451=CARTESIAN_POINT('',(0.0810367912054062,-0.296759939193726,5.37));
#43452=CARTESIAN_POINT('',(0.0810367912054062,-0.296759939193726,5.4));
#43453=CARTESIAN_POINT('Ctrl Pts',(0.0810367912054062,-0.296759939193726,
5.37));
#43454=CARTESIAN_POINT('Ctrl Pts',(0.132060036063194,-0.296759939193726,
5.37));
#43455=CARTESIAN_POINT('Ctrl Pts',(0.163949474692345,-0.30876544713974,
5.37));
#43456=CARTESIAN_POINT('Ctrl Pts',(-0.00937940180301666,-0.310828840732574,
5.4));
#43457=CARTESIAN_POINT('Ctrl Pts',(-0.00937940180301666,-0.310828840732574,
5.37));
#43458=CARTESIAN_POINT('Ctrl Pts',(0.0296385139226913,-0.296759939193726,
5.4));
#43459=CARTESIAN_POINT('Ctrl Pts',(0.0296385139226913,-0.296759939193726,
5.37));
#43460=CARTESIAN_POINT('Ctrl Pts',(0.0810367912054062,-0.296759939193726,
5.4));
#43461=CARTESIAN_POINT('Ctrl Pts',(0.0810367912054062,-0.296759939193726,
5.37));
#43462=CARTESIAN_POINT('',(-0.00937940180301666,-0.310828840732574,5.4));
#43463=CARTESIAN_POINT('Ctrl Pts',(-0.00937940180301666,-0.310828840732574,
5.4));
#43464=CARTESIAN_POINT('Ctrl Pts',(0.0296385139226913,-0.296759939193726,
5.4));
#43465=CARTESIAN_POINT('Ctrl Pts',(0.0810367912054062,-0.296759939193726,
5.4));
#43466=CARTESIAN_POINT('',(-0.00937940180301666,-0.310828840732574,5.37));
#43467=CARTESIAN_POINT('',(-0.00937940180301666,-0.310828840732574,5.4));
#43468=CARTESIAN_POINT('Ctrl Pts',(-0.00937940180301666,-0.310828840732574,
5.37));
#43469=CARTESIAN_POINT('Ctrl Pts',(0.0296385139226913,-0.296759939193726,
5.37));
#43470=CARTESIAN_POINT('Ctrl Pts',(0.0810367912054062,-0.296759939193726,
5.37));
#43471=CARTESIAN_POINT('Ctrl Pts',(-0.0690312534570694,-0.350972092151642,
5.4));
#43472=CARTESIAN_POINT('Ctrl Pts',(-0.0690312534570694,-0.350972092151642,
5.37));
#43473=CARTESIAN_POINT('Ctrl Pts',(-0.0483970791101456,-0.324897742271423,
5.4));
#43474=CARTESIAN_POINT('Ctrl Pts',(-0.0483970791101456,-0.324897742271423,
5.37));
#43475=CARTESIAN_POINT('Ctrl Pts',(-0.00937940180301666,-0.310828840732574,
5.4));
#43476=CARTESIAN_POINT('Ctrl Pts',(-0.00937940180301666,-0.310828840732574,
5.37));
#43477=CARTESIAN_POINT('',(-0.0690312534570694,-0.350972092151642,5.4));
#43478=CARTESIAN_POINT('Ctrl Pts',(-0.0690312534570694,-0.350972092151642,
5.4));
#43479=CARTESIAN_POINT('Ctrl Pts',(-0.0483970791101456,-0.324897742271423,
5.4));
#43480=CARTESIAN_POINT('Ctrl Pts',(-0.00937940180301666,-0.310828840732574,
5.4));
#43481=CARTESIAN_POINT('',(-0.0690312534570694,-0.350972092151642,5.37));
#43482=CARTESIAN_POINT('',(-0.0690312534570694,-0.350972092151642,5.4));
#43483=CARTESIAN_POINT('Ctrl Pts',(-0.0690312534570694,-0.350972092151642,
5.37));
#43484=CARTESIAN_POINT('Ctrl Pts',(-0.0483970791101456,-0.324897742271423,
5.37));
#43485=CARTESIAN_POINT('Ctrl Pts',(-0.00937940180301666,-0.310828840732574,
5.37));
#43486=CARTESIAN_POINT('Ctrl Pts',(-0.0986697822809219,-0.419440722465515,
5.4));
#43487=CARTESIAN_POINT('Ctrl Pts',(-0.0986697822809219,-0.419440722465515,
5.37));
#43488=CARTESIAN_POINT('Ctrl Pts',(-0.0896656662225723,-0.37704644203186,
5.4));
#43489=CARTESIAN_POINT('Ctrl Pts',(-0.0896656662225723,-0.37704644203186,
5.37));
#43490=CARTESIAN_POINT('Ctrl Pts',(-0.0690312534570694,-0.350972092151642,
5.4));
#43491=CARTESIAN_POINT('Ctrl Pts',(-0.0690312534570694,-0.350972092151642,
5.37));
#43492=CARTESIAN_POINT('',(-0.0986697822809219,-0.419440722465515,5.4));
#43493=CARTESIAN_POINT('Ctrl Pts',(-0.0986697822809219,-0.419440722465515,
5.4));
#43494=CARTESIAN_POINT('Ctrl Pts',(-0.0896656662225723,-0.37704644203186,
5.4));
#43495=CARTESIAN_POINT('Ctrl Pts',(-0.0690312534570694,-0.350972092151642,
5.4));
#43496=CARTESIAN_POINT('',(-0.0986697822809219,-0.419440722465515,5.37));
#43497=CARTESIAN_POINT('',(-0.0986697822809219,-0.419440722465515,5.4));
#43498=CARTESIAN_POINT('Ctrl Pts',(-0.0986697822809219,-0.419440722465515,
5.37));
#43499=CARTESIAN_POINT('Ctrl Pts',(-0.0896656662225723,-0.37704644203186,
5.37));
#43500=CARTESIAN_POINT('Ctrl Pts',(-0.0690312534570694,-0.350972092151642,
5.37));
#43501=CARTESIAN_POINT('Origin',(-0.0326397567987442,-0.42844477891922,
5.4));
#43502=CARTESIAN_POINT('',(-0.0326397567987442,-0.42844477891922,5.4));
#43503=CARTESIAN_POINT('',(-0.0452965477902544,-0.426718860145479,5.4));
#43504=CARTESIAN_POINT('',(-0.0326397567987442,-0.42844477891922,5.37));
#43505=CARTESIAN_POINT('',(-0.0326397567987442,-0.42844477891922,5.4));
#43506=CARTESIAN_POINT('',(-0.0326397567987442,-0.42844477891922,5.37));
#43507=CARTESIAN_POINT('Ctrl Pts',(0.000937923789024353,-0.369355475902557,
5.4));
#43508=CARTESIAN_POINT('Ctrl Pts',(0.000937923789024353,-0.369355475902557,
5.37));
#43509=CARTESIAN_POINT('Ctrl Pts',(-0.0217600017786026,-0.386050498485565,
5.4));
#43510=CARTESIAN_POINT('Ctrl Pts',(-0.0217600017786026,-0.386050498485565,
5.37));
#43511=CARTESIAN_POINT('Ctrl Pts',(-0.0326397567987442,-0.42844477891922,
5.4));
#43512=CARTESIAN_POINT('Ctrl Pts',(-0.0326397567987442,-0.42844477891922,
5.37));
#43513=CARTESIAN_POINT('',(0.000937923789024353,-0.369355475902557,5.4));
#43514=CARTESIAN_POINT('Ctrl Pts',(0.000937923789024353,-0.369355475902557,
5.4));
#43515=CARTESIAN_POINT('Ctrl Pts',(-0.0217600017786026,-0.386050498485565,
5.4));
#43516=CARTESIAN_POINT('Ctrl Pts',(-0.0326397567987442,-0.42844477891922,
5.4));
#43517=CARTESIAN_POINT('',(0.000937923789024353,-0.369355475902557,5.37));
#43518=CARTESIAN_POINT('',(0.000937923789024353,-0.369355475902557,5.4));
#43519=CARTESIAN_POINT('Ctrl Pts',(0.000937923789024353,-0.369355475902557,
5.37));
#43520=CARTESIAN_POINT('Ctrl Pts',(-0.0217600017786026,-0.386050498485565,
5.37));
#43521=CARTESIAN_POINT('Ctrl Pts',(-0.0326397567987442,-0.42844477891922,
5.37));
#43522=CARTESIAN_POINT('Ctrl Pts',(0.071282371878624,-0.35266033411026,
5.4));
#43523=CARTESIAN_POINT('Ctrl Pts',(0.071282371878624,-0.35266033411026,
5.37));
#43524=CARTESIAN_POINT('Ctrl Pts',(0.0236358493566513,-0.35266033411026,
5.4));
#43525=CARTESIAN_POINT('Ctrl Pts',(0.0236358493566513,-0.35266033411026,
5.37));
#43526=CARTESIAN_POINT('Ctrl Pts',(0.000937923789024353,-0.369355475902557,
5.4));
#43527=CARTESIAN_POINT('Ctrl Pts',(0.000937923789024353,-0.369355475902557,
5.37));
#43528=CARTESIAN_POINT('',(0.071282371878624,-0.35266033411026,5.4));
#43529=CARTESIAN_POINT('Ctrl Pts',(0.071282371878624,-0.35266033411026,
5.4));
#43530=CARTESIAN_POINT('Ctrl Pts',(0.0236358493566513,-0.35266033411026,
5.4));
#43531=CARTESIAN_POINT('Ctrl Pts',(0.000937923789024353,-0.369355475902557,
5.4));
#43532=CARTESIAN_POINT('',(0.071282371878624,-0.35266033411026,5.37));
#43533=CARTESIAN_POINT('',(0.071282371878624,-0.35266033411026,5.4));
#43534=CARTESIAN_POINT('Ctrl Pts',(0.071282371878624,-0.35266033411026,
5.37));
#43535=CARTESIAN_POINT('Ctrl Pts',(0.0236358493566513,-0.35266033411026,
5.37));
#43536=CARTESIAN_POINT('Ctrl Pts',(0.000937923789024353,-0.369355475902557,
5.37));
#43537=CARTESIAN_POINT('Ctrl Pts',(0.148192390799522,-0.37554577589035,
5.4));
#43538=CARTESIAN_POINT('Ctrl Pts',(0.148192390799522,-0.37554577589035,
5.37));
#43539=CARTESIAN_POINT('Ctrl Pts',(0.122305616736412,-0.35266033411026,
5.4));
#43540=CARTESIAN_POINT('Ctrl Pts',(0.122305616736412,-0.35266033411026,
5.37));
#43541=CARTESIAN_POINT('Ctrl Pts',(0.071282371878624,-0.35266033411026,
5.4));
#43542=CARTESIAN_POINT('Ctrl Pts',(0.071282371878624,-0.35266033411026,
5.37));
#43543=CARTESIAN_POINT('',(0.148192390799522,-0.37554577589035,5.4));
#43544=CARTESIAN_POINT('Ctrl Pts',(0.148192390799522,-0.37554577589035,
5.4));
#43545=CARTESIAN_POINT('Ctrl Pts',(0.122305616736412,-0.35266033411026,
5.4));
#43546=CARTESIAN_POINT('Ctrl Pts',(0.071282371878624,-0.35266033411026,
5.4));
#43547=CARTESIAN_POINT('',(0.148192390799522,-0.37554577589035,5.37));
#43548=CARTESIAN_POINT('',(0.148192390799522,-0.37554577589035,5.4));
#43549=CARTESIAN_POINT('Ctrl Pts',(0.148192390799522,-0.37554577589035,
5.37));
#43550=CARTESIAN_POINT('Ctrl Pts',(0.122305616736412,-0.35266033411026,
5.37));
#43551=CARTESIAN_POINT('Ctrl Pts',(0.071282371878624,-0.35266033411026,
5.37));
#43552=CARTESIAN_POINT('Ctrl Pts',(0.167325958609581,-0.433697199821472,
5.4));
#43553=CARTESIAN_POINT('Ctrl Pts',(0.167325958609581,-0.433697199821472,
5.37));
#43554=CARTESIAN_POINT('Ctrl Pts',(0.167325958609581,-0.392428433895111,
5.4));
#43555=CARTESIAN_POINT('Ctrl Pts',(0.167325958609581,-0.392428433895111,
5.37));
#43556=CARTESIAN_POINT('Ctrl Pts',(0.148192390799522,-0.37554577589035,
5.4));
#43557=CARTESIAN_POINT('Ctrl Pts',(0.148192390799522,-0.37554577589035,
5.37));
#43558=CARTESIAN_POINT('',(0.167325958609581,-0.433697199821472,5.4));
#43559=CARTESIAN_POINT('Ctrl Pts',(0.167325958609581,-0.433697199821472,
5.4));
#43560=CARTESIAN_POINT('Ctrl Pts',(0.167325958609581,-0.392428433895111,
5.4));
#43561=CARTESIAN_POINT('Ctrl Pts',(0.148192390799522,-0.37554577589035,
5.4));
#43562=CARTESIAN_POINT('',(0.167325958609581,-0.433697199821472,5.37));
#43563=CARTESIAN_POINT('',(0.167325958609581,-0.433697199821472,5.4));
#43564=CARTESIAN_POINT('Ctrl Pts',(0.167325958609581,-0.433697199821472,
5.37));
#43565=CARTESIAN_POINT('Ctrl Pts',(0.167325958609581,-0.392428433895111,
5.37));
#43566=CARTESIAN_POINT('Ctrl Pts',(0.148192390799522,-0.37554577589035,
5.37));
#43567=CARTESIAN_POINT('Ctrl Pts',(0.166950926184654,-0.45133022069931,
5.4));
#43568=CARTESIAN_POINT('Ctrl Pts',(0.166950926184654,-0.45133022069931,
5.37));
#43569=CARTESIAN_POINT('Ctrl Pts',(0.167325958609581,-0.43744889497757,
5.4));
#43570=CARTESIAN_POINT('Ctrl Pts',(0.167325958609581,-0.43744889497757,
5.37));
#43571=CARTESIAN_POINT('Ctrl Pts',(0.167325958609581,-0.433697199821472,
5.4));
#43572=CARTESIAN_POINT('Ctrl Pts',(0.167325958609581,-0.433697199821472,
5.37));
#43573=CARTESIAN_POINT('',(0.166950926184654,-0.45133022069931,5.4));
#43574=CARTESIAN_POINT('Ctrl Pts',(0.166950926184654,-0.45133022069931,
5.4));
#43575=CARTESIAN_POINT('Ctrl Pts',(0.167325958609581,-0.43744889497757,
5.4));
#43576=CARTESIAN_POINT('Ctrl Pts',(0.167325958609581,-0.433697199821472,
5.4));
#43577=CARTESIAN_POINT('',(0.166950926184654,-0.45133022069931,5.37));
#43578=CARTESIAN_POINT('',(0.166950926184654,-0.45133022069931,5.4));
#43579=CARTESIAN_POINT('Ctrl Pts',(0.166950926184654,-0.45133022069931,
5.37));
#43580=CARTESIAN_POINT('Ctrl Pts',(0.167325958609581,-0.43744889497757,
5.37));
#43581=CARTESIAN_POINT('Ctrl Pts',(0.167325958609581,-0.433697199821472,
5.37));
#43582=CARTESIAN_POINT('Ctrl Pts',(0.0465211719274521,-0.474590814113617,
5.4));
#43583=CARTESIAN_POINT('Ctrl Pts',(0.0465211719274521,-0.474590814113617,
5.37));
#43584=CARTESIAN_POINT('Ctrl Pts',(0.128308281302452,-0.464836394786835,
5.4));
#43585=CARTESIAN_POINT('Ctrl Pts',(0.128308281302452,-0.464836394786835,
5.37));
#43586=CARTESIAN_POINT('Ctrl Pts',(0.166950926184654,-0.45133022069931,
5.4));
#43587=CARTESIAN_POINT('Ctrl Pts',(0.166950926184654,-0.45133022069931,
5.37));
#43588=CARTESIAN_POINT('',(0.0465211719274521,-0.474590814113617,5.4));
#43589=CARTESIAN_POINT('Ctrl Pts',(0.0465211719274521,-0.474590814113617,
5.4));
#43590=CARTESIAN_POINT('Ctrl Pts',(0.128308281302452,-0.464836394786835,
5.4));
#43591=CARTESIAN_POINT('Ctrl Pts',(0.166950926184654,-0.45133022069931,
5.4));
#43592=CARTESIAN_POINT('',(0.0465211719274521,-0.474590814113617,5.37));
#43593=CARTESIAN_POINT('',(0.0465211719274521,-0.474590814113617,5.4));
#43594=CARTESIAN_POINT('Ctrl Pts',(0.0465211719274521,-0.474590814113617,
5.37));
#43595=CARTESIAN_POINT('Ctrl Pts',(0.128308281302452,-0.464836394786835,
5.37));
#43596=CARTESIAN_POINT('Ctrl Pts',(0.166950926184654,-0.45133022069931,
5.37));
#43597=CARTESIAN_POINT('Ctrl Pts',(-0.0135061889886856,-0.484720385074615,
5.4));
#43598=CARTESIAN_POINT('Ctrl Pts',(-0.0135061889886856,-0.484720385074615,
5.37));
#43599=CARTESIAN_POINT('Ctrl Pts',(0.0063779205083847,-0.479468023777008,
5.4));
#43600=CARTESIAN_POINT('Ctrl Pts',(0.0063779205083847,-0.479468023777008,
5.37));
#43601=CARTESIAN_POINT('Ctrl Pts',(0.0465211719274521,-0.474590814113617,
5.4));
#43602=CARTESIAN_POINT('Ctrl Pts',(0.0465211719274521,-0.474590814113617,
5.37));
#43603=CARTESIAN_POINT('',(-0.0135061889886856,-0.484720385074615,5.4));
#43604=CARTESIAN_POINT('Ctrl Pts',(-0.0135061889886856,-0.484720385074615,
5.4));
#43605=CARTESIAN_POINT('Ctrl Pts',(0.0063779205083847,-0.479468023777008,
5.4));
#43606=CARTESIAN_POINT('Ctrl Pts',(0.0465211719274521,-0.474590814113617,
5.4));
#43607=CARTESIAN_POINT('',(-0.0135061889886856,-0.484720385074615,5.37));
#43608=CARTESIAN_POINT('',(-0.0135061889886856,-0.484720385074615,5.4));
#43609=CARTESIAN_POINT('Ctrl Pts',(-0.0135061889886856,-0.484720385074615,
5.37));
#43610=CARTESIAN_POINT('Ctrl Pts',(0.0063779205083847,-0.479468023777008,
5.37));
#43611=CARTESIAN_POINT('Ctrl Pts',(0.0465211719274521,-0.474590814113617,
5.37));
#43612=CARTESIAN_POINT('Ctrl Pts',(-0.0620906502008438,-0.506855404376984,
5.4));
#43613=CARTESIAN_POINT('Ctrl Pts',(-0.0620906502008438,-0.506855404376984,
5.37));
#43614=CARTESIAN_POINT('Ctrl Pts',(-0.0405182987451553,-0.49222377538681,
5.4));
#43615=CARTESIAN_POINT('Ctrl Pts',(-0.0405182987451553,-0.49222377538681,
5.37));
#43616=CARTESIAN_POINT('Ctrl Pts',(-0.0135061889886856,-0.484720385074615,
5.4));
#43617=CARTESIAN_POINT('Ctrl Pts',(-0.0135061889886856,-0.484720385074615,
5.37));
#43618=CARTESIAN_POINT('',(-0.0620906502008438,-0.506855404376984,5.4));
#43619=CARTESIAN_POINT('Ctrl Pts',(-0.0620906502008438,-0.506855404376984,
5.4));
#43620=CARTESIAN_POINT('Ctrl Pts',(-0.0405182987451553,-0.49222377538681,
5.4));
#43621=CARTESIAN_POINT('Ctrl Pts',(-0.0135061889886856,-0.484720385074615,
5.4));
#43622=CARTESIAN_POINT('',(-0.0620906502008438,-0.506855404376984,5.37));
#43623=CARTESIAN_POINT('',(-0.0620906502008438,-0.506855404376984,5.4));
#43624=CARTESIAN_POINT('Ctrl Pts',(-0.0620906502008438,-0.506855404376984,
5.37));
#43625=CARTESIAN_POINT('Ctrl Pts',(-0.0405182987451553,-0.49222377538681,
5.37));
#43626=CARTESIAN_POINT('Ctrl Pts',(-0.0135061889886856,-0.484720385074615,
5.37));
#43627=CARTESIAN_POINT('Ctrl Pts',(-0.0969815403223038,-0.545685684680939,
5.4));
#43628=CARTESIAN_POINT('Ctrl Pts',(-0.0969815403223038,-0.545685684680939,
5.37));
#43629=CARTESIAN_POINT('Ctrl Pts',(-0.0836630016565323,-0.521487152576447,
5.4));
#43630=CARTESIAN_POINT('Ctrl Pts',(-0.0836630016565323,-0.521487152576447,
5.37));
#43631=CARTESIAN_POINT('Ctrl Pts',(-0.0620906502008438,-0.506855404376984,
5.4));
#43632=CARTESIAN_POINT('Ctrl Pts',(-0.0620906502008438,-0.506855404376984,
5.37));
#43633=CARTESIAN_POINT('',(-0.0969815403223038,-0.545685684680939,5.4));
#43634=CARTESIAN_POINT('Ctrl Pts',(-0.0969815403223038,-0.545685684680939,
5.4));
#43635=CARTESIAN_POINT('Ctrl Pts',(-0.0836630016565323,-0.521487152576447,
5.4));
#43636=CARTESIAN_POINT('Ctrl Pts',(-0.0620906502008438,-0.506855404376984,
5.4));
#43637=CARTESIAN_POINT('',(-0.0969815403223038,-0.545685684680939,5.37));
#43638=CARTESIAN_POINT('',(-0.0969815403223038,-0.545685684680939,5.4));
#43639=CARTESIAN_POINT('Ctrl Pts',(-0.0969815403223038,-0.545685684680939,
5.37));
#43640=CARTESIAN_POINT('Ctrl Pts',(-0.0836630016565323,-0.521487152576447,
5.37));
#43641=CARTESIAN_POINT('Ctrl Pts',(-0.0620906502008438,-0.506855404376984,
5.37));
#43642=CARTESIAN_POINT('Ctrl Pts',(-0.110300078988075,-0.599147474765778,
5.4));
#43643=CARTESIAN_POINT('Ctrl Pts',(-0.110300078988075,-0.599147474765778,
5.37));
#43644=CARTESIAN_POINT('Ctrl Pts',(-0.110300078988075,-0.569884097576141,
5.4));
#43645=CARTESIAN_POINT('Ctrl Pts',(-0.110300078988075,-0.569884097576141,
5.37));
#43646=CARTESIAN_POINT('Ctrl Pts',(-0.0969815403223038,-0.545685684680939,
5.4));
#43647=CARTESIAN_POINT('Ctrl Pts',(-0.0969815403223038,-0.545685684680939,
5.37));
#43648=CARTESIAN_POINT('',(-0.110300078988075,-0.599147474765778,5.4));
#43649=CARTESIAN_POINT('Ctrl Pts',(-0.110300078988075,-0.599147474765778,
5.4));
#43650=CARTESIAN_POINT('Ctrl Pts',(-0.110300078988075,-0.569884097576141,
5.4));
#43651=CARTESIAN_POINT('Ctrl Pts',(-0.0969815403223038,-0.545685684680939,
5.4));
#43652=CARTESIAN_POINT('',(-0.110300078988075,-0.599147474765778,5.37));
#43653=CARTESIAN_POINT('',(-0.110300078988075,-0.599147474765778,5.4));
#43654=CARTESIAN_POINT('Ctrl Pts',(-0.110300078988075,-0.599147474765778,
5.37));
#43655=CARTESIAN_POINT('Ctrl Pts',(-0.110300078988075,-0.569884097576141,
5.37));
#43656=CARTESIAN_POINT('Ctrl Pts',(-0.0969815403223038,-0.545685684680939,
5.37));
#43657=CARTESIAN_POINT('Ctrl Pts',(-0.0750341564416885,-0.68112221956253,
5.4));
#43658=CARTESIAN_POINT('Ctrl Pts',(-0.0750341564416885,-0.68112221956253,
5.37));
#43659=CARTESIAN_POINT('Ctrl Pts',(-0.110300078988075,-0.649045145511627,
5.4));
#43660=CARTESIAN_POINT('Ctrl Pts',(-0.110300078988075,-0.649045145511627,
5.37));
#43661=CARTESIAN_POINT('Ctrl Pts',(-0.110300078988075,-0.599147474765778,
5.4));
#43662=CARTESIAN_POINT('Ctrl Pts',(-0.110300078988075,-0.599147474765778,
5.37));
#43663=CARTESIAN_POINT('',(-0.0750341564416885,-0.68112221956253,5.4));
#43664=CARTESIAN_POINT('Ctrl Pts',(-0.0750341564416885,-0.68112221956253,
5.4));
#43665=CARTESIAN_POINT('Ctrl Pts',(-0.110300078988075,-0.649045145511627,
5.4));
#43666=CARTESIAN_POINT('Ctrl Pts',(-0.110300078988075,-0.599147474765778,
5.4));
#43667=CARTESIAN_POINT('',(-0.0750341564416885,-0.68112221956253,5.37));
#43668=CARTESIAN_POINT('',(-0.0750341564416885,-0.68112221956253,5.4));
#43669=CARTESIAN_POINT('Ctrl Pts',(-0.0750341564416885,-0.68112221956253,
5.37));
#43670=CARTESIAN_POINT('Ctrl Pts',(-0.110300078988075,-0.649045145511627,
5.37));
#43671=CARTESIAN_POINT('Ctrl Pts',(-0.110300078988075,-0.599147474765778,
5.37));
#43672=CARTESIAN_POINT('Ctrl Pts',(0.0258867591619492,-0.713199293613434,
5.4));
#43673=CARTESIAN_POINT('Ctrl Pts',(0.0258867591619492,-0.713199293613434,
5.37));
#43674=CARTESIAN_POINT('Ctrl Pts',(-0.0397679954767227,-0.713199293613434,
5.4));
#43675=CARTESIAN_POINT('Ctrl Pts',(-0.0397679954767227,-0.713199293613434,
5.37));
#43676=CARTESIAN_POINT('Ctrl Pts',(-0.0750341564416885,-0.68112221956253,
5.4));
#43677=CARTESIAN_POINT('Ctrl Pts',(-0.0750341564416885,-0.68112221956253,
5.37));
#43678=CARTESIAN_POINT('',(0.0258867591619492,-0.713199293613434,5.4));
#43679=CARTESIAN_POINT('Ctrl Pts',(0.0258867591619492,-0.713199293613434,
5.4));
#43680=CARTESIAN_POINT('Ctrl Pts',(-0.0397679954767227,-0.713199293613434,
5.4));
#43681=CARTESIAN_POINT('Ctrl Pts',(-0.0750341564416885,-0.68112221956253,
5.4));
#43682=CARTESIAN_POINT('',(0.0258867591619492,-0.713199293613434,5.37));
#43683=CARTESIAN_POINT('',(0.0258867591619492,-0.713199293613434,5.4));
#43684=CARTESIAN_POINT('Ctrl Pts',(0.0258867591619492,-0.713199293613434,
5.37));
#43685=CARTESIAN_POINT('Ctrl Pts',(-0.0397679954767227,-0.713199293613434,
5.37));
#43686=CARTESIAN_POINT('Ctrl Pts',(-0.0750341564416885,-0.68112221956253,
5.37));
#43687=CARTESIAN_POINT('Ctrl Pts',(0.100357994437218,-0.700068271160126,
5.4));
#43688=CARTESIAN_POINT('Ctrl Pts',(0.100357994437218,-0.700068271160126,
5.37));
#43689=CARTESIAN_POINT('Ctrl Pts',(0.0656547397375107,-0.713199293613434,
5.4));
#43690=CARTESIAN_POINT('Ctrl Pts',(0.0656547397375107,-0.713199293613434,
5.37));
#43691=CARTESIAN_POINT('Ctrl Pts',(0.0258867591619492,-0.713199293613434,
5.4));
#43692=CARTESIAN_POINT('Ctrl Pts',(0.0258867591619492,-0.713199293613434,
5.37));
#43693=CARTESIAN_POINT('',(0.100357994437218,-0.700068271160126,5.4));
#43694=CARTESIAN_POINT('Ctrl Pts',(0.100357994437218,-0.700068271160126,
5.4));
#43695=CARTESIAN_POINT('Ctrl Pts',(0.0656547397375107,-0.713199293613434,
5.4));
#43696=CARTESIAN_POINT('Ctrl Pts',(0.0258867591619492,-0.713199293613434,
5.4));
#43697=CARTESIAN_POINT('',(0.100357994437218,-0.700068271160126,5.37));
#43698=CARTESIAN_POINT('',(0.100357994437218,-0.700068271160126,5.4));
#43699=CARTESIAN_POINT('Ctrl Pts',(0.100357994437218,-0.700068271160126,
5.37));
#43700=CARTESIAN_POINT('Ctrl Pts',(0.0656547397375107,-0.713199293613434,
5.37));
#43701=CARTESIAN_POINT('Ctrl Pts',(0.0258867591619492,-0.713199293613434,
5.37));
#43702=CARTESIAN_POINT('Ctrl Pts',(0.172578319907188,-0.655047810077667,
5.4));
#43703=CARTESIAN_POINT('Ctrl Pts',(0.172578319907188,-0.655047810077667,
5.37));
#43704=CARTESIAN_POINT('Ctrl Pts',(0.135061249136925,-0.686937367916107,
5.4));
#43705=CARTESIAN_POINT('Ctrl Pts',(0.135061249136925,-0.686937367916107,
5.37));
#43706=CARTESIAN_POINT('Ctrl Pts',(0.100357994437218,-0.700068271160126,
5.4));
#43707=CARTESIAN_POINT('Ctrl Pts',(0.100357994437218,-0.700068271160126,
5.37));
#43708=CARTESIAN_POINT('',(0.172578319907188,-0.655047810077667,5.4));
#43709=CARTESIAN_POINT('Ctrl Pts',(0.172578319907188,-0.655047810077667,
5.4));
#43710=CARTESIAN_POINT('Ctrl Pts',(0.135061249136925,-0.686937367916107,
5.4));
#43711=CARTESIAN_POINT('Ctrl Pts',(0.100357994437218,-0.700068271160126,
5.4));
#43712=CARTESIAN_POINT('',(0.172578319907188,-0.655047810077667,5.37));
#43713=CARTESIAN_POINT('',(0.172578319907188,-0.655047810077667,5.4));
#43714=CARTESIAN_POINT('Ctrl Pts',(0.172578319907188,-0.655047810077667,
5.37));
#43715=CARTESIAN_POINT('Ctrl Pts',(0.135061249136925,-0.686937367916107,
5.37));
#43716=CARTESIAN_POINT('Ctrl Pts',(0.100357994437218,-0.700068271160126,
5.37));
#43717=CARTESIAN_POINT('Ctrl Pts',(0.186084732413292,-0.704195177555084,
5.4));
#43718=CARTESIAN_POINT('Ctrl Pts',(0.186084732413292,-0.704195177555084,
5.37));
#43719=CARTESIAN_POINT('Ctrl Pts',(0.175579771399498,-0.683185613155365,
5.4));
#43720=CARTESIAN_POINT('Ctrl Pts',(0.175579771399498,-0.683185613155365,
5.37));
#43721=CARTESIAN_POINT('Ctrl Pts',(0.172578319907188,-0.655047810077667,
5.4));
#43722=CARTESIAN_POINT('Ctrl Pts',(0.172578319907188,-0.655047810077667,
5.37));
#43723=CARTESIAN_POINT('',(0.186084732413292,-0.704195177555084,5.4));
#43724=CARTESIAN_POINT('Ctrl Pts',(0.186084732413292,-0.704195177555084,
5.4));
#43725=CARTESIAN_POINT('Ctrl Pts',(0.175579771399498,-0.683185613155365,
5.4));
#43726=CARTESIAN_POINT('Ctrl Pts',(0.172578319907188,-0.655047810077667,
5.4));
#43727=CARTESIAN_POINT('',(0.186084732413292,-0.704195177555084,5.37));
#43728=CARTESIAN_POINT('',(0.186084732413292,-0.704195177555084,5.4));
#43729=CARTESIAN_POINT('Ctrl Pts',(0.186084732413292,-0.704195177555084,
5.37));
#43730=CARTESIAN_POINT('Ctrl Pts',(0.175579771399498,-0.683185613155365,
5.37));
#43731=CARTESIAN_POINT('Ctrl Pts',(0.172578319907188,-0.655047810077667,
5.37));
#43732=CARTESIAN_POINT('Origin',(0.256616577506065,-0.704195177555084,5.4));
#43733=CARTESIAN_POINT('',(0.128308288753032,-0.704195177555084,5.4));
#43734=CARTESIAN_POINT('',(0.256616577506065,-0.704195177555084,5.37));
#43735=CARTESIAN_POINT('Origin',(0.0731582492589951,-0.50497961640358,5.37));
#43736=CARTESIAN_POINT('Ctrl Pts',(2.58492515981197,0.650545740127563,5.4));
#43737=CARTESIAN_POINT('Ctrl Pts',(2.58492515981197,0.650545740127563,5.37));
#43738=CARTESIAN_POINT('Ctrl Pts',(2.53840397298336,0.650545740127563,5.4));
#43739=CARTESIAN_POINT('Ctrl Pts',(2.53840397298336,0.650545740127563,5.37));
#43740=CARTESIAN_POINT('Ctrl Pts',(2.51064155995846,0.611152821779251,5.4));
#43741=CARTESIAN_POINT('Ctrl Pts',(2.51064155995846,0.611152821779251,5.37));
#43742=CARTESIAN_POINT('',(2.58492515981197,0.650545740127563,5.4));
#43743=CARTESIAN_POINT('',(2.51064155995846,0.611152821779251,5.4));
#43744=CARTESIAN_POINT('Ctrl Pts',(2.58492515981197,0.650545740127563,5.4));
#43745=CARTESIAN_POINT('Ctrl Pts',(2.53840397298336,0.650545740127563,5.4));
#43746=CARTESIAN_POINT('Ctrl Pts',(2.51064155995846,0.611152821779251,5.4));
#43747=CARTESIAN_POINT('',(2.58492515981197,0.650545740127563,5.37));
#43748=CARTESIAN_POINT('',(2.58492515981197,0.650545740127563,5.4));
#43749=CARTESIAN_POINT('',(2.51064155995846,0.611152821779251,5.37));
#43750=CARTESIAN_POINT('Ctrl Pts',(2.58492515981197,0.650545740127563,5.37));
#43751=CARTESIAN_POINT('Ctrl Pts',(2.53840397298336,0.650545740127563,5.37));
#43752=CARTESIAN_POINT('Ctrl Pts',(2.51064155995846,0.611152821779251,5.37));
#43753=CARTESIAN_POINT('',(2.51064155995846,0.611152821779251,5.4));
#43754=CARTESIAN_POINT('Ctrl Pts',(2.66389845311642,0.605900430679321,5.4));
#43755=CARTESIAN_POINT('Ctrl Pts',(2.66389845311642,0.605900430679321,5.37));
#43756=CARTESIAN_POINT('Ctrl Pts',(2.63219641149044,0.650545740127563,5.4));
#43757=CARTESIAN_POINT('Ctrl Pts',(2.63219641149044,0.650545740127563,5.37));
#43758=CARTESIAN_POINT('Ctrl Pts',(2.58492515981197,0.650545740127563,5.4));
#43759=CARTESIAN_POINT('Ctrl Pts',(2.58492515981197,0.650545740127563,5.37));
#43760=CARTESIAN_POINT('',(2.66389845311642,0.605900430679321,5.4));
#43761=CARTESIAN_POINT('Ctrl Pts',(2.66389845311642,0.605900430679321,5.4));
#43762=CARTESIAN_POINT('Ctrl Pts',(2.63219641149044,0.650545740127563,5.4));
#43763=CARTESIAN_POINT('Ctrl Pts',(2.58492515981197,0.650545740127563,5.4));
#43764=CARTESIAN_POINT('',(2.66389845311642,0.605900430679321,5.37));
#43765=CARTESIAN_POINT('',(2.66389845311642,0.605900430679321,5.4));
#43766=CARTESIAN_POINT('Ctrl Pts',(2.66389845311642,0.605900430679321,5.37));
#43767=CARTESIAN_POINT('Ctrl Pts',(2.63219641149044,0.650545740127563,5.37));
#43768=CARTESIAN_POINT('Ctrl Pts',(2.58492515981197,0.650545740127563,5.37));
#43769=CARTESIAN_POINT('Ctrl Pts',(2.69560049474239,0.425443404912949,5.4));
#43770=CARTESIAN_POINT('Ctrl Pts',(2.69560049474239,0.425443404912949,5.37));
#43771=CARTESIAN_POINT('Ctrl Pts',(2.69560049474239,0.561255151033402,5.4));
#43772=CARTESIAN_POINT('Ctrl Pts',(2.69560049474239,0.561255151033402,5.37));
#43773=CARTESIAN_POINT('Ctrl Pts',(2.66389845311642,0.605900430679321,5.4));
#43774=CARTESIAN_POINT('Ctrl Pts',(2.66389845311642,0.605900430679321,5.37));
#43775=CARTESIAN_POINT('',(2.69560049474239,0.425443404912949,5.4));
#43776=CARTESIAN_POINT('Ctrl Pts',(2.69560049474239,0.425443404912949,5.4));
#43777=CARTESIAN_POINT('Ctrl Pts',(2.69560049474239,0.561255151033402,5.4));
#43778=CARTESIAN_POINT('Ctrl Pts',(2.66389845311642,0.605900430679321,5.4));
#43779=CARTESIAN_POINT('',(2.69560049474239,0.425443404912949,5.37));
#43780=CARTESIAN_POINT('',(2.69560049474239,0.425443404912949,5.4));
#43781=CARTESIAN_POINT('Ctrl Pts',(2.69560049474239,0.425443404912949,5.37));
#43782=CARTESIAN_POINT('Ctrl Pts',(2.69560049474239,0.561255151033402,5.37));
#43783=CARTESIAN_POINT('Ctrl Pts',(2.66389845311642,0.605900430679321,5.37));
#43784=CARTESIAN_POINT('Ctrl Pts',(2.66389845311642,0.245361530780792,5.4));
#43785=CARTESIAN_POINT('Ctrl Pts',(2.66389845311642,0.245361530780792,5.37));
#43786=CARTESIAN_POINT('Ctrl Pts',(2.69560049474239,0.290381991863251,5.4));
#43787=CARTESIAN_POINT('Ctrl Pts',(2.69560049474239,0.290381991863251,5.37));
#43788=CARTESIAN_POINT('Ctrl Pts',(2.69560049474239,0.425443404912949,5.4));
#43789=CARTESIAN_POINT('Ctrl Pts',(2.69560049474239,0.425443404912949,5.37));
#43790=CARTESIAN_POINT('',(2.66389845311642,0.245361530780792,5.4));
#43791=CARTESIAN_POINT('Ctrl Pts',(2.66389845311642,0.245361530780792,5.4));
#43792=CARTESIAN_POINT('Ctrl Pts',(2.69560049474239,0.290381991863251,5.4));
#43793=CARTESIAN_POINT('Ctrl Pts',(2.69560049474239,0.425443404912949,5.4));
#43794=CARTESIAN_POINT('',(2.66389845311642,0.245361530780792,5.37));
#43795=CARTESIAN_POINT('',(2.66389845311642,0.245361530780792,5.4));
#43796=CARTESIAN_POINT('Ctrl Pts',(2.66389845311642,0.245361530780792,5.37));
#43797=CARTESIAN_POINT('Ctrl Pts',(2.69560049474239,0.290381991863251,5.37));
#43798=CARTESIAN_POINT('Ctrl Pts',(2.69560049474239,0.425443404912949,5.37));
#43799=CARTESIAN_POINT('Ctrl Pts',(2.58567522466183,0.200341069698334,5.4));
#43800=CARTESIAN_POINT('Ctrl Pts',(2.58567522466183,0.200341069698334,5.37));
#43801=CARTESIAN_POINT('Ctrl Pts',(2.63219641149044,0.200341069698334,5.4));
#43802=CARTESIAN_POINT('Ctrl Pts',(2.63219641149044,0.200341069698334,5.37));
#43803=CARTESIAN_POINT('Ctrl Pts',(2.66389845311642,0.245361530780792,5.4));
#43804=CARTESIAN_POINT('Ctrl Pts',(2.66389845311642,0.245361530780792,5.37));
#43805=CARTESIAN_POINT('',(2.58567522466183,0.200341069698334,5.4));
#43806=CARTESIAN_POINT('Ctrl Pts',(2.58567522466183,0.200341069698334,5.4));
#43807=CARTESIAN_POINT('Ctrl Pts',(2.63219641149044,0.200341069698334,5.4));
#43808=CARTESIAN_POINT('Ctrl Pts',(2.66389845311642,0.245361530780792,5.4));
#43809=CARTESIAN_POINT('',(2.58567522466183,0.200341069698334,5.37));
#43810=CARTESIAN_POINT('',(2.58567522466183,0.200341069698334,5.4));
#43811=CARTESIAN_POINT('Ctrl Pts',(2.58567522466183,0.200341069698334,5.37));
#43812=CARTESIAN_POINT('Ctrl Pts',(2.63219641149044,0.200341069698334,5.37));
#43813=CARTESIAN_POINT('Ctrl Pts',(2.66389845311642,0.245361530780792,5.37));
#43814=CARTESIAN_POINT('Ctrl Pts',(2.5074524730444,0.245173954963684,5.4));
#43815=CARTESIAN_POINT('Ctrl Pts',(2.5074524730444,0.245173954963684,5.37));
#43816=CARTESIAN_POINT('Ctrl Pts',(2.53915451467037,0.200341069698334,5.4));
#43817=CARTESIAN_POINT('Ctrl Pts',(2.53915451467037,0.200341069698334,5.37));
#43818=CARTESIAN_POINT('Ctrl Pts',(2.58567522466183,0.200341069698334,5.4));
#43819=CARTESIAN_POINT('Ctrl Pts',(2.58567522466183,0.200341069698334,5.37));
#43820=CARTESIAN_POINT('',(2.5074524730444,0.245173954963684,5.4));
#43821=CARTESIAN_POINT('Ctrl Pts',(2.5074524730444,0.245173954963684,5.4));
#43822=CARTESIAN_POINT('Ctrl Pts',(2.53915451467037,0.200341069698334,5.4));
#43823=CARTESIAN_POINT('Ctrl Pts',(2.58567522466183,0.200341069698334,5.4));
#43824=CARTESIAN_POINT('',(2.5074524730444,0.245173954963684,5.37));
#43825=CARTESIAN_POINT('',(2.5074524730444,0.245173954963684,5.4));
#43826=CARTESIAN_POINT('Ctrl Pts',(2.5074524730444,0.245173954963684,5.37));
#43827=CARTESIAN_POINT('Ctrl Pts',(2.53915451467037,0.200341069698334,5.37));
#43828=CARTESIAN_POINT('Ctrl Pts',(2.58567522466183,0.200341069698334,5.37));
#43829=CARTESIAN_POINT('Ctrl Pts',(2.47575043141842,0.425443404912949,5.4));
#43830=CARTESIAN_POINT('Ctrl Pts',(2.47575043141842,0.425443404912949,5.37));
#43831=CARTESIAN_POINT('Ctrl Pts',(2.47575043141842,0.290006840229034,5.4));
#43832=CARTESIAN_POINT('Ctrl Pts',(2.47575043141842,0.290006840229034,5.37));
#43833=CARTESIAN_POINT('Ctrl Pts',(2.5074524730444,0.245173954963684,5.4));
#43834=CARTESIAN_POINT('Ctrl Pts',(2.5074524730444,0.245173954963684,5.37));
#43835=CARTESIAN_POINT('',(2.47575043141842,0.425443404912949,5.4));
#43836=CARTESIAN_POINT('Ctrl Pts',(2.47575043141842,0.425443404912949,5.4));
#43837=CARTESIAN_POINT('Ctrl Pts',(2.47575043141842,0.290006840229034,5.4));
#43838=CARTESIAN_POINT('Ctrl Pts',(2.5074524730444,0.245173954963684,5.4));
#43839=CARTESIAN_POINT('',(2.47575043141842,0.425443404912949,5.37));
#43840=CARTESIAN_POINT('',(2.47575043141842,0.425443404912949,5.4));
#43841=CARTESIAN_POINT('Ctrl Pts',(2.47575043141842,0.425443404912949,5.37));
#43842=CARTESIAN_POINT('Ctrl Pts',(2.47575043141842,0.290006840229034,5.37));
#43843=CARTESIAN_POINT('Ctrl Pts',(2.5074524730444,0.245173954963684,5.37));
#43844=CARTESIAN_POINT('Ctrl Pts',(2.51064155995846,0.611152821779251,5.4));
#43845=CARTESIAN_POINT('Ctrl Pts',(2.51064155995846,0.611152821779251,5.37));
#43846=CARTESIAN_POINT('Ctrl Pts',(2.47575043141842,0.560879969596863,5.4));
#43847=CARTESIAN_POINT('Ctrl Pts',(2.47575043141842,0.560879969596863,5.37));
#43848=CARTESIAN_POINT('Ctrl Pts',(2.47575043141842,0.425443404912949,5.4));
#43849=CARTESIAN_POINT('Ctrl Pts',(2.47575043141842,0.425443404912949,5.37));
#43850=CARTESIAN_POINT('Ctrl Pts',(2.51064155995846,0.611152821779251,5.4));
#43851=CARTESIAN_POINT('Ctrl Pts',(2.47575043141842,0.560879969596863,5.4));
#43852=CARTESIAN_POINT('Ctrl Pts',(2.47575043141842,0.425443404912949,5.4));
#43853=CARTESIAN_POINT('Ctrl Pts',(2.51064155995846,0.611152821779251,5.37));
#43854=CARTESIAN_POINT('Ctrl Pts',(2.47575043141842,0.560879969596863,5.37));
#43855=CARTESIAN_POINT('Ctrl Pts',(2.47575043141842,0.425443404912949,5.37));
#43856=CARTESIAN_POINT('Ctrl Pts',(2.68565843999386,0.177268081903458,5.4));
#43857=CARTESIAN_POINT('Ctrl Pts',(2.68565843999386,0.177268081903458,5.37));
#43858=CARTESIAN_POINT('Ctrl Pts',(2.64607809484005,0.144815826416016,5.4));
#43859=CARTESIAN_POINT('Ctrl Pts',(2.64607809484005,0.144815826416016,5.37));
#43860=CARTESIAN_POINT('Ctrl Pts',(2.58567522466183,0.144815826416016,5.4));
#43861=CARTESIAN_POINT('Ctrl Pts',(2.58567522466183,0.144815826416016,5.37));
#43862=CARTESIAN_POINT('',(2.68565843999386,0.177268081903458,5.4));
#43863=CARTESIAN_POINT('',(2.58567522466183,0.144815826416016,5.4));
#43864=CARTESIAN_POINT('Ctrl Pts',(2.68565843999386,0.177268081903458,5.4));
#43865=CARTESIAN_POINT('Ctrl Pts',(2.64607809484005,0.144815826416016,5.4));
#43866=CARTESIAN_POINT('Ctrl Pts',(2.58567522466183,0.144815826416016,5.4));
#43867=CARTESIAN_POINT('',(2.68565843999386,0.177268081903458,5.37));
#43868=CARTESIAN_POINT('',(2.68565843999386,0.177268081903458,5.4));
#43869=CARTESIAN_POINT('',(2.58567522466183,0.144815826416016,5.37));
#43870=CARTESIAN_POINT('Ctrl Pts',(2.68565843999386,0.177268081903458,5.37));
#43871=CARTESIAN_POINT('Ctrl Pts',(2.64607809484005,0.144815826416016,5.37));
#43872=CARTESIAN_POINT('Ctrl Pts',(2.58567522466183,0.144815826416016,5.37));
#43873=CARTESIAN_POINT('',(2.58567522466183,0.144815826416016,5.4));
#43874=CARTESIAN_POINT('Ctrl Pts',(2.74512289464474,0.269184851646423,5.4));
#43875=CARTESIAN_POINT('Ctrl Pts',(2.74512289464474,0.269184851646423,5.37));
#43876=CARTESIAN_POINT('Ctrl Pts',(2.72523878514767,0.2097203373909,5.4));
#43877=CARTESIAN_POINT('Ctrl Pts',(2.72523878514767,0.2097203373909,5.37));
#43878=CARTESIAN_POINT('Ctrl Pts',(2.68565843999386,0.177268081903458,5.4));
#43879=CARTESIAN_POINT('Ctrl Pts',(2.68565843999386,0.177268081903458,5.37));
#43880=CARTESIAN_POINT('',(2.74512289464474,0.269184851646423,5.4));
#43881=CARTESIAN_POINT('Ctrl Pts',(2.74512289464474,0.269184851646423,5.4));
#43882=CARTESIAN_POINT('Ctrl Pts',(2.72523878514767,0.2097203373909,5.4));
#43883=CARTESIAN_POINT('Ctrl Pts',(2.68565843999386,0.177268081903458,5.4));
#43884=CARTESIAN_POINT('',(2.74512289464474,0.269184851646423,5.37));
#43885=CARTESIAN_POINT('',(2.74512289464474,0.269184851646423,5.4));
#43886=CARTESIAN_POINT('Ctrl Pts',(2.74512289464474,0.269184851646423,5.37));
#43887=CARTESIAN_POINT('Ctrl Pts',(2.72523878514767,0.2097203373909,5.37));
#43888=CARTESIAN_POINT('Ctrl Pts',(2.68565843999386,0.177268081903458,5.37));
#43889=CARTESIAN_POINT('Ctrl Pts',(2.76500700414181,0.425443404912949,5.4));
#43890=CARTESIAN_POINT('Ctrl Pts',(2.76500700414181,0.425443404912949,5.37));
#43891=CARTESIAN_POINT('Ctrl Pts',(2.76500700414181,0.328649395704269,5.4));
#43892=CARTESIAN_POINT('Ctrl Pts',(2.76500700414181,0.328649395704269,5.37));
#43893=CARTESIAN_POINT('Ctrl Pts',(2.74512289464474,0.269184851646423,5.4));
#43894=CARTESIAN_POINT('Ctrl Pts',(2.74512289464474,0.269184851646423,5.37));
#43895=CARTESIAN_POINT('',(2.76500700414181,0.425443404912949,5.4));
#43896=CARTESIAN_POINT('Ctrl Pts',(2.76500700414181,0.425443404912949,5.4));
#43897=CARTESIAN_POINT('Ctrl Pts',(2.76500700414181,0.328649395704269,5.4));
#43898=CARTESIAN_POINT('Ctrl Pts',(2.74512289464474,0.269184851646423,5.4));
#43899=CARTESIAN_POINT('',(2.76500700414181,0.425443404912949,5.37));
#43900=CARTESIAN_POINT('',(2.76500700414181,0.425443404912949,5.4));
#43901=CARTESIAN_POINT('Ctrl Pts',(2.76500700414181,0.425443404912949,5.37));
#43902=CARTESIAN_POINT('Ctrl Pts',(2.76500700414181,0.328649395704269,5.37));
#43903=CARTESIAN_POINT('Ctrl Pts',(2.74512289464474,0.269184851646423,5.37));
#43904=CARTESIAN_POINT('Ctrl Pts',(2.75262640416622,0.555440002679825,5.4));
#43905=CARTESIAN_POINT('Ctrl Pts',(2.75262640416622,0.555440002679825,5.37));
#43906=CARTESIAN_POINT('Ctrl Pts',(2.76500700414181,0.507230573892593,5.4));
#43907=CARTESIAN_POINT('Ctrl Pts',(2.76500700414181,0.507230573892593,5.37));
#43908=CARTESIAN_POINT('Ctrl Pts',(2.76500700414181,0.425443404912949,5.4));
#43909=CARTESIAN_POINT('Ctrl Pts',(2.76500700414181,0.425443404912949,5.37));
#43910=CARTESIAN_POINT('',(2.75262640416622,0.555440002679825,5.4));
#43911=CARTESIAN_POINT('Ctrl Pts',(2.75262640416622,0.555440002679825,5.4));
#43912=CARTESIAN_POINT('Ctrl Pts',(2.76500700414181,0.507230573892593,5.4));
#43913=CARTESIAN_POINT('Ctrl Pts',(2.76500700414181,0.425443404912949,5.4));
#43914=CARTESIAN_POINT('',(2.75262640416622,0.555440002679825,5.37));
#43915=CARTESIAN_POINT('',(2.75262640416622,0.555440002679825,5.4));
#43916=CARTESIAN_POINT('Ctrl Pts',(2.75262640416622,0.555440002679825,5.37));
#43917=CARTESIAN_POINT('Ctrl Pts',(2.76500700414181,0.507230573892593,5.37));
#43918=CARTESIAN_POINT('Ctrl Pts',(2.76500700414181,0.425443404912949,5.37));
#43919=CARTESIAN_POINT('Ctrl Pts',(2.71848581731319,0.63722717165947,5.4));
#43920=CARTESIAN_POINT('Ctrl Pts',(2.71848581731319,0.63722717165947,5.37));
#43921=CARTESIAN_POINT('Ctrl Pts',(2.74024580419064,0.603649401664734,5.4));
#43922=CARTESIAN_POINT('Ctrl Pts',(2.74024580419064,0.603649401664734,5.37));
#43923=CARTESIAN_POINT('Ctrl Pts',(2.75262640416622,0.555440002679825,5.4));
#43924=CARTESIAN_POINT('Ctrl Pts',(2.75262640416622,0.555440002679825,5.37));
#43925=CARTESIAN_POINT('',(2.71848581731319,0.63722717165947,5.4));
#43926=CARTESIAN_POINT('Ctrl Pts',(2.71848581731319,0.63722717165947,5.4));
#43927=CARTESIAN_POINT('Ctrl Pts',(2.74024580419064,0.603649401664734,5.4));
#43928=CARTESIAN_POINT('Ctrl Pts',(2.75262640416622,0.555440002679825,5.4));
#43929=CARTESIAN_POINT('',(2.71848581731319,0.63722717165947,5.37));
#43930=CARTESIAN_POINT('',(2.71848581731319,0.63722717165947,5.4));
#43931=CARTESIAN_POINT('Ctrl Pts',(2.71848581731319,0.63722717165947,5.37));
#43932=CARTESIAN_POINT('Ctrl Pts',(2.74024580419064,0.603649401664734,5.37));
#43933=CARTESIAN_POINT('Ctrl Pts',(2.75262640416622,0.555440002679825,5.37));
#43934=CARTESIAN_POINT('Ctrl Pts',(2.66333578526974,0.688625538349152,5.4));
#43935=CARTESIAN_POINT('Ctrl Pts',(2.66333578526974,0.688625538349152,5.37));
#43936=CARTESIAN_POINT('Ctrl Pts',(2.69672583043575,0.670804941654205,5.4));
#43937=CARTESIAN_POINT('Ctrl Pts',(2.69672583043575,0.670804941654205,5.37));
#43938=CARTESIAN_POINT('Ctrl Pts',(2.71848581731319,0.63722717165947,5.4));
#43939=CARTESIAN_POINT('Ctrl Pts',(2.71848581731319,0.63722717165947,5.37));
#43940=CARTESIAN_POINT('',(2.66333578526974,0.688625538349152,5.4));
#43941=CARTESIAN_POINT('Ctrl Pts',(2.66333578526974,0.688625538349152,5.4));
#43942=CARTESIAN_POINT('Ctrl Pts',(2.69672583043575,0.670804941654205,5.4));
#43943=CARTESIAN_POINT('Ctrl Pts',(2.71848581731319,0.63722717165947,5.4));
#43944=CARTESIAN_POINT('',(2.66333578526974,0.688625538349152,5.37));
#43945=CARTESIAN_POINT('',(2.66333578526974,0.688625538349152,5.4));
#43946=CARTESIAN_POINT('Ctrl Pts',(2.66333578526974,0.688625538349152,5.37));
#43947=CARTESIAN_POINT('Ctrl Pts',(2.69672583043575,0.670804941654205,5.37));
#43948=CARTESIAN_POINT('Ctrl Pts',(2.71848581731319,0.63722717165947,5.37));
#43949=CARTESIAN_POINT('Ctrl Pts',(2.58567522466183,0.706446135044098,5.4));
#43950=CARTESIAN_POINT('Ctrl Pts',(2.58567522466183,0.706446135044098,5.37));
#43951=CARTESIAN_POINT('Ctrl Pts',(2.62994574010372,0.706446135044098,5.4));
#43952=CARTESIAN_POINT('Ctrl Pts',(2.62994574010372,0.706446135044098,5.37));
#43953=CARTESIAN_POINT('Ctrl Pts',(2.66333578526974,0.688625538349152,5.4));
#43954=CARTESIAN_POINT('Ctrl Pts',(2.66333578526974,0.688625538349152,5.37));
#43955=CARTESIAN_POINT('',(2.58567522466183,0.706446135044098,5.4));
#43956=CARTESIAN_POINT('Ctrl Pts',(2.58567522466183,0.706446135044098,5.4));
#43957=CARTESIAN_POINT('Ctrl Pts',(2.62994574010372,0.706446135044098,5.4));
#43958=CARTESIAN_POINT('Ctrl Pts',(2.66333578526974,0.688625538349152,5.4));
#43959=CARTESIAN_POINT('',(2.58567522466183,0.706446135044098,5.37));
#43960=CARTESIAN_POINT('',(2.58567522466183,0.706446135044098,5.4));
#43961=CARTESIAN_POINT('Ctrl Pts',(2.58567522466183,0.706446135044098,5.37));
#43962=CARTESIAN_POINT('Ctrl Pts',(2.62994574010372,0.706446135044098,5.37));
#43963=CARTESIAN_POINT('Ctrl Pts',(2.66333578526974,0.688625538349152,5.37));
#43964=CARTESIAN_POINT('Ctrl Pts',(2.48606775701046,0.674181485176086,5.4));
#43965=CARTESIAN_POINT('Ctrl Pts',(2.48606775701046,0.674181485176086,5.37));
#43966=CARTESIAN_POINT('Ctrl Pts',(2.52564810216427,0.706446135044098,5.4));
#43967=CARTESIAN_POINT('Ctrl Pts',(2.52564810216427,0.706446135044098,5.37));
#43968=CARTESIAN_POINT('Ctrl Pts',(2.58567522466183,0.706446135044098,5.4));
#43969=CARTESIAN_POINT('Ctrl Pts',(2.58567522466183,0.706446135044098,5.37));
#43970=CARTESIAN_POINT('',(2.48606775701046,0.674181485176086,5.4));
#43971=CARTESIAN_POINT('Ctrl Pts',(2.48606775701046,0.674181485176086,5.4));
#43972=CARTESIAN_POINT('Ctrl Pts',(2.52564810216427,0.706446135044098,5.4));
#43973=CARTESIAN_POINT('Ctrl Pts',(2.58567522466183,0.706446135044098,5.4));
#43974=CARTESIAN_POINT('',(2.48606775701046,0.674181485176086,5.37));
#43975=CARTESIAN_POINT('',(2.48606775701046,0.674181485176086,5.4));
#43976=CARTESIAN_POINT('Ctrl Pts',(2.48606775701046,0.674181485176086,5.37));
#43977=CARTESIAN_POINT('Ctrl Pts',(2.52564810216427,0.706446135044098,5.37));
#43978=CARTESIAN_POINT('Ctrl Pts',(2.58567522466183,0.706446135044098,5.37));
#43979=CARTESIAN_POINT('Ctrl Pts',(2.42641542851925,0.582452261447907,5.4));
#43980=CARTESIAN_POINT('Ctrl Pts',(2.42641542851925,0.582452261447907,5.37));
#43981=CARTESIAN_POINT('Ctrl Pts',(2.44648693501949,0.641916805505753,5.4));
#43982=CARTESIAN_POINT('Ctrl Pts',(2.44648693501949,0.641916805505753,5.37));
#43983=CARTESIAN_POINT('Ctrl Pts',(2.48606775701046,0.674181485176086,5.4));
#43984=CARTESIAN_POINT('Ctrl Pts',(2.48606775701046,0.674181485176086,5.37));
#43985=CARTESIAN_POINT('',(2.42641542851925,0.582452261447907,5.4));
#43986=CARTESIAN_POINT('Ctrl Pts',(2.42641542851925,0.582452261447907,5.4));
#43987=CARTESIAN_POINT('Ctrl Pts',(2.44648693501949,0.641916805505753,5.4));
#43988=CARTESIAN_POINT('Ctrl Pts',(2.48606775701046,0.674181485176086,5.4));
#43989=CARTESIAN_POINT('',(2.42641542851925,0.582452261447907,5.37));
#43990=CARTESIAN_POINT('',(2.42641542851925,0.582452261447907,5.4));
#43991=CARTESIAN_POINT('Ctrl Pts',(2.42641542851925,0.582452261447907,5.37));
#43992=CARTESIAN_POINT('Ctrl Pts',(2.44648693501949,0.641916805505753,5.37));
#43993=CARTESIAN_POINT('Ctrl Pts',(2.48606775701046,0.674181485176086,5.37));
#43994=CARTESIAN_POINT('Ctrl Pts',(2.406343922019,0.425443404912949,5.4));
#43995=CARTESIAN_POINT('Ctrl Pts',(2.406343922019,0.425443404912949,5.37));
#43996=CARTESIAN_POINT('Ctrl Pts',(2.406343922019,0.522987747192383,5.4));
#43997=CARTESIAN_POINT('Ctrl Pts',(2.406343922019,0.522987747192383,5.37));
#43998=CARTESIAN_POINT('Ctrl Pts',(2.42641542851925,0.582452261447907,5.4));
#43999=CARTESIAN_POINT('Ctrl Pts',(2.42641542851925,0.582452261447907,5.37));
#44000=CARTESIAN_POINT('',(2.406343922019,0.425443404912949,5.4));
#44001=CARTESIAN_POINT('Ctrl Pts',(2.406343922019,0.425443404912949,5.4));
#44002=CARTESIAN_POINT('Ctrl Pts',(2.406343922019,0.522987747192383,5.4));
#44003=CARTESIAN_POINT('Ctrl Pts',(2.42641542851925,0.582452261447907,5.4));
#44004=CARTESIAN_POINT('',(2.406343922019,0.425443404912949,5.37));
#44005=CARTESIAN_POINT('',(2.406343922019,0.425443404912949,5.4));
#44006=CARTESIAN_POINT('Ctrl Pts',(2.406343922019,0.425443404912949,5.37));
#44007=CARTESIAN_POINT('Ctrl Pts',(2.406343922019,0.522987747192383,5.37));
#44008=CARTESIAN_POINT('Ctrl Pts',(2.42641542851925,0.582452261447907,5.37));
#44009=CARTESIAN_POINT('Ctrl Pts',(2.46074388921261,0.201841765642166,5.4));
#44010=CARTESIAN_POINT('Ctrl Pts',(2.46074388921261,0.201841765642166,5.37));
#44011=CARTESIAN_POINT('Ctrl Pts',(2.406343922019,0.270497941970825,5.4));
#44012=CARTESIAN_POINT('Ctrl Pts',(2.406343922019,0.270497941970825,5.37));
#44013=CARTESIAN_POINT('Ctrl Pts',(2.406343922019,0.425443404912949,5.4));
#44014=CARTESIAN_POINT('Ctrl Pts',(2.406343922019,0.425443404912949,5.37));
#44015=CARTESIAN_POINT('',(2.46074388921261,0.201841765642166,5.4));
#44016=CARTESIAN_POINT('Ctrl Pts',(2.46074388921261,0.201841765642166,5.4));
#44017=CARTESIAN_POINT('Ctrl Pts',(2.406343922019,0.270497941970825,5.4));
#44018=CARTESIAN_POINT('Ctrl Pts',(2.406343922019,0.425443404912949,5.4));
#44019=CARTESIAN_POINT('',(2.46074388921261,0.201841765642166,5.37));
#44020=CARTESIAN_POINT('',(2.46074388921261,0.201841765642166,5.4));
#44021=CARTESIAN_POINT('Ctrl Pts',(2.46074388921261,0.201841765642166,5.37));
#44022=CARTESIAN_POINT('Ctrl Pts',(2.406343922019,0.270497941970825,5.37));
#44023=CARTESIAN_POINT('Ctrl Pts',(2.406343922019,0.425443404912949,5.37));
#44024=CARTESIAN_POINT('Ctrl Pts',(2.58567522466183,0.144815826416016,5.4));
#44025=CARTESIAN_POINT('Ctrl Pts',(2.58567522466183,0.144815826416016,5.37));
#44026=CARTESIAN_POINT('Ctrl Pts',(2.5061392635107,0.144815826416016,5.4));
#44027=CARTESIAN_POINT('Ctrl Pts',(2.5061392635107,0.144815826416016,5.37));
#44028=CARTESIAN_POINT('Ctrl Pts',(2.46074388921261,0.201841765642166,5.4));
#44029=CARTESIAN_POINT('Ctrl Pts',(2.46074388921261,0.201841765642166,5.37));
#44030=CARTESIAN_POINT('Ctrl Pts',(2.58567522466183,0.144815826416016,5.4));
#44031=CARTESIAN_POINT('Ctrl Pts',(2.5061392635107,0.144815826416016,5.4));
#44032=CARTESIAN_POINT('Ctrl Pts',(2.46074388921261,0.201841765642166,5.4));
#44033=CARTESIAN_POINT('Ctrl Pts',(2.58567522466183,0.144815826416016,5.37));
#44034=CARTESIAN_POINT('Ctrl Pts',(2.5061392635107,0.144815826416016,5.37));
#44035=CARTESIAN_POINT('Ctrl Pts',(2.46074388921261,0.201841765642166,5.37));
#44036=CARTESIAN_POINT('Origin',(2.58567546308041,0.425630980730057,5.37));
#44037=CARTESIAN_POINT('Ctrl Pts',(1.70252369344234,0.632912719249725,5.4));
#44038=CARTESIAN_POINT('Ctrl Pts',(1.70252369344234,0.632912719249725,5.37));
#44039=CARTESIAN_POINT('Ctrl Pts',(1.74491833150387,0.670804941654205,5.4));
#44040=CARTESIAN_POINT('Ctrl Pts',(1.74491833150387,0.670804941654205,5.37));
#44041=CARTESIAN_POINT('Ctrl Pts',(1.76255129277706,0.706446135044098,5.4));
#44042=CARTESIAN_POINT('Ctrl Pts',(1.76255129277706,0.706446135044098,5.37));
#44043=CARTESIAN_POINT('',(1.70252369344234,0.632912719249725,5.4));
#44044=CARTESIAN_POINT('',(1.76255129277706,0.706446135044098,5.4));
#44045=CARTESIAN_POINT('Ctrl Pts',(1.70252369344234,0.632912719249725,5.4));
#44046=CARTESIAN_POINT('Ctrl Pts',(1.74491833150387,0.670804941654205,5.4));
#44047=CARTESIAN_POINT('Ctrl Pts',(1.76255129277706,0.706446135044098,5.4));
#44048=CARTESIAN_POINT('',(1.70252369344234,0.632912719249725,5.37));
#44049=CARTESIAN_POINT('',(1.70252369344234,0.632912719249725,5.4));
#44050=CARTESIAN_POINT('',(1.76255129277706,0.706446135044098,5.37));
#44051=CARTESIAN_POINT('Ctrl Pts',(1.70252369344234,0.632912719249725,5.37));
#44052=CARTESIAN_POINT('Ctrl Pts',(1.74491833150387,0.670804941654205,5.37));
#44053=CARTESIAN_POINT('Ctrl Pts',(1.76255129277706,0.706446135044098,5.37));
#44054=CARTESIAN_POINT('',(1.76255129277706,0.706446135044098,5.4));
#44055=CARTESIAN_POINT('Ctrl Pts',(1.60347889363766,0.56838338971138,5.4));
#44056=CARTESIAN_POINT('Ctrl Pts',(1.60347889363766,0.56838338971138,5.37));
#44057=CARTESIAN_POINT('Ctrl Pts',(1.66012953221798,0.595020496845245,5.4));
#44058=CARTESIAN_POINT('Ctrl Pts',(1.66012953221798,0.595020496845245,5.37));
#44059=CARTESIAN_POINT('Ctrl Pts',(1.70252369344234,0.632912719249725,5.4));
#44060=CARTESIAN_POINT('Ctrl Pts',(1.70252369344234,0.632912719249725,5.37));
#44061=CARTESIAN_POINT('',(1.60347889363766,0.56838338971138,5.4));
#44062=CARTESIAN_POINT('Ctrl Pts',(1.60347889363766,0.56838338971138,5.4));
#44063=CARTESIAN_POINT('Ctrl Pts',(1.66012953221798,0.595020496845245,5.4));
#44064=CARTESIAN_POINT('Ctrl Pts',(1.70252369344234,0.632912719249725,5.4));
#44065=CARTESIAN_POINT('',(1.60347889363766,0.56838338971138,5.37));
#44066=CARTESIAN_POINT('',(1.60347889363766,0.56838338971138,5.4));
#44067=CARTESIAN_POINT('Ctrl Pts',(1.60347889363766,0.56838338971138,5.37));
#44068=CARTESIAN_POINT('Ctrl Pts',(1.66012953221798,0.595020496845245,5.37));
#44069=CARTESIAN_POINT('Ctrl Pts',(1.70252369344234,0.632912719249725,5.37));
#44070=CARTESIAN_POINT('Origin',(1.60347889363766,0.503103697299957,5.4));
#44071=CARTESIAN_POINT('',(1.60347889363766,0.503103697299957,5.4));
#44072=CARTESIAN_POINT('',(1.60347889363766,0.251551848649979,5.4));
#44073=CARTESIAN_POINT('',(1.60347889363766,0.503103697299957,5.37));
#44074=CARTESIAN_POINT('',(1.60347889363766,0.503103697299957,5.4));
#44075=CARTESIAN_POINT('',(1.60347889363766,0.503103697299957,5.37));
#44076=CARTESIAN_POINT('Ctrl Pts',(1.67457388341427,0.537994557619095,5.4));
#44077=CARTESIAN_POINT('Ctrl Pts',(1.67457388341427,0.537994557619095,5.37));
#44078=CARTESIAN_POINT('Ctrl Pts',(1.6349930614233,0.514733994007111,5.4));
#44079=CARTESIAN_POINT('Ctrl Pts',(1.6349930614233,0.514733994007111,5.37));
#44080=CARTESIAN_POINT('Ctrl Pts',(1.60347889363766,0.503103697299957,5.4));
#44081=CARTESIAN_POINT('Ctrl Pts',(1.60347889363766,0.503103697299957,5.37));
#44082=CARTESIAN_POINT('',(1.67457388341427,0.537994557619095,5.4));
#44083=CARTESIAN_POINT('Ctrl Pts',(1.67457388341427,0.537994557619095,5.4));
#44084=CARTESIAN_POINT('Ctrl Pts',(1.6349930614233,0.514733994007111,5.4));
#44085=CARTESIAN_POINT('Ctrl Pts',(1.60347889363766,0.503103697299957,5.4));
#44086=CARTESIAN_POINT('',(1.67457388341427,0.537994557619095,5.37));
#44087=CARTESIAN_POINT('',(1.67457388341427,0.537994557619095,5.4));
#44088=CARTESIAN_POINT('Ctrl Pts',(1.67457388341427,0.537994557619095,5.37));
#44089=CARTESIAN_POINT('Ctrl Pts',(1.6349930614233,0.514733994007111,5.37));
#44090=CARTESIAN_POINT('Ctrl Pts',(1.60347889363766,0.503103697299957,5.37));
#44091=CARTESIAN_POINT('Ctrl Pts',(1.73854015767574,0.584515714645386,5.4));
#44092=CARTESIAN_POINT('Ctrl Pts',(1.73854015767574,0.584515714645386,5.37));
#44093=CARTESIAN_POINT('Ctrl Pts',(1.71415422856808,0.561255151033402,5.4));
#44094=CARTESIAN_POINT('Ctrl Pts',(1.71415422856808,0.561255151033402,5.37));
#44095=CARTESIAN_POINT('Ctrl Pts',(1.67457388341427,0.537994557619095,5.4));
#44096=CARTESIAN_POINT('Ctrl Pts',(1.67457388341427,0.537994557619095,5.37));
#44097=CARTESIAN_POINT('',(1.73854015767574,0.584515714645386,5.4));
#44098=CARTESIAN_POINT('Ctrl Pts',(1.73854015767574,0.584515714645386,5.4));
#44099=CARTESIAN_POINT('Ctrl Pts',(1.71415422856808,0.561255151033402,5.4));
#44100=CARTESIAN_POINT('Ctrl Pts',(1.67457388341427,0.537994557619095,5.4));
#44101=CARTESIAN_POINT('',(1.73854015767574,0.584515714645386,5.37));
#44102=CARTESIAN_POINT('',(1.73854015767574,0.584515714645386,5.4));
#44103=CARTESIAN_POINT('Ctrl Pts',(1.73854015767574,0.584515714645386,5.37));
#44104=CARTESIAN_POINT('Ctrl Pts',(1.71415422856808,0.561255151033402,5.37));
#44105=CARTESIAN_POINT('Ctrl Pts',(1.67457388341427,0.537994557619095,5.37));
#44106=CARTESIAN_POINT('Origin',(1.73854015767574,0.154195094108582,5.4));
#44107=CARTESIAN_POINT('',(1.73854015767574,0.154195094108582,5.4));
#44108=CARTESIAN_POINT('',(1.73854015767574,0.0770975470542908,5.4));
#44109=CARTESIAN_POINT('',(1.73854015767574,0.154195094108582,5.37));
#44110=CARTESIAN_POINT('',(1.73854015767574,0.154195094108582,5.4));
#44111=CARTESIAN_POINT('',(1.73854015767574,0.154195094108582,5.37));
#44112=CARTESIAN_POINT('Origin',(1.80607078969479,0.154195094108582,5.4));
#44113=CARTESIAN_POINT('',(1.80607078969479,0.154195094108582,5.4));
#44114=CARTESIAN_POINT('',(0.903035394847393,0.154195094108582,5.4));
#44115=CARTESIAN_POINT('',(1.80607078969479,0.154195094108582,5.37));
#44116=CARTESIAN_POINT('',(1.80607078969479,0.154195094108582,5.4));
#44117=CARTESIAN_POINT('',(1.80607078969479,0.154195094108582,5.37));
#44118=CARTESIAN_POINT('Origin',(1.80607078969479,0.706446135044098,5.4));
#44119=CARTESIAN_POINT('',(1.80607078969479,0.706446135044098,5.4));
#44120=CARTESIAN_POINT('',(1.80607078969479,0.353223067522049,5.4));
#44121=CARTESIAN_POINT('',(1.80607078969479,0.706446135044098,5.37));
#44122=CARTESIAN_POINT('',(1.80607078969479,0.706446135044098,5.4));
#44123=CARTESIAN_POINT('',(1.80607078969479,0.706446135044098,5.37));
#44124=CARTESIAN_POINT('Origin',(1.76255129277706,0.706446135044098,5.4));
#44125=CARTESIAN_POINT('',(0.881275646388531,0.706446135044098,5.4));
#44126=CARTESIAN_POINT('',(1.76255129277706,0.706446135044098,5.37));
#44127=CARTESIAN_POINT('Origin',(1.70477484166622,0.43032061457634,5.37));
#44128=CARTESIAN_POINT('Origin',(-2.53577782213688,0.154195094108582,5.4));
#44129=CARTESIAN_POINT('',(-2.53577782213688,0.154195094108582,5.4));
#44130=CARTESIAN_POINT('',(-2.69485013186932,0.622407937049866,5.4));
#44131=CARTESIAN_POINT('',(-2.38109215733969,-0.301106114497601,5.4));
#44132=CARTESIAN_POINT('',(-2.53577782213688,0.154195094108582,5.37));
#44133=CARTESIAN_POINT('',(-2.53577782213688,0.154195094108582,5.4));
#44134=CARTESIAN_POINT('',(-2.69485013186932,0.622407937049866,5.37));
#44135=CARTESIAN_POINT('',(-2.53577782213688,0.154195094108582,5.37));
#44136=CARTESIAN_POINT('',(-2.69485013186932,0.622407937049866,5.4));
#44137=CARTESIAN_POINT('Origin',(-2.47012294828892,0.154195094108582,5.4));
#44138=CARTESIAN_POINT('',(-2.47012294828892,0.154195094108582,5.4));
#44139=CARTESIAN_POINT('',(-1.23506147414446,0.154195094108582,5.4));
#44140=CARTESIAN_POINT('',(-2.47012294828892,0.154195094108582,5.37));
#44141=CARTESIAN_POINT('',(-2.47012294828892,0.154195094108582,5.4));
#44142=CARTESIAN_POINT('',(-2.47012294828892,0.154195094108582,5.37));
#44143=CARTESIAN_POINT('Origin',(-2.31030030548573,0.614529365301132,5.4));
#44144=CARTESIAN_POINT('',(-2.31030030548573,0.614529365301132,5.4));
#44145=CARTESIAN_POINT('',(-2.28124043684146,0.698229980049323,5.4));
#44146=CARTESIAN_POINT('',(-2.31030030548573,0.614529365301132,5.37));
#44147=CARTESIAN_POINT('',(-2.31030030548573,0.614529365301132,5.4));
#44148=CARTESIAN_POINT('',(-2.31030030548573,0.614529365301132,5.37));
#44149=CARTESIAN_POINT('Origin',(-2.31030030548573,0.154195094108582,5.4));
#44150=CARTESIAN_POINT('',(-2.31030030548573,0.154195094108582,5.4));
#44151=CARTESIAN_POINT('',(-2.31030030548573,0.0770975470542908,5.4));
#44152=CARTESIAN_POINT('',(-2.31030030548573,0.154195094108582,5.37));
#44153=CARTESIAN_POINT('',(-2.31030030548573,0.154195094108582,5.4));
#44154=CARTESIAN_POINT('',(-2.31030030548573,0.154195094108582,5.37));
#44155=CARTESIAN_POINT('Origin',(-2.24014343321323,0.154195094108582,5.4));
#44156=CARTESIAN_POINT('',(-2.24014343321323,0.154195094108582,5.4));
#44157=CARTESIAN_POINT('',(-1.12007171660662,0.154195094108582,5.4));
#44158=CARTESIAN_POINT('',(-2.24014343321323,0.154195094108582,5.37));
#44159=CARTESIAN_POINT('',(-2.24014343321323,0.154195094108582,5.4));
#44160=CARTESIAN_POINT('',(-2.24014343321323,0.154195094108582,5.37));
#44161=CARTESIAN_POINT('Origin',(-2.24014343321323,0.704195106029511,5.4));
#44162=CARTESIAN_POINT('',(-2.24014343321323,0.704195106029511,5.4));
#44163=CARTESIAN_POINT('',(-2.24014343321323,0.352097553014755,5.4));
#44164=CARTESIAN_POINT('',(-2.24014343321323,0.704195106029511,5.37));
#44165=CARTESIAN_POINT('',(-2.24014343321323,0.704195106029511,5.4));
#44166=CARTESIAN_POINT('',(-2.24014343321323,0.704195106029511,5.37));
#44167=CARTESIAN_POINT('Origin',(-2.33806295692921,0.704195106029511,5.4));
#44168=CARTESIAN_POINT('',(-2.33806295692921,0.704195106029511,5.4));
#44169=CARTESIAN_POINT('',(-1.1690314784646,0.704195106029511,5.4));
#44170=CARTESIAN_POINT('',(-2.33806295692921,0.704195106029511,5.37));
#44171=CARTESIAN_POINT('',(-2.33806295692921,0.704195106029511,5.4));
#44172=CARTESIAN_POINT('',(-2.33806295692921,0.704195106029511,5.37));
#44173=CARTESIAN_POINT('Origin',(-2.4697477966547,0.321521157026291,5.4));
#44174=CARTESIAN_POINT('',(-2.4697477966547,0.321521157026291,5.4));
#44175=CARTESIAN_POINT('',(-2.38846377938169,0.557731156184516,5.4));
#44176=CARTESIAN_POINT('',(-2.4697477966547,0.321521157026291,5.37));
#44177=CARTESIAN_POINT('',(-2.4697477966547,0.321521157026291,5.4));
#44178=CARTESIAN_POINT('',(-2.4697477966547,0.321521157026291,5.37));
#44179=CARTESIAN_POINT('Ctrl Pts',(-2.49901111423969,0.233356082439423,
5.4));
#44180=CARTESIAN_POINT('Ctrl Pts',(-2.49901111423969,0.233356082439423,
5.37));
#44181=CARTESIAN_POINT('Ctrl Pts',(-2.48963184654713,0.263369733095169,
5.4));
#44182=CARTESIAN_POINT('Ctrl Pts',(-2.48963184654713,0.263369733095169,
5.37));
#44183=CARTESIAN_POINT('Ctrl Pts',(-2.4697477966547,0.321521157026291,5.4));
#44184=CARTESIAN_POINT('Ctrl Pts',(-2.4697477966547,0.321521157026291,5.37));
#44185=CARTESIAN_POINT('',(-2.49901111423969,0.233356082439423,5.4));
#44186=CARTESIAN_POINT('Ctrl Pts',(-2.49901111423969,0.233356082439423,
5.4));
#44187=CARTESIAN_POINT('Ctrl Pts',(-2.48963184654713,0.263369733095169,
5.4));
#44188=CARTESIAN_POINT('Ctrl Pts',(-2.4697477966547,0.321521157026291,5.4));
#44189=CARTESIAN_POINT('',(-2.49901111423969,0.233356082439423,5.37));
#44190=CARTESIAN_POINT('',(-2.49901111423969,0.233356082439423,5.4));
#44191=CARTESIAN_POINT('Ctrl Pts',(-2.49901111423969,0.233356082439423,
5.37));
#44192=CARTESIAN_POINT('Ctrl Pts',(-2.48963184654713,0.263369733095169,
5.37));
#44193=CARTESIAN_POINT('Ctrl Pts',(-2.4697477966547,0.321521157026291,5.37));
#44194=CARTESIAN_POINT('Ctrl Pts',(-2.52527303993702,0.31476808488369,5.4));
#44195=CARTESIAN_POINT('Ctrl Pts',(-2.52527303993702,0.31476808488369,5.37));
#44196=CARTESIAN_POINT('Ctrl Pts',(-2.50726486742496,0.260368371009827,
5.4));
#44197=CARTESIAN_POINT('Ctrl Pts',(-2.50726486742496,0.260368371009827,
5.37));
#44198=CARTESIAN_POINT('Ctrl Pts',(-2.49901111423969,0.233356082439423,
5.4));
#44199=CARTESIAN_POINT('Ctrl Pts',(-2.49901111423969,0.233356082439423,
5.37));
#44200=CARTESIAN_POINT('',(-2.52527303993702,0.31476808488369,5.4));
#44201=CARTESIAN_POINT('Ctrl Pts',(-2.52527303993702,0.31476808488369,5.4));
#44202=CARTESIAN_POINT('Ctrl Pts',(-2.50726486742496,0.260368371009827,
5.4));
#44203=CARTESIAN_POINT('Ctrl Pts',(-2.49901111423969,0.233356082439423,
5.4));
#44204=CARTESIAN_POINT('',(-2.52527303993702,0.31476808488369,5.37));
#44205=CARTESIAN_POINT('',(-2.52527303993702,0.31476808488369,5.4));
#44206=CARTESIAN_POINT('Ctrl Pts',(-2.52527303993702,0.31476808488369,5.37));
#44207=CARTESIAN_POINT('Ctrl Pts',(-2.50726486742496,0.260368371009827,
5.37));
#44208=CARTESIAN_POINT('Ctrl Pts',(-2.49901111423969,0.233356082439423,
5.37));
#44209=CARTESIAN_POINT('Origin',(-2.655457213521,0.704195106029511,5.4));
#44210=CARTESIAN_POINT('',(-2.655457213521,0.704195106029511,5.4));
#44211=CARTESIAN_POINT('',(-2.41611977305377,-0.0117480376252982,5.4));
#44212=CARTESIAN_POINT('',(-2.655457213521,0.704195106029511,5.37));
#44213=CARTESIAN_POINT('',(-2.655457213521,0.704195106029511,5.4));
#44214=CARTESIAN_POINT('',(-2.655457213521,0.704195106029511,5.37));
#44215=CARTESIAN_POINT('Origin',(-2.76500703394413,0.704195106029511,5.4));
#44216=CARTESIAN_POINT('',(-2.76500703394413,0.704195106029511,5.4));
#44217=CARTESIAN_POINT('',(-1.38250351697206,0.704195106029511,5.4));
#44218=CARTESIAN_POINT('',(-2.76500703394413,0.704195106029511,5.37));
#44219=CARTESIAN_POINT('',(-2.76500703394413,0.704195106029511,5.4));
#44220=CARTESIAN_POINT('',(-2.76500703394413,0.704195106029511,5.37));
#44221=CARTESIAN_POINT('Origin',(-2.76500703394413,0.154195094108582,5.4));
#44222=CARTESIAN_POINT('',(-2.76500703394413,0.154195094108582,5.4));
#44223=CARTESIAN_POINT('',(-2.76500703394413,0.0770975470542908,5.4));
#44224=CARTESIAN_POINT('',(-2.76500703394413,0.154195094108582,5.37));
#44225=CARTESIAN_POINT('',(-2.76500703394413,0.154195094108582,5.4));
#44226=CARTESIAN_POINT('',(-2.76500703394413,0.154195094108582,5.37));
#44227=CARTESIAN_POINT('Origin',(-2.69485013186932,0.154195094108582,5.4));
#44228=CARTESIAN_POINT('',(-2.69485013186932,0.154195094108582,5.4));
#44229=CARTESIAN_POINT('',(-1.34742506593466,0.154195094108582,5.4));
#44230=CARTESIAN_POINT('',(-2.69485013186932,0.154195094108582,5.37));
#44231=CARTESIAN_POINT('',(-2.69485013186932,0.154195094108582,5.4));
#44232=CARTESIAN_POINT('',(-2.69485013186932,0.154195094108582,5.37));
#44233=CARTESIAN_POINT('Origin',(-2.69485013186932,0.622407937049866,5.4));
#44234=CARTESIAN_POINT('',(-2.69485013186932,0.311203968524933,5.4));
#44235=CARTESIAN_POINT('',(-2.69485013186932,0.622407937049866,5.37));
#44236=CARTESIAN_POINT('Origin',(-2.50257523357868,0.429195100069046,5.37));
#44237=CARTESIAN_POINT('Ctrl Pts',(-0.133935943245888,0.194525921344757,
5.4));
#44238=CARTESIAN_POINT('Ctrl Pts',(-0.133935943245888,0.194525921344757,
5.37));
#44239=CARTESIAN_POINT('Ctrl Pts',(-0.186459794640541,0.144440674781799,
5.4));
#44240=CARTESIAN_POINT('Ctrl Pts',(-0.186459794640541,0.144440674781799,
5.37));
#44241=CARTESIAN_POINT('Ctrl Pts',(-0.266746297478676,0.144440674781799,
5.4));
#44242=CARTESIAN_POINT('Ctrl Pts',(-0.266746297478676,0.144440674781799,
5.37));
#44243=CARTESIAN_POINT('',(-0.133935943245888,0.194525921344757,5.4));
#44244=CARTESIAN_POINT('',(-0.266746297478676,0.144440674781799,5.4));
#44245=CARTESIAN_POINT('Ctrl Pts',(-0.133935943245888,0.194525921344757,
5.4));
#44246=CARTESIAN_POINT('Ctrl Pts',(-0.186459794640541,0.144440674781799,
5.4));
#44247=CARTESIAN_POINT('Ctrl Pts',(-0.266746297478676,0.144440674781799,
5.4));
#44248=CARTESIAN_POINT('',(-0.133935943245888,0.194525921344757,5.37));
#44249=CARTESIAN_POINT('',(-0.133935943245888,0.194525921344757,5.4));
#44250=CARTESIAN_POINT('',(-0.266746297478676,0.144440674781799,5.37));
#44251=CARTESIAN_POINT('Ctrl Pts',(-0.133935943245888,0.194525921344757,
5.37));
#44252=CARTESIAN_POINT('Ctrl Pts',(-0.186459794640541,0.144440674781799,
5.37));
#44253=CARTESIAN_POINT('Ctrl Pts',(-0.266746297478676,0.144440674781799,
5.37));
#44254=CARTESIAN_POINT('',(-0.266746297478676,0.144440674781799,5.4));
#44255=CARTESIAN_POINT('Ctrl Pts',(-0.0814120918512344,0.316643932461739,
5.4));
#44256=CARTESIAN_POINT('Ctrl Pts',(-0.0814120918512344,0.316643932461739,
5.37));
#44257=CARTESIAN_POINT('Ctrl Pts',(-0.0814120918512344,0.244611197710037,
5.4));
#44258=CARTESIAN_POINT('Ctrl Pts',(-0.0814120918512344,0.244611197710037,
5.37));
#44259=CARTESIAN_POINT('Ctrl Pts',(-0.133935943245888,0.194525921344757,
5.4));
#44260=CARTESIAN_POINT('Ctrl Pts',(-0.133935943245888,0.194525921344757,
5.37));
#44261=CARTESIAN_POINT('',(-0.0814120918512344,0.316643932461739,5.4));
#44262=CARTESIAN_POINT('Ctrl Pts',(-0.0814120918512344,0.316643932461739,
5.4));
#44263=CARTESIAN_POINT('Ctrl Pts',(-0.0814120918512344,0.244611197710037,
5.4));
#44264=CARTESIAN_POINT('Ctrl Pts',(-0.133935943245888,0.194525921344757,
5.4));
#44265=CARTESIAN_POINT('',(-0.0814120918512344,0.316643932461739,5.37));
#44266=CARTESIAN_POINT('',(-0.0814120918512344,0.316643932461739,5.4));
#44267=CARTESIAN_POINT('Ctrl Pts',(-0.0814120918512344,0.316643932461739,
5.37));
#44268=CARTESIAN_POINT('Ctrl Pts',(-0.0814120918512344,0.244611197710037,
5.37));
#44269=CARTESIAN_POINT('Ctrl Pts',(-0.133935943245888,0.194525921344757,
5.37));
#44270=CARTESIAN_POINT('Ctrl Pts',(-0.108424201607704,0.405371749401093,
5.4));
#44271=CARTESIAN_POINT('Ctrl Pts',(-0.108424201607704,0.405371749401093,
5.37));
#44272=CARTESIAN_POINT('Ctrl Pts',(-0.0814120918512344,0.369918146729469,
5.4));
#44273=CARTESIAN_POINT('Ctrl Pts',(-0.0814120918512344,0.369918146729469,
5.37));
#44274=CARTESIAN_POINT('Ctrl Pts',(-0.0814120918512344,0.316643932461739,
5.4));
#44275=CARTESIAN_POINT('Ctrl Pts',(-0.0814120918512344,0.316643932461739,
5.37));
#44276=CARTESIAN_POINT('',(-0.108424201607704,0.405371749401093,5.4));
#44277=CARTESIAN_POINT('Ctrl Pts',(-0.108424201607704,0.405371749401093,
5.4));
#44278=CARTESIAN_POINT('Ctrl Pts',(-0.0814120918512344,0.369918146729469,
5.4));
#44279=CARTESIAN_POINT('Ctrl Pts',(-0.0814120918512344,0.316643932461739,
5.4));
#44280=CARTESIAN_POINT('',(-0.108424201607704,0.405371749401093,5.37));
#44281=CARTESIAN_POINT('',(-0.108424201607704,0.405371749401093,5.4));
#44282=CARTESIAN_POINT('Ctrl Pts',(-0.108424201607704,0.405371749401093,
5.37));
#44283=CARTESIAN_POINT('Ctrl Pts',(-0.0814120918512344,0.369918146729469,
5.37));
#44284=CARTESIAN_POINT('Ctrl Pts',(-0.0814120918512344,0.316643932461739,
5.37));
#44285=CARTESIAN_POINT('Ctrl Pts',(-0.184208884835243,0.452080512046814,
5.4));
#44286=CARTESIAN_POINT('Ctrl Pts',(-0.184208884835243,0.452080512046814,
5.37));
#44287=CARTESIAN_POINT('Ctrl Pts',(-0.135436549782753,0.440825366973877,
5.4));
#44288=CARTESIAN_POINT('Ctrl Pts',(-0.135436549782753,0.440825366973877,
5.37));
#44289=CARTESIAN_POINT('Ctrl Pts',(-0.108424201607704,0.405371749401093,
5.4));
#44290=CARTESIAN_POINT('Ctrl Pts',(-0.108424201607704,0.405371749401093,
5.37));
#44291=CARTESIAN_POINT('',(-0.184208884835243,0.452080512046814,5.4));
#44292=CARTESIAN_POINT('Ctrl Pts',(-0.184208884835243,0.452080512046814,
5.4));
#44293=CARTESIAN_POINT('Ctrl Pts',(-0.135436549782753,0.440825366973877,
5.4));
#44294=CARTESIAN_POINT('Ctrl Pts',(-0.108424201607704,0.405371749401093,
5.4));
#44295=CARTESIAN_POINT('',(-0.184208884835243,0.452080512046814,5.37));
#44296=CARTESIAN_POINT('',(-0.184208884835243,0.452080512046814,5.4));
#44297=CARTESIAN_POINT('Ctrl Pts',(-0.184208884835243,0.452080512046814,
5.37));
#44298=CARTESIAN_POINT('Ctrl Pts',(-0.135436549782753,0.440825366973877,
5.37));
#44299=CARTESIAN_POINT('Ctrl Pts',(-0.108424201607704,0.405371749401093,
5.37));
#44300=CARTESIAN_POINT('Ctrl Pts',(-0.127558007836342,0.498601639270782,
5.4));
#44301=CARTESIAN_POINT('Ctrl Pts',(-0.127558007836342,0.498601639270782,
5.37));
#44302=CARTESIAN_POINT('Ctrl Pts',(-0.14669181406498,0.469338321685791,
5.4));
#44303=CARTESIAN_POINT('Ctrl Pts',(-0.14669181406498,0.469338321685791,
5.37));
#44304=CARTESIAN_POINT('Ctrl Pts',(-0.184208884835243,0.452080512046814,
5.4));
#44305=CARTESIAN_POINT('Ctrl Pts',(-0.184208884835243,0.452080512046814,
5.37));
#44306=CARTESIAN_POINT('',(-0.127558007836342,0.498601639270782,5.4));
#44307=CARTESIAN_POINT('Ctrl Pts',(-0.127558007836342,0.498601639270782,
5.4));
#44308=CARTESIAN_POINT('Ctrl Pts',(-0.14669181406498,0.469338321685791,
5.4));
#44309=CARTESIAN_POINT('Ctrl Pts',(-0.184208884835243,0.452080512046814,
5.4));
#44310=CARTESIAN_POINT('',(-0.127558007836342,0.498601639270782,5.37));
#44311=CARTESIAN_POINT('',(-0.127558007836342,0.498601639270782,5.4));
#44312=CARTESIAN_POINT('Ctrl Pts',(-0.127558007836342,0.498601639270782,
5.37));
#44313=CARTESIAN_POINT('Ctrl Pts',(-0.14669181406498,0.469338321685791,
5.37));
#44314=CARTESIAN_POINT('Ctrl Pts',(-0.184208884835243,0.452080512046814,
5.37));
#44315=CARTESIAN_POINT('Ctrl Pts',(-0.108424201607704,0.563506150245667,
5.4));
#44316=CARTESIAN_POINT('Ctrl Pts',(-0.108424201607704,0.563506150245667,
5.37));
#44317=CARTESIAN_POINT('Ctrl Pts',(-0.108424201607704,0.527864956855774,
5.4));
#44318=CARTESIAN_POINT('Ctrl Pts',(-0.108424201607704,0.527864956855774,
5.37));
#44319=CARTESIAN_POINT('Ctrl Pts',(-0.127558007836342,0.498601639270782,
5.4));
#44320=CARTESIAN_POINT('Ctrl Pts',(-0.127558007836342,0.498601639270782,
5.37));
#44321=CARTESIAN_POINT('',(-0.108424201607704,0.563506150245667,5.4));
#44322=CARTESIAN_POINT('Ctrl Pts',(-0.108424201607704,0.563506150245667,
5.4));
#44323=CARTESIAN_POINT('Ctrl Pts',(-0.108424201607704,0.527864956855774,
5.4));
#44324=CARTESIAN_POINT('Ctrl Pts',(-0.127558007836342,0.498601639270782,
5.4));
#44325=CARTESIAN_POINT('',(-0.108424201607704,0.563506150245667,5.37));
#44326=CARTESIAN_POINT('',(-0.108424201607704,0.563506150245667,5.4));
#44327=CARTESIAN_POINT('Ctrl Pts',(-0.108424201607704,0.563506150245667,
5.37));
#44328=CARTESIAN_POINT('Ctrl Pts',(-0.108424201607704,0.527864956855774,
5.37));
#44329=CARTESIAN_POINT('Ctrl Pts',(-0.127558007836342,0.498601639270782,
5.37));
#44330=CARTESIAN_POINT('Ctrl Pts',(-0.128495946526527,0.634413385391235,
5.4));
#44331=CARTESIAN_POINT('Ctrl Pts',(-0.128495946526527,0.634413385391235,
5.37));
#44332=CARTESIAN_POINT('Ctrl Pts',(-0.108424201607704,0.601023161411285,
5.4));
#44333=CARTESIAN_POINT('Ctrl Pts',(-0.108424201607704,0.601023161411285,
5.37));
#44334=CARTESIAN_POINT('Ctrl Pts',(-0.108424201607704,0.563506150245667,
5.4));
#44335=CARTESIAN_POINT('Ctrl Pts',(-0.108424201607704,0.563506150245667,
5.37));
#44336=CARTESIAN_POINT('',(-0.128495946526527,0.634413385391235,5.4));
#44337=CARTESIAN_POINT('Ctrl Pts',(-0.128495946526527,0.634413385391235,
5.4));
#44338=CARTESIAN_POINT('Ctrl Pts',(-0.108424201607704,0.601023161411285,
5.4));
#44339=CARTESIAN_POINT('Ctrl Pts',(-0.108424201607704,0.563506150245667,
5.4));
#44340=CARTESIAN_POINT('',(-0.128495946526527,0.634413385391235,5.37));
#44341=CARTESIAN_POINT('',(-0.128495946526527,0.634413385391235,5.4));
#44342=CARTESIAN_POINT('Ctrl Pts',(-0.128495946526527,0.634413385391235,
5.37));
#44343=CARTESIAN_POINT('Ctrl Pts',(-0.108424201607704,0.601023161411285,
5.37));
#44344=CARTESIAN_POINT('Ctrl Pts',(-0.108424201607704,0.563506150245667,
5.37));
#44345=CARTESIAN_POINT('Ctrl Pts',(-0.186459794640541,0.687124812602997,
5.4));
#44346=CARTESIAN_POINT('Ctrl Pts',(-0.186459794640541,0.687124812602997,
5.37));
#44347=CARTESIAN_POINT('Ctrl Pts',(-0.148567691445351,0.667803549766541,
5.4));
#44348=CARTESIAN_POINT('Ctrl Pts',(-0.148567691445351,0.667803549766541,
5.37));
#44349=CARTESIAN_POINT('Ctrl Pts',(-0.128495946526527,0.634413385391235,
5.4));
#44350=CARTESIAN_POINT('Ctrl Pts',(-0.128495946526527,0.634413385391235,
5.37));
#44351=CARTESIAN_POINT('',(-0.186459794640541,0.687124812602997,5.4));
#44352=CARTESIAN_POINT('Ctrl Pts',(-0.186459794640541,0.687124812602997,
5.4));
#44353=CARTESIAN_POINT('Ctrl Pts',(-0.148567691445351,0.667803549766541,
5.4));
#44354=CARTESIAN_POINT('Ctrl Pts',(-0.128495946526527,0.634413385391235,
5.4));
#44355=CARTESIAN_POINT('',(-0.186459794640541,0.687124812602997,5.37));
#44356=CARTESIAN_POINT('',(-0.186459794640541,0.687124812602997,5.4));
#44357=CARTESIAN_POINT('Ctrl Pts',(-0.186459794640541,0.687124812602997,
5.37));
#44358=CARTESIAN_POINT('Ctrl Pts',(-0.148567691445351,0.667803549766541,
5.37));
#44359=CARTESIAN_POINT('Ctrl Pts',(-0.128495946526527,0.634413385391235,
5.37));
#44360=CARTESIAN_POINT('Ctrl Pts',(-0.26937247812748,0.706446135044098,
5.4));
#44361=CARTESIAN_POINT('Ctrl Pts',(-0.26937247812748,0.706446135044098,
5.37));
#44362=CARTESIAN_POINT('Ctrl Pts',(-0.224352136254311,0.706446135044098,
5.4));
#44363=CARTESIAN_POINT('Ctrl Pts',(-0.224352136254311,0.706446135044098,
5.37));
#44364=CARTESIAN_POINT('Ctrl Pts',(-0.186459794640541,0.687124812602997,
5.4));
#44365=CARTESIAN_POINT('Ctrl Pts',(-0.186459794640541,0.687124812602997,
5.37));
#44366=CARTESIAN_POINT('',(-0.26937247812748,0.706446135044098,5.4));
#44367=CARTESIAN_POINT('Ctrl Pts',(-0.26937247812748,0.706446135044098,
5.4));
#44368=CARTESIAN_POINT('Ctrl Pts',(-0.224352136254311,0.706446135044098,
5.4));
#44369=CARTESIAN_POINT('Ctrl Pts',(-0.186459794640541,0.687124812602997,
5.4));
#44370=CARTESIAN_POINT('',(-0.26937247812748,0.706446135044098,5.37));
#44371=CARTESIAN_POINT('',(-0.26937247812748,0.706446135044098,5.4));
#44372=CARTESIAN_POINT('Ctrl Pts',(-0.26937247812748,0.706446135044098,
5.37));
#44373=CARTESIAN_POINT('Ctrl Pts',(-0.224352136254311,0.706446135044098,
5.37));
#44374=CARTESIAN_POINT('Ctrl Pts',(-0.186459794640541,0.687124812602997,
5.37));
#44375=CARTESIAN_POINT('Ctrl Pts',(-0.378547206521034,0.669116640090942,
5.4));
#44376=CARTESIAN_POINT('Ctrl Pts',(-0.378547206521034,0.669116640090942,
5.37));
#44377=CARTESIAN_POINT('Ctrl Pts',(-0.334652200341225,0.706446135044098,
5.4));
#44378=CARTESIAN_POINT('Ctrl Pts',(-0.334652200341225,0.706446135044098,
5.37));
#44379=CARTESIAN_POINT('Ctrl Pts',(-0.26937247812748,0.706446135044098,
5.4));
#44380=CARTESIAN_POINT('Ctrl Pts',(-0.26937247812748,0.706446135044098,
5.37));
#44381=CARTESIAN_POINT('',(-0.378547206521034,0.669116640090942,5.4));
#44382=CARTESIAN_POINT('Ctrl Pts',(-0.378547206521034,0.669116640090942,
5.4));
#44383=CARTESIAN_POINT('Ctrl Pts',(-0.334652200341225,0.706446135044098,
5.4));
#44384=CARTESIAN_POINT('Ctrl Pts',(-0.26937247812748,0.706446135044098,
5.4));
#44385=CARTESIAN_POINT('',(-0.378547206521034,0.669116640090942,5.37));
#44386=CARTESIAN_POINT('',(-0.378547206521034,0.669116640090942,5.4));
#44387=CARTESIAN_POINT('Ctrl Pts',(-0.378547206521034,0.669116640090942,
5.37));
#44388=CARTESIAN_POINT('Ctrl Pts',(-0.334652200341225,0.706446135044098,
5.37));
#44389=CARTESIAN_POINT('Ctrl Pts',(-0.26937247812748,0.706446135044098,
5.37));
#44390=CARTESIAN_POINT('Ctrl Pts',(-0.43482281267643,0.563881301879883,
5.4));
#44391=CARTESIAN_POINT('Ctrl Pts',(-0.43482281267643,0.563881301879883,
5.37));
#44392=CARTESIAN_POINT('Ctrl Pts',(-0.422441974282265,0.631787145137787,
5.4));
#44393=CARTESIAN_POINT('Ctrl Pts',(-0.422441974282265,0.631787145137787,
5.37));
#44394=CARTESIAN_POINT('Ctrl Pts',(-0.378547206521034,0.669116640090942,
5.4));
#44395=CARTESIAN_POINT('Ctrl Pts',(-0.378547206521034,0.669116640090942,
5.37));
#44396=CARTESIAN_POINT('',(-0.43482281267643,0.563881301879883,5.4));
#44397=CARTESIAN_POINT('Ctrl Pts',(-0.43482281267643,0.563881301879883,
5.4));
#44398=CARTESIAN_POINT('Ctrl Pts',(-0.422441974282265,0.631787145137787,
5.4));
#44399=CARTESIAN_POINT('Ctrl Pts',(-0.378547206521034,0.669116640090942,
5.4));
#44400=CARTESIAN_POINT('',(-0.43482281267643,0.563881301879883,5.37));
#44401=CARTESIAN_POINT('',(-0.43482281267643,0.563881301879883,5.4));
#44402=CARTESIAN_POINT('Ctrl Pts',(-0.43482281267643,0.563881301879883,
5.37));
#44403=CARTESIAN_POINT('Ctrl Pts',(-0.422441974282265,0.631787145137787,
5.37));
#44404=CARTESIAN_POINT('Ctrl Pts',(-0.378547206521034,0.669116640090942,
5.37));
#44405=CARTESIAN_POINT('Origin',(-0.367291942238808,0.551875853538513,5.4));
#44406=CARTESIAN_POINT('',(-0.367291942238808,0.551875853538513,5.4));
#44407=CARTESIAN_POINT('',(-0.141719653140393,0.511774245985313,5.4));
#44408=CARTESIAN_POINT('',(-0.367291942238808,0.551875853538513,5.37));
#44409=CARTESIAN_POINT('',(-0.367291942238808,0.551875853538513,5.4));
#44410=CARTESIAN_POINT('',(-0.367291942238808,0.551875853538513,5.37));
#44411=CARTESIAN_POINT('Ctrl Pts',(-0.333526626229286,0.626159632205963,
5.4));
#44412=CARTESIAN_POINT('Ctrl Pts',(-0.333526626229286,0.626159632205963,
5.37));
#44413=CARTESIAN_POINT('Ctrl Pts',(-0.359788671135902,0.601398372650147,
5.4));
#44414=CARTESIAN_POINT('Ctrl Pts',(-0.359788671135902,0.601398372650147,
5.37));
#44415=CARTESIAN_POINT('Ctrl Pts',(-0.367291942238808,0.551875853538513,
5.4));
#44416=CARTESIAN_POINT('Ctrl Pts',(-0.367291942238808,0.551875853538513,
5.37));
#44417=CARTESIAN_POINT('',(-0.333526626229286,0.626159632205963,5.4));
#44418=CARTESIAN_POINT('Ctrl Pts',(-0.333526626229286,0.626159632205963,
5.4));
#44419=CARTESIAN_POINT('Ctrl Pts',(-0.359788671135902,0.601398372650147,
5.4));
#44420=CARTESIAN_POINT('Ctrl Pts',(-0.367291942238808,0.551875853538513,
5.4));
#44421=CARTESIAN_POINT('',(-0.333526626229286,0.626159632205963,5.37));
#44422=CARTESIAN_POINT('',(-0.333526626229286,0.626159632205963,5.4));
#44423=CARTESIAN_POINT('Ctrl Pts',(-0.333526626229286,0.626159632205963,
5.37));
#44424=CARTESIAN_POINT('Ctrl Pts',(-0.359788671135902,0.601398372650147,
5.37));
#44425=CARTESIAN_POINT('Ctrl Pts',(-0.367291942238808,0.551875853538513,
5.37));
#44426=CARTESIAN_POINT('Ctrl Pts',(-0.267871871590614,0.65092089176178,
5.4));
#44427=CARTESIAN_POINT('Ctrl Pts',(-0.267871871590614,0.65092089176178,
5.37));
#44428=CARTESIAN_POINT('Ctrl Pts',(-0.307264819741249,0.65092089176178,
5.4));
#44429=CARTESIAN_POINT('Ctrl Pts',(-0.307264819741249,0.65092089176178,
5.37));
#44430=CARTESIAN_POINT('Ctrl Pts',(-0.333526626229286,0.626159632205963,
5.4));
#44431=CARTESIAN_POINT('Ctrl Pts',(-0.333526626229286,0.626159632205963,
5.37));
#44432=CARTESIAN_POINT('',(-0.267871871590614,0.65092089176178,5.4));
#44433=CARTESIAN_POINT('Ctrl Pts',(-0.267871871590614,0.65092089176178,
5.4));
#44434=CARTESIAN_POINT('Ctrl Pts',(-0.307264819741249,0.65092089176178,
5.4));
#44435=CARTESIAN_POINT('Ctrl Pts',(-0.333526626229286,0.626159632205963,
5.4));
#44436=CARTESIAN_POINT('',(-0.267871871590614,0.65092089176178,5.37));
#44437=CARTESIAN_POINT('',(-0.267871871590614,0.65092089176178,5.4));
#44438=CARTESIAN_POINT('Ctrl Pts',(-0.267871871590614,0.65092089176178,
5.37));
#44439=CARTESIAN_POINT('Ctrl Pts',(-0.307264819741249,0.65092089176178,
5.37));
#44440=CARTESIAN_POINT('Ctrl Pts',(-0.333526626229286,0.626159632205963,
5.37));
#44441=CARTESIAN_POINT('Ctrl Pts',(-0.202967420220375,0.626534783840179,
5.4));
#44442=CARTESIAN_POINT('Ctrl Pts',(-0.202967420220375,0.626534783840179,
5.37));
#44443=CARTESIAN_POINT('Ctrl Pts',(-0.228103652596474,0.65092089176178,
5.4));
#44444=CARTESIAN_POINT('Ctrl Pts',(-0.228103652596474,0.65092089176178,
5.37));
#44445=CARTESIAN_POINT('Ctrl Pts',(-0.267871871590614,0.65092089176178,
5.4));
#44446=CARTESIAN_POINT('Ctrl Pts',(-0.267871871590614,0.65092089176178,
5.37));
#44447=CARTESIAN_POINT('',(-0.202967420220375,0.626534783840179,5.4));
#44448=CARTESIAN_POINT('Ctrl Pts',(-0.202967420220375,0.626534783840179,
5.4));
#44449=CARTESIAN_POINT('Ctrl Pts',(-0.228103652596474,0.65092089176178,
5.4));
#44450=CARTESIAN_POINT('Ctrl Pts',(-0.267871871590614,0.65092089176178,
5.4));
#44451=CARTESIAN_POINT('',(-0.202967420220375,0.626534783840179,5.37));
#44452=CARTESIAN_POINT('',(-0.202967420220375,0.626534783840179,5.4));
#44453=CARTESIAN_POINT('Ctrl Pts',(-0.202967420220375,0.626534783840179,
5.37));
#44454=CARTESIAN_POINT('Ctrl Pts',(-0.228103652596474,0.65092089176178,
5.37));
#44455=CARTESIAN_POINT('Ctrl Pts',(-0.267871871590614,0.65092089176178,
5.37));
#44456=CARTESIAN_POINT('Ctrl Pts',(-0.177830949425697,0.565006816387177,
5.4));
#44457=CARTESIAN_POINT('Ctrl Pts',(-0.177830949425697,0.565006816387177,
5.37));
#44458=CARTESIAN_POINT('Ctrl Pts',(-0.177830949425697,0.602148675918579,
5.4));
#44459=CARTESIAN_POINT('Ctrl Pts',(-0.177830949425697,0.602148675918579,
5.37));
#44460=CARTESIAN_POINT('Ctrl Pts',(-0.202967420220375,0.626534783840179,
5.4));
#44461=CARTESIAN_POINT('Ctrl Pts',(-0.202967420220375,0.626534783840179,
5.37));
#44462=CARTESIAN_POINT('',(-0.177830949425697,0.565006816387177,5.4));
#44463=CARTESIAN_POINT('Ctrl Pts',(-0.177830949425697,0.565006816387177,
5.4));
#44464=CARTESIAN_POINT('Ctrl Pts',(-0.177830949425697,0.602148675918579,
5.4));
#44465=CARTESIAN_POINT('Ctrl Pts',(-0.202967420220375,0.626534783840179,
5.4));
#44466=CARTESIAN_POINT('',(-0.177830949425697,0.565006816387177,5.37));
#44467=CARTESIAN_POINT('',(-0.177830949425697,0.565006816387177,5.4));
#44468=CARTESIAN_POINT('Ctrl Pts',(-0.177830949425697,0.565006816387177,
5.37));
#44469=CARTESIAN_POINT('Ctrl Pts',(-0.177830949425697,0.602148675918579,
5.37));
#44470=CARTESIAN_POINT('Ctrl Pts',(-0.202967420220375,0.626534783840179,
5.37));
#44471=CARTESIAN_POINT('Ctrl Pts',(-0.212346568703651,0.495600247383118,
5.4));
#44472=CARTESIAN_POINT('Ctrl Pts',(-0.212346568703651,0.495600247383118,
5.37));
#44473=CARTESIAN_POINT('Ctrl Pts',(-0.177830949425697,0.518110477924347,
5.4));
#44474=CARTESIAN_POINT('Ctrl Pts',(-0.177830949425697,0.518110477924347,
5.37));
#44475=CARTESIAN_POINT('Ctrl Pts',(-0.177830949425697,0.565006816387177,
5.4));
#44476=CARTESIAN_POINT('Ctrl Pts',(-0.177830949425697,0.565006816387177,
5.37));
#44477=CARTESIAN_POINT('',(-0.212346568703651,0.495600247383118,5.4));
#44478=CARTESIAN_POINT('Ctrl Pts',(-0.212346568703651,0.495600247383118,
5.4));
#44479=CARTESIAN_POINT('Ctrl Pts',(-0.177830949425697,0.518110477924347,
5.4));
#44480=CARTESIAN_POINT('Ctrl Pts',(-0.177830949425697,0.565006816387177,
5.4));
#44481=CARTESIAN_POINT('',(-0.212346568703651,0.495600247383118,5.37));
#44482=CARTESIAN_POINT('',(-0.212346568703651,0.495600247383118,5.4));
#44483=CARTESIAN_POINT('Ctrl Pts',(-0.212346568703651,0.495600247383118,
5.37));
#44484=CARTESIAN_POINT('Ctrl Pts',(-0.177830949425697,0.518110477924347,
5.37));
#44485=CARTESIAN_POINT('Ctrl Pts',(-0.177830949425697,0.565006816387177,
5.37));
#44486=CARTESIAN_POINT('Ctrl Pts',(-0.290006890892982,0.473090016841888,
5.4));
#44487=CARTESIAN_POINT('Ctrl Pts',(-0.290006890892982,0.473090016841888,
5.37));
#44488=CARTESIAN_POINT('Ctrl Pts',(-0.246862187981606,0.473090016841888,
5.4));
#44489=CARTESIAN_POINT('Ctrl Pts',(-0.246862187981606,0.473090016841888,
5.37));
#44490=CARTESIAN_POINT('Ctrl Pts',(-0.212346568703651,0.495600247383118,
5.4));
#44491=CARTESIAN_POINT('Ctrl Pts',(-0.212346568703651,0.495600247383118,
5.37));
#44492=CARTESIAN_POINT('',(-0.290006890892982,0.473090016841888,5.4));
#44493=CARTESIAN_POINT('Ctrl Pts',(-0.290006890892982,0.473090016841888,
5.4));
#44494=CARTESIAN_POINT('Ctrl Pts',(-0.246862187981606,0.473090016841888,
5.4));
#44495=CARTESIAN_POINT('Ctrl Pts',(-0.212346568703651,0.495600247383118,
5.4));
#44496=CARTESIAN_POINT('',(-0.290006890892982,0.473090016841888,5.37));
#44497=CARTESIAN_POINT('',(-0.290006890892982,0.473090016841888,5.4));
#44498=CARTESIAN_POINT('Ctrl Pts',(-0.290006890892982,0.473090016841888,
5.37));
#44499=CARTESIAN_POINT('Ctrl Pts',(-0.246862187981606,0.473090016841888,
5.37));
#44500=CARTESIAN_POINT('Ctrl Pts',(-0.212346568703651,0.495600247383118,
5.37));
#44501=CARTESIAN_POINT('Ctrl Pts',(-0.300886884331703,0.473840379714966,
5.4));
#44502=CARTESIAN_POINT('Ctrl Pts',(-0.300886884331703,0.473840379714966,
5.37));
#44503=CARTESIAN_POINT('Ctrl Pts',(-0.294133678078651,0.473090016841888,
5.4));
#44504=CARTESIAN_POINT('Ctrl Pts',(-0.294133678078651,0.473090016841888,
5.37));
#44505=CARTESIAN_POINT('Ctrl Pts',(-0.290006890892982,0.473090016841888,
5.4));
#44506=CARTESIAN_POINT('Ctrl Pts',(-0.290006890892982,0.473090016841888,
5.37));
#44507=CARTESIAN_POINT('',(-0.300886884331703,0.473840379714966,5.4));
#44508=CARTESIAN_POINT('Ctrl Pts',(-0.300886884331703,0.473840379714966,
5.4));
#44509=CARTESIAN_POINT('Ctrl Pts',(-0.294133678078651,0.473090016841888,
5.4));
#44510=CARTESIAN_POINT('Ctrl Pts',(-0.290006890892982,0.473090016841888,
5.4));
#44511=CARTESIAN_POINT('',(-0.300886884331703,0.473840379714966,5.37));
#44512=CARTESIAN_POINT('',(-0.300886884331703,0.473840379714966,5.4));
#44513=CARTESIAN_POINT('Ctrl Pts',(-0.300886884331703,0.473840379714966,
5.37));
#44514=CARTESIAN_POINT('Ctrl Pts',(-0.294133678078651,0.473090016841888,
5.37));
#44515=CARTESIAN_POINT('Ctrl Pts',(-0.290006890892982,0.473090016841888,
5.37));
#44516=CARTESIAN_POINT('Origin',(-0.308390155434609,0.41456344127655,5.4));
#44517=CARTESIAN_POINT('',(-0.308390155434609,0.41456344127655,5.4));
#44518=CARTESIAN_POINT('',(-0.331782471939349,0.229760721720473,5.4));
#44519=CARTESIAN_POINT('',(-0.308390155434609,0.41456344127655,5.37));
#44520=CARTESIAN_POINT('',(-0.308390155434609,0.41456344127655,5.4));
#44521=CARTESIAN_POINT('',(-0.308390155434609,0.41456344127655,5.37));
#44522=CARTESIAN_POINT('Ctrl Pts',(-0.260743632912636,0.422066831588745,
5.4));
#44523=CARTESIAN_POINT('Ctrl Pts',(-0.260743632912636,0.422066831588745,
5.37));
#44524=CARTESIAN_POINT('Ctrl Pts',(-0.279877200722694,0.422066831588745,
5.4));
#44525=CARTESIAN_POINT('Ctrl Pts',(-0.279877200722694,0.422066831588745,
5.37));
#44526=CARTESIAN_POINT('Ctrl Pts',(-0.308390155434608,0.41456344127655,
5.4));
#44527=CARTESIAN_POINT('Ctrl Pts',(-0.308390155434608,0.41456344127655,
5.37));
#44528=CARTESIAN_POINT('',(-0.260743632912636,0.422066831588745,5.4));
#44529=CARTESIAN_POINT('Ctrl Pts',(-0.260743632912636,0.422066831588745,
5.4));
#44530=CARTESIAN_POINT('Ctrl Pts',(-0.279877200722694,0.422066831588745,
5.4));
#44531=CARTESIAN_POINT('Ctrl Pts',(-0.308390155434608,0.41456344127655,
5.4));
#44532=CARTESIAN_POINT('',(-0.260743632912636,0.422066831588745,5.37));
#44533=CARTESIAN_POINT('',(-0.260743632912636,0.422066831588745,5.4));
#44534=CARTESIAN_POINT('Ctrl Pts',(-0.260743632912636,0.422066831588745,
5.37));
#44535=CARTESIAN_POINT('Ctrl Pts',(-0.279877200722694,0.422066831588745,
5.37));
#44536=CARTESIAN_POINT('Ctrl Pts',(-0.308390155434608,0.41456344127655,
5.37));
#44537=CARTESIAN_POINT('Ctrl Pts',(-0.183458343148232,0.391865620017052,
5.4));
#44538=CARTESIAN_POINT('Ctrl Pts',(-0.183458343148232,0.391865620017052,
5.37));
#44539=CARTESIAN_POINT('Ctrl Pts',(-0.213847175240517,0.422066831588745,
5.4));
#44540=CARTESIAN_POINT('Ctrl Pts',(-0.213847175240517,0.422066831588745,
5.37));
#44541=CARTESIAN_POINT('Ctrl Pts',(-0.260743632912636,0.422066831588745,
5.4));
#44542=CARTESIAN_POINT('Ctrl Pts',(-0.260743632912636,0.422066831588745,
5.37));
#44543=CARTESIAN_POINT('',(-0.183458343148232,0.391865620017052,5.4));
#44544=CARTESIAN_POINT('Ctrl Pts',(-0.183458343148232,0.391865620017052,
5.4));
#44545=CARTESIAN_POINT('Ctrl Pts',(-0.213847175240517,0.422066831588745,
5.4));
#44546=CARTESIAN_POINT('Ctrl Pts',(-0.260743632912636,0.422066831588745,
5.4));
#44547=CARTESIAN_POINT('',(-0.183458343148232,0.391865620017052,5.37));
#44548=CARTESIAN_POINT('',(-0.183458343148232,0.391865620017052,5.4));
#44549=CARTESIAN_POINT('Ctrl Pts',(-0.183458343148232,0.391865620017052,
5.37));
#44550=CARTESIAN_POINT('Ctrl Pts',(-0.213847175240517,0.422066831588745,
5.37));
#44551=CARTESIAN_POINT('Ctrl Pts',(-0.260743632912636,0.422066831588745,
5.37));
#44552=CARTESIAN_POINT('Ctrl Pts',(-0.153069511055946,0.315143251419067,
5.4));
#44553=CARTESIAN_POINT('Ctrl Pts',(-0.153069511055946,0.315143251419067,
5.37));
#44554=CARTESIAN_POINT('Ctrl Pts',(-0.153069511055946,0.361664393544197,
5.4));
#44555=CARTESIAN_POINT('Ctrl Pts',(-0.153069511055946,0.361664393544197,
5.37));
#44556=CARTESIAN_POINT('Ctrl Pts',(-0.183458343148232,0.391865620017052,
5.4));
#44557=CARTESIAN_POINT('Ctrl Pts',(-0.183458343148232,0.391865620017052,
5.37));
#44558=CARTESIAN_POINT('',(-0.153069511055946,0.315143251419067,5.4));
#44559=CARTESIAN_POINT('Ctrl Pts',(-0.153069511055946,0.315143251419067,
5.4));
#44560=CARTESIAN_POINT('Ctrl Pts',(-0.153069511055946,0.361664393544197,
5.4));
#44561=CARTESIAN_POINT('Ctrl Pts',(-0.183458343148232,0.391865620017052,
5.4));
#44562=CARTESIAN_POINT('',(-0.153069511055946,0.315143251419067,5.37));
#44563=CARTESIAN_POINT('',(-0.153069511055946,0.315143251419067,5.4));
#44564=CARTESIAN_POINT('Ctrl Pts',(-0.153069511055946,0.315143251419067,
5.37));
#44565=CARTESIAN_POINT('Ctrl Pts',(-0.153069511055946,0.361664393544197,
5.37));
#44566=CARTESIAN_POINT('Ctrl Pts',(-0.183458343148232,0.391865620017052,
5.37));
#44567=CARTESIAN_POINT('Ctrl Pts',(-0.185897126793861,0.233356082439423,
5.4));
#44568=CARTESIAN_POINT('Ctrl Pts',(-0.185897126793861,0.233356082439423,
5.37));
#44569=CARTESIAN_POINT('Ctrl Pts',(-0.153069511055946,0.266371095180511,
5.4));
#44570=CARTESIAN_POINT('Ctrl Pts',(-0.153069511055946,0.266371095180511,
5.37));
#44571=CARTESIAN_POINT('Ctrl Pts',(-0.153069511055946,0.315143251419067,
5.4));
#44572=CARTESIAN_POINT('Ctrl Pts',(-0.153069511055946,0.315143251419067,
5.37));
#44573=CARTESIAN_POINT('',(-0.185897126793861,0.233356082439423,5.4));
#44574=CARTESIAN_POINT('Ctrl Pts',(-0.185897126793861,0.233356082439423,
5.4));
#44575=CARTESIAN_POINT('Ctrl Pts',(-0.153069511055946,0.266371095180511,
5.4));
#44576=CARTESIAN_POINT('Ctrl Pts',(-0.153069511055946,0.315143251419067,
5.4));
#44577=CARTESIAN_POINT('',(-0.185897126793861,0.233356082439423,5.37));
#44578=CARTESIAN_POINT('',(-0.185897126793861,0.233356082439423,5.4));
#44579=CARTESIAN_POINT('Ctrl Pts',(-0.185897126793861,0.233356082439423,
5.37));
#44580=CARTESIAN_POINT('Ctrl Pts',(-0.153069511055946,0.266371095180511,
5.37));
#44581=CARTESIAN_POINT('Ctrl Pts',(-0.153069511055946,0.315143251419067,
5.37));
#44582=CARTESIAN_POINT('Ctrl Pts',(-0.26637102663517,0.200341069698334,
5.4));
#44583=CARTESIAN_POINT('Ctrl Pts',(-0.26637102663517,0.200341069698334,
5.37));
#44584=CARTESIAN_POINT('Ctrl Pts',(-0.218724504113197,0.200341069698334,
5.4));
#44585=CARTESIAN_POINT('Ctrl Pts',(-0.218724504113197,0.200341069698334,
5.37));
#44586=CARTESIAN_POINT('Ctrl Pts',(-0.185897126793861,0.233356082439423,
5.4));
#44587=CARTESIAN_POINT('Ctrl Pts',(-0.185897126793861,0.233356082439423,
5.37));
#44588=CARTESIAN_POINT('',(-0.26637102663517,0.200341069698334,5.4));
#44589=CARTESIAN_POINT('Ctrl Pts',(-0.26637102663517,0.200341069698334,
5.4));
#44590=CARTESIAN_POINT('Ctrl Pts',(-0.218724504113197,0.200341069698334,
5.4));
#44591=CARTESIAN_POINT('Ctrl Pts',(-0.185897126793861,0.233356082439423,
5.4));
#44592=CARTESIAN_POINT('',(-0.26637102663517,0.200341069698334,5.37));
#44593=CARTESIAN_POINT('',(-0.26637102663517,0.200341069698334,5.4));
#44594=CARTESIAN_POINT('Ctrl Pts',(-0.26637102663517,0.200341069698334,
5.37));
#44595=CARTESIAN_POINT('Ctrl Pts',(-0.218724504113197,0.200341069698334,
5.37));
#44596=CARTESIAN_POINT('Ctrl Pts',(-0.185897126793861,0.233356082439423,
5.37));
#44597=CARTESIAN_POINT('Ctrl Pts',(-0.334464564919472,0.225665086507797,
5.4));
#44598=CARTESIAN_POINT('Ctrl Pts',(-0.334464564919472,0.225665086507797,
5.37));
#44599=CARTESIAN_POINT('Ctrl Pts',(-0.306514278054237,0.200341069698334,
5.4));
#44600=CARTESIAN_POINT('Ctrl Pts',(-0.306514278054237,0.200341069698334,
5.37));
#44601=CARTESIAN_POINT('Ctrl Pts',(-0.26637102663517,0.200341069698334,
5.4));
#44602=CARTESIAN_POINT('Ctrl Pts',(-0.26637102663517,0.200341069698334,
5.37));
#44603=CARTESIAN_POINT('',(-0.334464564919472,0.225665086507797,5.4));
#44604=CARTESIAN_POINT('Ctrl Pts',(-0.334464564919472,0.225665086507797,
5.4));
#44605=CARTESIAN_POINT('Ctrl Pts',(-0.306514278054237,0.200341069698334,
5.4));
#44606=CARTESIAN_POINT('Ctrl Pts',(-0.26637102663517,0.200341069698334,
5.4));
#44607=CARTESIAN_POINT('',(-0.334464564919472,0.225665086507797,5.37));
#44608=CARTESIAN_POINT('',(-0.334464564919472,0.225665086507797,5.4));
#44609=CARTESIAN_POINT('Ctrl Pts',(-0.334464564919472,0.225665086507797,
5.37));
#44610=CARTESIAN_POINT('Ctrl Pts',(-0.306514278054237,0.200341069698334,
5.37));
#44611=CARTESIAN_POINT('Ctrl Pts',(-0.26637102663517,0.200341069698334,
5.37));
#44612=CARTESIAN_POINT('Ctrl Pts',(-0.374045148491859,0.308390179276466,
5.4));
#44613=CARTESIAN_POINT('Ctrl Pts',(-0.374045148491859,0.308390179276466,
5.37));
#44614=CARTESIAN_POINT('Ctrl Pts',(-0.362414851784706,0.250989103317261,
5.4));
#44615=CARTESIAN_POINT('Ctrl Pts',(-0.362414851784706,0.250989103317261,
5.37));
#44616=CARTESIAN_POINT('Ctrl Pts',(-0.334464564919472,0.225665086507797,
5.4));
#44617=CARTESIAN_POINT('Ctrl Pts',(-0.334464564919472,0.225665086507797,
5.37));
#44618=CARTESIAN_POINT('',(-0.374045148491859,0.308390179276466,5.4));
#44619=CARTESIAN_POINT('Ctrl Pts',(-0.374045148491859,0.308390179276466,
5.4));
#44620=CARTESIAN_POINT('Ctrl Pts',(-0.362414851784706,0.250989103317261,
5.4));
#44621=CARTESIAN_POINT('Ctrl Pts',(-0.334464564919472,0.225665086507797,
5.4));
#44622=CARTESIAN_POINT('',(-0.374045148491859,0.308390179276466,5.37));
#44623=CARTESIAN_POINT('',(-0.374045148491859,0.308390179276466,5.4));
#44624=CARTESIAN_POINT('Ctrl Pts',(-0.374045148491859,0.308390179276466,
5.37));
#44625=CARTESIAN_POINT('Ctrl Pts',(-0.362414851784706,0.250989103317261,
5.37));
#44626=CARTESIAN_POINT('Ctrl Pts',(-0.334464564919472,0.225665086507797,
5.37));
#44627=CARTESIAN_POINT('Origin',(-0.441575780510902,0.299386093020439,5.4));
#44628=CARTESIAN_POINT('',(-0.441575780510902,0.299386093020439,5.4));
#44629=CARTESIAN_POINT('',(-0.244254895913005,0.325695550105545,5.4));
#44630=CARTESIAN_POINT('',(-0.441575780510902,0.299386093020439,5.37));
#44631=CARTESIAN_POINT('',(-0.441575780510902,0.299386093020439,5.4));
#44632=CARTESIAN_POINT('',(-0.441575780510902,0.299386093020439,5.37));
#44633=CARTESIAN_POINT('Ctrl Pts',(-0.386988416314125,0.187585258483887,
5.4));
#44634=CARTESIAN_POINT('Ctrl Pts',(-0.386988416314125,0.187585258483887,
5.37));
#44635=CARTESIAN_POINT('Ctrl Pts',(-0.43482281267643,0.230729871988297,
5.4));
#44636=CARTESIAN_POINT('Ctrl Pts',(-0.43482281267643,0.230729871988297,
5.37));
#44637=CARTESIAN_POINT('Ctrl Pts',(-0.441575780510902,0.299386093020439,
5.4));
#44638=CARTESIAN_POINT('Ctrl Pts',(-0.441575780510902,0.299386093020439,
5.37));
#44639=CARTESIAN_POINT('',(-0.386988416314125,0.187585258483887,5.4));
#44640=CARTESIAN_POINT('Ctrl Pts',(-0.386988416314125,0.187585258483887,
5.4));
#44641=CARTESIAN_POINT('Ctrl Pts',(-0.43482281267643,0.230729871988297,
5.4));
#44642=CARTESIAN_POINT('Ctrl Pts',(-0.441575780510902,0.299386093020439,
5.4));
#44643=CARTESIAN_POINT('',(-0.386988416314125,0.187585258483887,5.37));
#44644=CARTESIAN_POINT('',(-0.386988416314125,0.187585258483887,5.4));
#44645=CARTESIAN_POINT('Ctrl Pts',(-0.386988416314125,0.187585258483887,
5.37));
#44646=CARTESIAN_POINT('Ctrl Pts',(-0.43482281267643,0.230729871988297,
5.37));
#44647=CARTESIAN_POINT('Ctrl Pts',(-0.441575780510902,0.299386093020439,
5.37));
#44648=CARTESIAN_POINT('Ctrl Pts',(-0.266746297478676,0.144440674781799,
5.4));
#44649=CARTESIAN_POINT('Ctrl Pts',(-0.266746297478676,0.144440674781799,
5.37));
#44650=CARTESIAN_POINT('Ctrl Pts',(-0.339154258370399,0.144440674781799,
5.4));
#44651=CARTESIAN_POINT('Ctrl Pts',(-0.339154258370399,0.144440674781799,
5.37));
#44652=CARTESIAN_POINT('Ctrl Pts',(-0.386988416314125,0.187585258483887,
5.4));
#44653=CARTESIAN_POINT('Ctrl Pts',(-0.386988416314125,0.187585258483887,
5.37));
#44654=CARTESIAN_POINT('Ctrl Pts',(-0.266746297478676,0.144440674781799,
5.4));
#44655=CARTESIAN_POINT('Ctrl Pts',(-0.339154258370399,0.144440674781799,
5.4));
#44656=CARTESIAN_POINT('Ctrl Pts',(-0.386988416314125,0.187585258483887,
5.4));
#44657=CARTESIAN_POINT('Ctrl Pts',(-0.266746297478676,0.144440674781799,
5.37));
#44658=CARTESIAN_POINT('Ctrl Pts',(-0.339154258370399,0.144440674781799,
5.37));
#44659=CARTESIAN_POINT('Ctrl Pts',(-0.386988416314125,0.187585258483887,
5.37));
#44660=CARTESIAN_POINT('Origin',(-0.261493936181068,0.425443404912949,5.37));
#44661=CARTESIAN_POINT('Origin',(-1.13264001905918,0.387176015973091,5.4));
#44662=CARTESIAN_POINT('',(-1.13264001905918,0.387176015973091,5.4));
#44663=CARTESIAN_POINT('',(-0.925170674920082,0.387176015973091,5.4));
#44664=CARTESIAN_POINT('',(-0.566320009529591,0.387176015973091,5.4));
#44665=CARTESIAN_POINT('',(-1.13264001905918,0.387176015973091,5.37));
#44666=CARTESIAN_POINT('',(-1.13264001905918,0.387176015973091,5.4));
#44667=CARTESIAN_POINT('',(-0.925170674920082,0.387176015973091,5.37));
#44668=CARTESIAN_POINT('',(-1.13264001905918,0.387176015973091,5.37));
#44669=CARTESIAN_POINT('',(-0.925170674920082,0.387176015973091,5.4));
#44670=CARTESIAN_POINT('Origin',(-1.13264001905918,0.319270142912865,5.4));
#44671=CARTESIAN_POINT('',(-1.13264001905918,0.319270142912865,5.4));
#44672=CARTESIAN_POINT('',(-1.13264001905918,0.159635071456432,5.4));
#44673=CARTESIAN_POINT('',(-1.13264001905918,0.319270142912865,5.37));
#44674=CARTESIAN_POINT('',(-1.13264001905918,0.319270142912865,5.4));
#44675=CARTESIAN_POINT('',(-1.13264001905918,0.319270142912865,5.37));
#44676=CARTESIAN_POINT('Origin',(-0.925170674920082,0.319270142912865,5.4));
#44677=CARTESIAN_POINT('',(-0.925170674920082,0.319270142912865,5.4));
#44678=CARTESIAN_POINT('',(-0.462585337460041,0.319270142912865,5.4));
#44679=CARTESIAN_POINT('',(-0.925170674920082,0.319270142912865,5.37));
#44680=CARTESIAN_POINT('',(-0.925170674920082,0.319270142912865,5.4));
#44681=CARTESIAN_POINT('',(-0.925170674920082,0.319270142912865,5.37));
#44682=CARTESIAN_POINT('Origin',(-0.925170674920082,0.387176015973091,5.4));
#44683=CARTESIAN_POINT('',(-0.925170674920082,0.193588007986546,5.4));
#44684=CARTESIAN_POINT('',(-0.925170674920082,0.387176015973091,5.37));
#44685=CARTESIAN_POINT('Origin',(-1.02890534698963,0.353223079442978,5.37));
#44686=CARTESIAN_POINT('Ctrl Pts',(-1.93437947332859,0.646418863534927,
5.4));
#44687=CARTESIAN_POINT('Ctrl Pts',(-1.93437947332859,0.646418863534927,
5.37));
#44688=CARTESIAN_POINT('Ctrl Pts',(-1.94488431513309,0.593519800901413,
5.4));
#44689=CARTESIAN_POINT('Ctrl Pts',(-1.94488431513309,0.593519800901413,
5.37));
#44690=CARTESIAN_POINT('Ctrl Pts',(-1.96401788294315,0.541371101140976,
5.4));
#44691=CARTESIAN_POINT('Ctrl Pts',(-1.96401788294315,0.541371101140976,
5.37));
#44692=CARTESIAN_POINT('',(-1.93437947332859,0.646418863534927,5.4));
#44693=CARTESIAN_POINT('',(-1.96401788294315,0.541371101140976,5.4));
#44694=CARTESIAN_POINT('Ctrl Pts',(-1.93437947332859,0.646418863534927,
5.4));
#44695=CARTESIAN_POINT('Ctrl Pts',(-1.94488431513309,0.593519800901413,
5.4));
#44696=CARTESIAN_POINT('Ctrl Pts',(-1.96401788294315,0.541371101140976,
5.4));
#44697=CARTESIAN_POINT('',(-1.93437947332859,0.646418863534927,5.37));
#44698=CARTESIAN_POINT('',(-1.93437947332859,0.646418863534927,5.4));
#44699=CARTESIAN_POINT('',(-1.96401788294315,0.541371101140976,5.37));
#44700=CARTESIAN_POINT('Ctrl Pts',(-1.93437947332859,0.646418863534927,
5.37));
#44701=CARTESIAN_POINT('Ctrl Pts',(-1.94488431513309,0.593519800901413,
5.37));
#44702=CARTESIAN_POINT('Ctrl Pts',(-1.96401788294315,0.541371101140976,
5.37));
#44703=CARTESIAN_POINT('',(-1.96401788294315,0.541371101140976,5.4));
#44704=CARTESIAN_POINT('Ctrl Pts',(-1.89536167681217,0.532367014884949,
5.4));
#44705=CARTESIAN_POINT('Ctrl Pts',(-1.89536167681217,0.532367014884949,
5.37));
#44706=CARTESIAN_POINT('Ctrl Pts',(-1.92162372171879,0.601773554086685,
5.4));
#44707=CARTESIAN_POINT('Ctrl Pts',(-1.92162372171879,0.601773554086685,
5.37));
#44708=CARTESIAN_POINT('Ctrl Pts',(-1.93437947332859,0.646418863534927,
5.4));
#44709=CARTESIAN_POINT('Ctrl Pts',(-1.93437947332859,0.646418863534927,
5.37));
#44710=CARTESIAN_POINT('',(-1.89536167681217,0.532367014884949,5.4));
#44711=CARTESIAN_POINT('Ctrl Pts',(-1.89536167681217,0.532367014884949,
5.4));
#44712=CARTESIAN_POINT('Ctrl Pts',(-1.92162372171879,0.601773554086685,
5.4));
#44713=CARTESIAN_POINT('Ctrl Pts',(-1.93437947332859,0.646418863534927,
5.4));
#44714=CARTESIAN_POINT('',(-1.89536167681217,0.532367014884949,5.37));
#44715=CARTESIAN_POINT('',(-1.89536167681217,0.532367014884949,5.4));
#44716=CARTESIAN_POINT('Ctrl Pts',(-1.89536167681217,0.532367014884949,
5.37));
#44717=CARTESIAN_POINT('Ctrl Pts',(-1.92162372171879,0.601773554086685,
5.37));
#44718=CARTESIAN_POINT('Ctrl Pts',(-1.93437947332859,0.646418863534927,
5.37));
#44719=CARTESIAN_POINT('Origin',(-1.83796061575413,0.380047762393951,5.4));
#44720=CARTESIAN_POINT('',(-1.83796061575413,0.380047762393951,5.4));
#44721=CARTESIAN_POINT('',(-1.66097698357881,-0.089595377631381,5.4));
#44722=CARTESIAN_POINT('',(-1.83796061575413,0.380047762393951,5.37));
#44723=CARTESIAN_POINT('',(-1.83796061575413,0.380047762393951,5.4));
#44724=CARTESIAN_POINT('',(-1.83796061575413,0.380047762393951,5.37));
#44725=CARTESIAN_POINT('Origin',(-2.02442039549351,0.380047762393951,5.4));
#44726=CARTESIAN_POINT('',(-2.02442039549351,0.380047762393951,5.4));
#44727=CARTESIAN_POINT('',(-1.01221019774675,0.380047762393951,5.4));
#44728=CARTESIAN_POINT('',(-2.02442039549351,0.380047762393951,5.37));
#44729=CARTESIAN_POINT('',(-2.02442039549351,0.380047762393951,5.4));
#44730=CARTESIAN_POINT('',(-2.02442039549351,0.380047762393951,5.37));
#44731=CARTESIAN_POINT('Origin',(-1.96401788294315,0.541371101140976,5.4));
#44732=CARTESIAN_POINT('',(-1.93216564827672,0.626442212026634,5.4));
#44733=CARTESIAN_POINT('',(-1.96401788294315,0.541371101140976,5.37));
#44734=CARTESIAN_POINT('Origin',(-1.81545044481754,0.320770823955536,5.4));
#44735=CARTESIAN_POINT('',(-1.81545044481754,0.320770823955536,5.4));
#44736=CARTESIAN_POINT('',(-2.04542995989323,0.320770823955536,5.4));
#44737=CARTESIAN_POINT('',(-0.907725222408772,0.320770823955536,5.4));
#44738=CARTESIAN_POINT('',(-1.81545044481754,0.320770823955536,5.37));
#44739=CARTESIAN_POINT('',(-1.81545044481754,0.320770823955536,5.4));
#44740=CARTESIAN_POINT('',(-2.04542995989323,0.320770823955536,5.37));
#44741=CARTESIAN_POINT('',(-1.81545044481754,0.320770823955536,5.37));
#44742=CARTESIAN_POINT('',(-2.04542995989323,0.320770823955536,5.4));
#44743=CARTESIAN_POINT('Origin',(-1.75129629671574,0.154195094108582,5.4));
#44744=CARTESIAN_POINT('',(-1.75129629671574,0.154195094108582,5.4));
#44745=CARTESIAN_POINT('',(-1.61233179129081,-0.206625127169145,5.4));
#44746=CARTESIAN_POINT('',(-1.75129629671574,0.154195094108582,5.37));
#44747=CARTESIAN_POINT('',(-1.75129629671574,0.154195094108582,5.4));
#44748=CARTESIAN_POINT('',(-1.75129629671574,0.154195094108582,5.37));
#44749=CARTESIAN_POINT('Origin',(-1.6683836132288,0.154195094108582,5.4));
#44750=CARTESIAN_POINT('',(-1.6683836132288,0.154195094108582,5.4));
#44751=CARTESIAN_POINT('',(-0.834191806614399,0.154195094108582,5.4));
#44752=CARTESIAN_POINT('',(-1.6683836132288,0.154195094108582,5.37));
#44753=CARTESIAN_POINT('',(-1.6683836132288,0.154195094108582,5.4));
#44754=CARTESIAN_POINT('',(-1.6683836132288,0.154195094108582,5.37));
#44755=CARTESIAN_POINT('Origin',(-1.89348591864109,0.704195106029511,5.4));
#44756=CARTESIAN_POINT('',(-1.89348591864109,0.704195106029511,5.4));
#44757=CARTESIAN_POINT('',(-1.63422248259755,0.0707280579980082,5.4));
#44758=CARTESIAN_POINT('',(-1.89348591864109,0.704195106029511,5.37));
#44759=CARTESIAN_POINT('',(-1.89348591864109,0.704195106029511,5.4));
#44760=CARTESIAN_POINT('',(-1.89348591864109,0.704195106029511,5.37));
#44761=CARTESIAN_POINT('Origin',(-1.97189654409885,0.704195106029511,5.4));
#44762=CARTESIAN_POINT('',(-1.97189654409885,0.704195106029511,5.4));
#44763=CARTESIAN_POINT('',(-0.985948272049427,0.704195106029511,5.4));
#44764=CARTESIAN_POINT('',(-1.97189654409885,0.704195106029511,5.37));
#44765=CARTESIAN_POINT('',(-1.97189654409885,0.704195106029511,5.4));
#44766=CARTESIAN_POINT('',(-1.97189654409885,0.704195106029511,5.37));
#44767=CARTESIAN_POINT('Origin',(-2.18311752378941,0.154195094108582,5.4));
#44768=CARTESIAN_POINT('',(-2.18311752378941,0.154195094108582,5.4));
#44769=CARTESIAN_POINT('',(-2.06862327822368,0.452327583212093,5.4));
#44770=CARTESIAN_POINT('',(-2.18311752378941,0.154195094108582,5.37));
#44771=CARTESIAN_POINT('',(-2.18311752378941,0.154195094108582,5.4));
#44772=CARTESIAN_POINT('',(-2.18311752378941,0.154195094108582,5.37));
#44773=CARTESIAN_POINT('Origin',(-2.10583241283894,0.154195094108582,5.4));
#44774=CARTESIAN_POINT('',(-2.10583241283894,0.154195094108582,5.4));
#44775=CARTESIAN_POINT('',(-1.05291620641947,0.154195094108582,5.4));
#44776=CARTESIAN_POINT('',(-2.10583241283894,0.154195094108582,5.37));
#44777=CARTESIAN_POINT('',(-2.10583241283894,0.154195094108582,5.4));
#44778=CARTESIAN_POINT('',(-2.10583241283894,0.154195094108582,5.37));
#44779=CARTESIAN_POINT('Origin',(-2.04542995989323,0.320770823955536,5.4));
#44780=CARTESIAN_POINT('',(-1.97798173193314,0.506777140775716,5.4));
#44781=CARTESIAN_POINT('',(-2.04542995989323,0.320770823955536,5.37));
#44782=CARTESIAN_POINT('Origin',(-1.9257505685091,0.429195100069046,5.37));
#44783=CARTESIAN_POINT('Ctrl Pts',(-1.40051163733006,0.144815826416016,
5.4));
#44784=CARTESIAN_POINT('Ctrl Pts',(-1.40051163733006,0.144815826416016,
5.37));
#44785=CARTESIAN_POINT('Ctrl Pts',(-1.47517050802708,0.144815826416016,
5.4));
#44786=CARTESIAN_POINT('Ctrl Pts',(-1.47517050802708,0.144815826416016,
5.37));
#44787=CARTESIAN_POINT('Ctrl Pts',(-1.5256309658289,0.16657572388649,5.4));
#44788=CARTESIAN_POINT('Ctrl Pts',(-1.5256309658289,0.16657572388649,5.37));
#44789=CARTESIAN_POINT('',(-1.40051163733006,0.144815826416016,5.4));
#44790=CARTESIAN_POINT('',(-1.5256309658289,0.16657572388649,5.4));
#44791=CARTESIAN_POINT('Ctrl Pts',(-1.40051163733006,0.144815826416016,
5.4));
#44792=CARTESIAN_POINT('Ctrl Pts',(-1.47517050802708,0.144815826416016,
5.4));
#44793=CARTESIAN_POINT('Ctrl Pts',(-1.5256309658289,0.16657572388649,5.4));
#44794=CARTESIAN_POINT('',(-1.40051163733006,0.144815826416016,5.37));
#44795=CARTESIAN_POINT('',(-1.40051163733006,0.144815826416016,5.4));
#44796=CARTESIAN_POINT('',(-1.5256309658289,0.16657572388649,5.37));
#44797=CARTESIAN_POINT('Ctrl Pts',(-1.40051163733006,0.144815826416016,
5.37));
#44798=CARTESIAN_POINT('Ctrl Pts',(-1.47517050802708,0.144815826416016,
5.37));
#44799=CARTESIAN_POINT('Ctrl Pts',(-1.5256309658289,0.16657572388649,5.37));
#44800=CARTESIAN_POINT('',(-1.5256309658289,0.16657572388649,5.4));
#44801=CARTESIAN_POINT('Ctrl Pts',(-1.29452587664127,0.166388148069382,
5.4));
#44802=CARTESIAN_POINT('Ctrl Pts',(-1.29452587664127,0.166388148069382,
5.37));
#44803=CARTESIAN_POINT('Ctrl Pts',(-1.34160985052586,0.144815826416016,
5.4));
#44804=CARTESIAN_POINT('Ctrl Pts',(-1.34160985052586,0.144815826416016,
5.37));
#44805=CARTESIAN_POINT('Ctrl Pts',(-1.40051163733006,0.144815826416016,
5.4));
#44806=CARTESIAN_POINT('Ctrl Pts',(-1.40051163733006,0.144815826416016,
5.37));
#44807=CARTESIAN_POINT('',(-1.29452587664127,0.166388148069382,5.4));
#44808=CARTESIAN_POINT('Ctrl Pts',(-1.29452587664127,0.166388148069382,
5.4));
#44809=CARTESIAN_POINT('Ctrl Pts',(-1.34160985052586,0.144815826416016,
5.4));
#44810=CARTESIAN_POINT('Ctrl Pts',(-1.40051163733006,0.144815826416016,
5.4));
#44811=CARTESIAN_POINT('',(-1.29452587664127,0.166388148069382,5.37));
#44812=CARTESIAN_POINT('',(-1.29452587664127,0.166388148069382,5.4));
#44813=CARTESIAN_POINT('Ctrl Pts',(-1.29452587664127,0.166388148069382,
5.37));
#44814=CARTESIAN_POINT('Ctrl Pts',(-1.34160985052586,0.144815826416016,
5.37));
#44815=CARTESIAN_POINT('Ctrl Pts',(-1.40051163733006,0.144815826416016,
5.37));
#44816=CARTESIAN_POINT('Ctrl Pts',(-1.2223055511713,0.226790601015091,5.4));
#44817=CARTESIAN_POINT('Ctrl Pts',(-1.2223055511713,0.226790601015091,5.37));
#44818=CARTESIAN_POINT('Ctrl Pts',(-1.24744202196598,0.187960439920425,
5.4));
#44819=CARTESIAN_POINT('Ctrl Pts',(-1.24744202196598,0.187960439920425,
5.37));
#44820=CARTESIAN_POINT('Ctrl Pts',(-1.29452587664127,0.166388148069382,
5.4));
#44821=CARTESIAN_POINT('Ctrl Pts',(-1.29452587664127,0.166388148069382,
5.37));
#44822=CARTESIAN_POINT('',(-1.2223055511713,0.226790601015091,5.4));
#44823=CARTESIAN_POINT('Ctrl Pts',(-1.2223055511713,0.226790601015091,5.4));
#44824=CARTESIAN_POINT('Ctrl Pts',(-1.24744202196598,0.187960439920425,
5.4));
#44825=CARTESIAN_POINT('Ctrl Pts',(-1.29452587664127,0.166388148069382,
5.4));
#44826=CARTESIAN_POINT('',(-1.2223055511713,0.226790601015091,5.37));
#44827=CARTESIAN_POINT('',(-1.2223055511713,0.226790601015091,5.4));
#44828=CARTESIAN_POINT('Ctrl Pts',(-1.2223055511713,0.226790601015091,5.37));
#44829=CARTESIAN_POINT('Ctrl Pts',(-1.24744202196598,0.187960439920425,
5.37));
#44830=CARTESIAN_POINT('Ctrl Pts',(-1.29452587664127,0.166388148069382,
5.37));
#44831=CARTESIAN_POINT('Ctrl Pts',(-1.19716919958591,0.30951569378376,5.4));
#44832=CARTESIAN_POINT('Ctrl Pts',(-1.19716919958591,0.30951569378376,5.37));
#44833=CARTESIAN_POINT('Ctrl Pts',(-1.19716919958591,0.265620732307434,
5.4));
#44834=CARTESIAN_POINT('Ctrl Pts',(-1.19716919958591,0.265620732307434,
5.37));
#44835=CARTESIAN_POINT('Ctrl Pts',(-1.2223055511713,0.226790601015091,5.4));
#44836=CARTESIAN_POINT('Ctrl Pts',(-1.2223055511713,0.226790601015091,5.37));
#44837=CARTESIAN_POINT('',(-1.19716919958591,0.30951569378376,5.4));
#44838=CARTESIAN_POINT('Ctrl Pts',(-1.19716919958591,0.30951569378376,5.4));
#44839=CARTESIAN_POINT('Ctrl Pts',(-1.19716919958591,0.265620732307434,
5.4));
#44840=CARTESIAN_POINT('Ctrl Pts',(-1.2223055511713,0.226790601015091,5.4));
#44841=CARTESIAN_POINT('',(-1.19716919958591,0.30951569378376,5.37));
#44842=CARTESIAN_POINT('',(-1.19716919958591,0.30951569378376,5.4));
#44843=CARTESIAN_POINT('Ctrl Pts',(-1.19716919958591,0.30951569378376,5.37));
#44844=CARTESIAN_POINT('Ctrl Pts',(-1.19716919958591,0.265620732307434,
5.37));
#44845=CARTESIAN_POINT('Ctrl Pts',(-1.2223055511713,0.226790601015091,5.37));
#44846=CARTESIAN_POINT('Ctrl Pts',(-1.220054641366,0.387738758325577,5.4));
#44847=CARTESIAN_POINT('Ctrl Pts',(-1.220054641366,0.387738758325577,5.37));
#44848=CARTESIAN_POINT('Ctrl Pts',(-1.19716919958591,0.353785821795464,
5.4));
#44849=CARTESIAN_POINT('Ctrl Pts',(-1.19716919958591,0.353785821795464,
5.37));
#44850=CARTESIAN_POINT('Ctrl Pts',(-1.19716919958591,0.30951569378376,5.4));
#44851=CARTESIAN_POINT('Ctrl Pts',(-1.19716919958591,0.30951569378376,5.37));
#44852=CARTESIAN_POINT('',(-1.220054641366,0.387738758325577,5.4));
#44853=CARTESIAN_POINT('Ctrl Pts',(-1.220054641366,0.387738758325577,5.4));
#44854=CARTESIAN_POINT('Ctrl Pts',(-1.19716919958591,0.353785821795464,
5.4));
#44855=CARTESIAN_POINT('Ctrl Pts',(-1.19716919958591,0.30951569378376,5.4));
#44856=CARTESIAN_POINT('',(-1.220054641366,0.387738758325577,5.37));
#44857=CARTESIAN_POINT('',(-1.220054641366,0.387738758325577,5.4));
#44858=CARTESIAN_POINT('Ctrl Pts',(-1.220054641366,0.387738758325577,5.37));
#44859=CARTESIAN_POINT('Ctrl Pts',(-1.19716919958591,0.353785821795464,
5.37));
#44860=CARTESIAN_POINT('Ctrl Pts',(-1.19716919958591,0.30951569378376,5.37));
#44861=CARTESIAN_POINT('Ctrl Pts',(-1.29096175730228,0.443826758861542,
5.4));
#44862=CARTESIAN_POINT('Ctrl Pts',(-1.29096175730228,0.443826758861542,
5.37));
#44863=CARTESIAN_POINT('Ctrl Pts',(-1.24293996393681,0.421691679954529,
5.4));
#44864=CARTESIAN_POINT('Ctrl Pts',(-1.24293996393681,0.421691679954529,
5.37));
#44865=CARTESIAN_POINT('Ctrl Pts',(-1.220054641366,0.387738758325577,5.4));
#44866=CARTESIAN_POINT('Ctrl Pts',(-1.220054641366,0.387738758325577,5.37));
#44867=CARTESIAN_POINT('',(-1.29096175730228,0.443826758861542,5.4));
#44868=CARTESIAN_POINT('Ctrl Pts',(-1.29096175730228,0.443826758861542,
5.4));
#44869=CARTESIAN_POINT('Ctrl Pts',(-1.24293996393681,0.421691679954529,
5.4));
#44870=CARTESIAN_POINT('Ctrl Pts',(-1.220054641366,0.387738758325577,5.4));
#44871=CARTESIAN_POINT('',(-1.29096175730228,0.443826758861542,5.37));
#44872=CARTESIAN_POINT('',(-1.29096175730228,0.443826758861542,5.4));
#44873=CARTESIAN_POINT('Ctrl Pts',(-1.29096175730228,0.443826758861542,
5.37));
#44874=CARTESIAN_POINT('Ctrl Pts',(-1.24293996393681,0.421691679954529,
5.37));
#44875=CARTESIAN_POINT('Ctrl Pts',(-1.220054641366,0.387738758325577,5.37));
#44876=CARTESIAN_POINT('Ctrl Pts',(-1.41270472109318,0.478905194997787,
5.4));
#44877=CARTESIAN_POINT('Ctrl Pts',(-1.41270472109318,0.478905194997787,
5.37));
#44878=CARTESIAN_POINT('Ctrl Pts',(-1.32397677004337,0.458833569288254,
5.4));
#44879=CARTESIAN_POINT('Ctrl Pts',(-1.32397677004337,0.458833569288254,
5.37));
#44880=CARTESIAN_POINT('Ctrl Pts',(-1.29096175730228,0.443826758861542,
5.4));
#44881=CARTESIAN_POINT('Ctrl Pts',(-1.29096175730228,0.443826758861542,
5.37));
#44882=CARTESIAN_POINT('',(-1.41270472109318,0.478905194997787,5.4));
#44883=CARTESIAN_POINT('Ctrl Pts',(-1.41270472109318,0.478905194997787,
5.4));
#44884=CARTESIAN_POINT('Ctrl Pts',(-1.32397677004337,0.458833569288254,
5.4));
#44885=CARTESIAN_POINT('Ctrl Pts',(-1.29096175730228,0.443826758861542,
5.4));
#44886=CARTESIAN_POINT('',(-1.41270472109318,0.478905194997787,5.37));
#44887=CARTESIAN_POINT('',(-1.41270472109318,0.478905194997787,5.4));
#44888=CARTESIAN_POINT('Ctrl Pts',(-1.41270472109318,0.478905194997787,
5.37));
#44889=CARTESIAN_POINT('Ctrl Pts',(-1.32397677004337,0.458833569288254,
5.37));
#44890=CARTESIAN_POINT('Ctrl Pts',(-1.29096175730228,0.443826758861542,
5.37));
#44891=CARTESIAN_POINT('Ctrl Pts',(-1.52244199812412,0.518110537528992,
5.4));
#44892=CARTESIAN_POINT('Ctrl Pts',(-1.52244199812412,0.518110537528992,
5.37));
#44893=CARTESIAN_POINT('Ctrl Pts',(-1.5014324337244,0.498976820707321,5.4));
#44894=CARTESIAN_POINT('Ctrl Pts',(-1.5014324337244,0.498976820707321,5.37));
#44895=CARTESIAN_POINT('Ctrl Pts',(-1.41270472109318,0.478905194997787,
5.4));
#44896=CARTESIAN_POINT('Ctrl Pts',(-1.41270472109318,0.478905194997787,
5.37));
#44897=CARTESIAN_POINT('',(-1.52244199812412,0.518110537528992,5.4));
#44898=CARTESIAN_POINT('Ctrl Pts',(-1.52244199812412,0.518110537528992,
5.4));
#44899=CARTESIAN_POINT('Ctrl Pts',(-1.5014324337244,0.498976820707321,5.4));
#44900=CARTESIAN_POINT('Ctrl Pts',(-1.41270472109318,0.478905194997787,
5.4));
#44901=CARTESIAN_POINT('',(-1.52244199812412,0.518110537528992,5.37));
#44902=CARTESIAN_POINT('',(-1.52244199812412,0.518110537528992,5.4));
#44903=CARTESIAN_POINT('Ctrl Pts',(-1.52244199812412,0.518110537528992,
5.37));
#44904=CARTESIAN_POINT('Ctrl Pts',(-1.5014324337244,0.498976820707321,5.37));
#44905=CARTESIAN_POINT('Ctrl Pts',(-1.41270472109318,0.478905194997787,
5.37));
#44906=CARTESIAN_POINT('Ctrl Pts',(-1.54382671415806,0.566882693767548,
5.4));
#44907=CARTESIAN_POINT('Ctrl Pts',(-1.54382671415806,0.566882693767548,
5.37));
#44908=CARTESIAN_POINT('Ctrl Pts',(-1.54382671415806,0.53724422454834,5.4));
#44909=CARTESIAN_POINT('Ctrl Pts',(-1.54382671415806,0.53724422454834,5.37));
#44910=CARTESIAN_POINT('Ctrl Pts',(-1.52244199812412,0.518110537528992,
5.4));
#44911=CARTESIAN_POINT('Ctrl Pts',(-1.52244199812412,0.518110537528992,
5.37));
#44912=CARTESIAN_POINT('',(-1.54382671415806,0.566882693767548,5.4));
#44913=CARTESIAN_POINT('Ctrl Pts',(-1.54382671415806,0.566882693767548,
5.4));
#44914=CARTESIAN_POINT('Ctrl Pts',(-1.54382671415806,0.53724422454834,5.4));
#44915=CARTESIAN_POINT('Ctrl Pts',(-1.52244199812412,0.518110537528992,
5.4));
#44916=CARTESIAN_POINT('',(-1.54382671415806,0.566882693767548,5.37));
#44917=CARTESIAN_POINT('',(-1.54382671415806,0.566882693767548,5.4));
#44918=CARTESIAN_POINT('Ctrl Pts',(-1.54382671415806,0.566882693767548,
5.37));
#44919=CARTESIAN_POINT('Ctrl Pts',(-1.54382671415806,0.53724422454834,5.37));
#44920=CARTESIAN_POINT('Ctrl Pts',(-1.52244199812412,0.518110537528992,
5.37));
#44921=CARTESIAN_POINT('Ctrl Pts',(-1.51362551748753,0.6252217233181,5.4));
#44922=CARTESIAN_POINT('Ctrl Pts',(-1.51362551748753,0.6252217233181,5.37));
#44923=CARTESIAN_POINT('Ctrl Pts',(-1.54382671415806,0.60102322101593,5.4));
#44924=CARTESIAN_POINT('Ctrl Pts',(-1.54382671415806,0.60102322101593,5.37));
#44925=CARTESIAN_POINT('Ctrl Pts',(-1.54382671415806,0.566882693767548,
5.4));
#44926=CARTESIAN_POINT('Ctrl Pts',(-1.54382671415806,0.566882693767548,
5.37));
#44927=CARTESIAN_POINT('',(-1.51362551748753,0.6252217233181,5.4));
#44928=CARTESIAN_POINT('Ctrl Pts',(-1.51362551748753,0.6252217233181,5.4));
#44929=CARTESIAN_POINT('Ctrl Pts',(-1.54382671415806,0.60102322101593,5.4));
#44930=CARTESIAN_POINT('Ctrl Pts',(-1.54382671415806,0.566882693767548,
5.4));
#44931=CARTESIAN_POINT('',(-1.51362551748753,0.6252217233181,5.37));
#44932=CARTESIAN_POINT('',(-1.51362551748753,0.6252217233181,5.4));
#44933=CARTESIAN_POINT('Ctrl Pts',(-1.51362551748753,0.6252217233181,5.37));
#44934=CARTESIAN_POINT('Ctrl Pts',(-1.54382671415806,0.60102322101593,5.37));
#44935=CARTESIAN_POINT('Ctrl Pts',(-1.54382671415806,0.566882693767548,
5.37));
#44936=CARTESIAN_POINT('Ctrl Pts',(-1.41739429533482,0.64942022562027,5.4));
#44937=CARTESIAN_POINT('Ctrl Pts',(-1.41739429533482,0.64942022562027,5.37));
#44938=CARTESIAN_POINT('Ctrl Pts',(-1.48342432081699,0.64942022562027,5.4));
#44939=CARTESIAN_POINT('Ctrl Pts',(-1.48342432081699,0.64942022562027,5.37));
#44940=CARTESIAN_POINT('Ctrl Pts',(-1.51362551748753,0.6252217233181,5.4));
#44941=CARTESIAN_POINT('Ctrl Pts',(-1.51362551748753,0.6252217233181,5.37));
#44942=CARTESIAN_POINT('',(-1.41739429533482,0.64942022562027,5.4));
#44943=CARTESIAN_POINT('Ctrl Pts',(-1.41739429533482,0.64942022562027,5.4));
#44944=CARTESIAN_POINT('Ctrl Pts',(-1.48342432081699,0.64942022562027,5.4));
#44945=CARTESIAN_POINT('Ctrl Pts',(-1.51362551748753,0.6252217233181,5.4));
#44946=CARTESIAN_POINT('',(-1.41739429533482,0.64942022562027,5.37));
#44947=CARTESIAN_POINT('',(-1.41739429533482,0.64942022562027,5.4));
#44948=CARTESIAN_POINT('Ctrl Pts',(-1.41739429533482,0.64942022562027,5.37));
#44949=CARTESIAN_POINT('Ctrl Pts',(-1.48342432081699,0.64942022562027,5.37));
#44950=CARTESIAN_POINT('Ctrl Pts',(-1.51362551748753,0.6252217233181,5.37));
#44951=CARTESIAN_POINT('Ctrl Pts',(-1.32153822481632,0.622783118486404,
5.4));
#44952=CARTESIAN_POINT('Ctrl Pts',(-1.32153822481632,0.622783118486404,
5.37));
#44953=CARTESIAN_POINT('Ctrl Pts',(-1.35399045050144,0.64942022562027,5.4));
#44954=CARTESIAN_POINT('Ctrl Pts',(-1.35399045050144,0.64942022562027,5.37));
#44955=CARTESIAN_POINT('Ctrl Pts',(-1.41739429533482,0.64942022562027,5.4));
#44956=CARTESIAN_POINT('Ctrl Pts',(-1.41739429533482,0.64942022562027,5.37));
#44957=CARTESIAN_POINT('',(-1.32153822481632,0.622783118486404,5.4));
#44958=CARTESIAN_POINT('Ctrl Pts',(-1.32153822481632,0.622783118486404,
5.4));
#44959=CARTESIAN_POINT('Ctrl Pts',(-1.35399045050144,0.64942022562027,5.4));
#44960=CARTESIAN_POINT('Ctrl Pts',(-1.41739429533482,0.64942022562027,5.4));
#44961=CARTESIAN_POINT('',(-1.32153822481632,0.622783118486404,5.37));
#44962=CARTESIAN_POINT('',(-1.32153822481632,0.622783118486404,5.4));
#44963=CARTESIAN_POINT('Ctrl Pts',(-1.32153822481632,0.622783118486404,
5.37));
#44964=CARTESIAN_POINT('Ctrl Pts',(-1.35399045050144,0.64942022562027,5.37));
#44965=CARTESIAN_POINT('Ctrl Pts',(-1.41739429533482,0.64942022562027,5.37));
#44966=CARTESIAN_POINT('Ctrl Pts',(-1.28345836699009,0.54399728178978,5.4));
#44967=CARTESIAN_POINT('Ctrl Pts',(-1.28345836699009,0.54399728178978,5.37));
#44968=CARTESIAN_POINT('Ctrl Pts',(-1.2890859991312,0.596146011352539,5.4));
#44969=CARTESIAN_POINT('Ctrl Pts',(-1.2890859991312,0.596146011352539,5.37));
#44970=CARTESIAN_POINT('Ctrl Pts',(-1.32153822481632,0.622783118486404,
5.4));
#44971=CARTESIAN_POINT('Ctrl Pts',(-1.32153822481632,0.622783118486404,
5.37));
#44972=CARTESIAN_POINT('',(-1.28345836699009,0.54399728178978,5.4));
#44973=CARTESIAN_POINT('Ctrl Pts',(-1.28345836699009,0.54399728178978,5.4));
#44974=CARTESIAN_POINT('Ctrl Pts',(-1.2890859991312,0.596146011352539,5.4));
#44975=CARTESIAN_POINT('Ctrl Pts',(-1.32153822481632,0.622783118486404,
5.4));
#44976=CARTESIAN_POINT('',(-1.28345836699009,0.54399728178978,5.37));
#44977=CARTESIAN_POINT('',(-1.28345836699009,0.54399728178978,5.4));
#44978=CARTESIAN_POINT('Ctrl Pts',(-1.28345836699009,0.54399728178978,5.37));
#44979=CARTESIAN_POINT('Ctrl Pts',(-1.2890859991312,0.596146011352539,5.37));
#44980=CARTESIAN_POINT('Ctrl Pts',(-1.32153822481632,0.622783118486404,
5.37));
#44981=CARTESIAN_POINT('Origin',(-1.21367670595646,0.549249672889709,5.4));
#44982=CARTESIAN_POINT('',(-1.21367670595646,0.549249672889709,5.4));
#44983=CARTESIAN_POINT('',(-0.630811244176041,0.59312133370381,5.4));
#44984=CARTESIAN_POINT('',(-1.21367670595646,0.549249672889709,5.37));
#44985=CARTESIAN_POINT('',(-1.21367670595646,0.549249672889709,5.4));
#44986=CARTESIAN_POINT('',(-1.21367670595646,0.549249672889709,5.37));
#44987=CARTESIAN_POINT('Ctrl Pts',(-1.24068893492222,0.635914081335068,
5.4));
#44988=CARTESIAN_POINT('Ctrl Pts',(-1.24068893492222,0.635914081335068,
5.37));
#44989=CARTESIAN_POINT('Ctrl Pts',(-1.21555258333683,0.597646677494049,
5.4));
#44990=CARTESIAN_POINT('Ctrl Pts',(-1.21555258333683,0.597646677494049,
5.37));
#44991=CARTESIAN_POINT('Ctrl Pts',(-1.21367670595646,0.549249672889709,
5.4));
#44992=CARTESIAN_POINT('Ctrl Pts',(-1.21367670595646,0.549249672889709,
5.37));
#44993=CARTESIAN_POINT('',(-1.24068893492222,0.635914081335068,5.4));
#44994=CARTESIAN_POINT('Ctrl Pts',(-1.24068893492222,0.635914081335068,
5.4));
#44995=CARTESIAN_POINT('Ctrl Pts',(-1.21555258333683,0.597646677494049,
5.4));
#44996=CARTESIAN_POINT('Ctrl Pts',(-1.21367670595646,0.549249672889709,
5.4));
#44997=CARTESIAN_POINT('',(-1.24068893492222,0.635914081335068,5.37));
#44998=CARTESIAN_POINT('',(-1.24068893492222,0.635914081335068,5.4));
#44999=CARTESIAN_POINT('Ctrl Pts',(-1.24068893492222,0.635914081335068,
5.37));
#45000=CARTESIAN_POINT('Ctrl Pts',(-1.21555258333683,0.597646677494049,
5.37));
#45001=CARTESIAN_POINT('Ctrl Pts',(-1.21367670595646,0.549249672889709,
5.37));
#45002=CARTESIAN_POINT('Ctrl Pts',(-1.31253410875797,0.693877899646759,
5.4));
#45003=CARTESIAN_POINT('Ctrl Pts',(-1.31253410875797,0.693877899646759,
5.37));
#45004=CARTESIAN_POINT('Ctrl Pts',(-1.2658254057169,0.674181485176086,5.4));
#45005=CARTESIAN_POINT('Ctrl Pts',(-1.2658254057169,0.674181485176086,5.37));
#45006=CARTESIAN_POINT('Ctrl Pts',(-1.24068893492222,0.635914081335068,
5.4));
#45007=CARTESIAN_POINT('Ctrl Pts',(-1.24068893492222,0.635914081335068,
5.37));
#45008=CARTESIAN_POINT('',(-1.31253410875797,0.693877899646759,5.4));
#45009=CARTESIAN_POINT('Ctrl Pts',(-1.31253410875797,0.693877899646759,
5.4));
#45010=CARTESIAN_POINT('Ctrl Pts',(-1.2658254057169,0.674181485176086,5.4));
#45011=CARTESIAN_POINT('Ctrl Pts',(-1.24068893492222,0.635914081335068,
5.4));
#45012=CARTESIAN_POINT('',(-1.31253410875797,0.693877899646759,5.37));
#45013=CARTESIAN_POINT('',(-1.31253410875797,0.693877899646759,5.4));
#45014=CARTESIAN_POINT('Ctrl Pts',(-1.31253410875797,0.693877899646759,
5.37));
#45015=CARTESIAN_POINT('Ctrl Pts',(-1.2658254057169,0.674181485176086,5.37));
#45016=CARTESIAN_POINT('Ctrl Pts',(-1.24068893492222,0.635914081335068,
5.37));
#45017=CARTESIAN_POINT('Ctrl Pts',(-1.42039562761784,0.713574373722076,
5.4));
#45018=CARTESIAN_POINT('Ctrl Pts',(-1.42039562761784,0.713574373722076,
5.37));
#45019=CARTESIAN_POINT('Ctrl Pts',(-1.35924281179905,0.713574373722076,
5.4));
#45020=CARTESIAN_POINT('Ctrl Pts',(-1.35924281179905,0.713574373722076,
5.37));
#45021=CARTESIAN_POINT('Ctrl Pts',(-1.31253410875797,0.693877899646759,
5.4));
#45022=CARTESIAN_POINT('Ctrl Pts',(-1.31253410875797,0.693877899646759,
5.37));
#45023=CARTESIAN_POINT('',(-1.42039562761784,0.713574373722076,5.4));
#45024=CARTESIAN_POINT('Ctrl Pts',(-1.42039562761784,0.713574373722076,
5.4));
#45025=CARTESIAN_POINT('Ctrl Pts',(-1.35924281179905,0.713574373722076,
5.4));
#45026=CARTESIAN_POINT('Ctrl Pts',(-1.31253410875797,0.693877899646759,
5.4));
#45027=CARTESIAN_POINT('',(-1.42039562761784,0.713574373722076,5.37));
#45028=CARTESIAN_POINT('',(-1.42039562761784,0.713574373722076,5.4));
#45029=CARTESIAN_POINT('Ctrl Pts',(-1.42039562761784,0.713574373722076,
5.37));
#45030=CARTESIAN_POINT('Ctrl Pts',(-1.35924281179905,0.713574373722076,
5.37));
#45031=CARTESIAN_POINT('Ctrl Pts',(-1.31253410875797,0.693877899646759,
5.37));
#45032=CARTESIAN_POINT('Ctrl Pts',(-1.52131654322147,0.694815838336945,
5.4));
#45033=CARTESIAN_POINT('Ctrl Pts',(-1.52131654322147,0.694815838336945,
5.37));
#45034=CARTESIAN_POINT('Ctrl Pts',(-1.4759209305048,0.713574373722076,5.4));
#45035=CARTESIAN_POINT('Ctrl Pts',(-1.4759209305048,0.713574373722076,5.37));
#45036=CARTESIAN_POINT('Ctrl Pts',(-1.42039562761784,0.713574373722076,
5.4));
#45037=CARTESIAN_POINT('Ctrl Pts',(-1.42039562761784,0.713574373722076,
5.37));
#45038=CARTESIAN_POINT('',(-1.52131654322147,0.694815838336945,5.4));
#45039=CARTESIAN_POINT('Ctrl Pts',(-1.52131654322147,0.694815838336945,
5.4));
#45040=CARTESIAN_POINT('Ctrl Pts',(-1.4759209305048,0.713574373722076,5.4));
#45041=CARTESIAN_POINT('Ctrl Pts',(-1.42039562761784,0.713574373722076,
5.4));
#45042=CARTESIAN_POINT('',(-1.52131654322147,0.694815838336945,5.37));
#45043=CARTESIAN_POINT('',(-1.52131654322147,0.694815838336945,5.4));
#45044=CARTESIAN_POINT('Ctrl Pts',(-1.52131654322147,0.694815838336945,
5.37));
#45045=CARTESIAN_POINT('Ctrl Pts',(-1.4759209305048,0.713574373722076,5.37));
#45046=CARTESIAN_POINT('Ctrl Pts',(-1.42039562761784,0.713574373722076,
5.37));
#45047=CARTESIAN_POINT('Ctrl Pts',(-1.59034790098667,0.639853382110596,
5.4));
#45048=CARTESIAN_POINT('Ctrl Pts',(-1.59034790098667,0.639853382110596,
5.37));
#45049=CARTESIAN_POINT('Ctrl Pts',(-1.56671215593815,0.676057302951813,
5.4));
#45050=CARTESIAN_POINT('Ctrl Pts',(-1.56671215593815,0.676057302951813,
5.37));
#45051=CARTESIAN_POINT('Ctrl Pts',(-1.52131654322147,0.694815838336945,
5.4));
#45052=CARTESIAN_POINT('Ctrl Pts',(-1.52131654322147,0.694815838336945,
5.37));
#45053=CARTESIAN_POINT('',(-1.59034790098667,0.639853382110596,5.4));
#45054=CARTESIAN_POINT('Ctrl Pts',(-1.59034790098667,0.639853382110596,
5.4));
#45055=CARTESIAN_POINT('Ctrl Pts',(-1.56671215593815,0.676057302951813,
5.4));
#45056=CARTESIAN_POINT('Ctrl Pts',(-1.52131654322147,0.694815838336945,
5.4));
#45057=CARTESIAN_POINT('',(-1.59034790098667,0.639853382110596,5.37));
#45058=CARTESIAN_POINT('',(-1.59034790098667,0.639853382110596,5.4));
#45059=CARTESIAN_POINT('Ctrl Pts',(-1.59034790098667,0.639853382110596,
5.37));
#45060=CARTESIAN_POINT('Ctrl Pts',(-1.56671215593815,0.676057302951813,
5.37));
#45061=CARTESIAN_POINT('Ctrl Pts',(-1.52131654322147,0.694815838336945,
5.37));
#45062=CARTESIAN_POINT('Ctrl Pts',(-1.61398364603519,0.562005484104157,
5.4));
#45063=CARTESIAN_POINT('Ctrl Pts',(-1.61398364603519,0.562005484104157,
5.37));
#45064=CARTESIAN_POINT('Ctrl Pts',(-1.61398364603519,0.603649401664734,
5.4));
#45065=CARTESIAN_POINT('Ctrl Pts',(-1.61398364603519,0.603649401664734,
5.37));
#45066=CARTESIAN_POINT('Ctrl Pts',(-1.59034790098667,0.639853382110596,
5.4));
#45067=CARTESIAN_POINT('Ctrl Pts',(-1.59034790098667,0.639853382110596,
5.37));
#45068=CARTESIAN_POINT('',(-1.61398364603519,0.562005484104157,5.4));
#45069=CARTESIAN_POINT('Ctrl Pts',(-1.61398364603519,0.562005484104157,
5.4));
#45070=CARTESIAN_POINT('Ctrl Pts',(-1.61398364603519,0.603649401664734,
5.4));
#45071=CARTESIAN_POINT('Ctrl Pts',(-1.59034790098667,0.639853382110596,
5.4));
#45072=CARTESIAN_POINT('',(-1.61398364603519,0.562005484104157,5.37));
#45073=CARTESIAN_POINT('',(-1.61398364603519,0.562005484104157,5.4));
#45074=CARTESIAN_POINT('Ctrl Pts',(-1.61398364603519,0.562005484104157,
5.37));
#45075=CARTESIAN_POINT('Ctrl Pts',(-1.61398364603519,0.603649401664734,
5.37));
#45076=CARTESIAN_POINT('Ctrl Pts',(-1.59034790098667,0.639853382110596,
5.37));
#45077=CARTESIAN_POINT('Ctrl Pts',(-1.59466232359409,0.493536853790283,
5.4));
#45078=CARTESIAN_POINT('Ctrl Pts',(-1.59466232359409,0.493536853790283,
5.37));
#45079=CARTESIAN_POINT('Ctrl Pts',(-1.61398364603519,0.524113261699677,
5.4));
#45080=CARTESIAN_POINT('Ctrl Pts',(-1.61398364603519,0.524113261699677,
5.37));
#45081=CARTESIAN_POINT('Ctrl Pts',(-1.61398364603519,0.562005484104157,
5.4));
#45082=CARTESIAN_POINT('Ctrl Pts',(-1.61398364603519,0.562005484104157,
5.37));
#45083=CARTESIAN_POINT('',(-1.59466232359409,0.493536853790283,5.4));
#45084=CARTESIAN_POINT('Ctrl Pts',(-1.59466232359409,0.493536853790283,
5.4));
#45085=CARTESIAN_POINT('Ctrl Pts',(-1.61398364603519,0.524113261699677,
5.4));
#45086=CARTESIAN_POINT('Ctrl Pts',(-1.61398364603519,0.562005484104157,
5.4));
#45087=CARTESIAN_POINT('',(-1.59466232359409,0.493536853790283,5.37));
#45088=CARTESIAN_POINT('',(-1.59466232359409,0.493536853790283,5.4));
#45089=CARTESIAN_POINT('Ctrl Pts',(-1.59466232359409,0.493536853790283,
5.37));
#45090=CARTESIAN_POINT('Ctrl Pts',(-1.61398364603519,0.524113261699677,
5.37));
#45091=CARTESIAN_POINT('Ctrl Pts',(-1.61398364603519,0.562005484104157,
5.37));
#45092=CARTESIAN_POINT('Ctrl Pts',(-1.53594817221165,0.442326062917709,
5.4));
#45093=CARTESIAN_POINT('Ctrl Pts',(-1.53594817221165,0.442326062917709,
5.37));
#45094=CARTESIAN_POINT('Ctrl Pts',(-1.57534112036228,0.46296044588089,5.4));
#45095=CARTESIAN_POINT('Ctrl Pts',(-1.57534112036228,0.46296044588089,5.37));
#45096=CARTESIAN_POINT('Ctrl Pts',(-1.59466232359409,0.493536853790283,
5.4));
#45097=CARTESIAN_POINT('Ctrl Pts',(-1.59466232359409,0.493536853790283,
5.37));
#45098=CARTESIAN_POINT('',(-1.53594817221165,0.442326062917709,5.4));
#45099=CARTESIAN_POINT('Ctrl Pts',(-1.53594817221165,0.442326062917709,
5.4));
#45100=CARTESIAN_POINT('Ctrl Pts',(-1.57534112036228,0.46296044588089,5.4));
#45101=CARTESIAN_POINT('Ctrl Pts',(-1.59466232359409,0.493536853790283,
5.4));
#45102=CARTESIAN_POINT('',(-1.53594817221165,0.442326062917709,5.37));
#45103=CARTESIAN_POINT('',(-1.53594817221165,0.442326062917709,5.4));
#45104=CARTESIAN_POINT('Ctrl Pts',(-1.53594817221165,0.442326062917709,
5.37));
#45105=CARTESIAN_POINT('Ctrl Pts',(-1.57534112036228,0.46296044588089,5.37));
#45106=CARTESIAN_POINT('Ctrl Pts',(-1.59466232359409,0.493536853790283,
5.37));
#45107=CARTESIAN_POINT('Ctrl Pts',(-1.4297748953104,0.407997959852219,5.4));
#45108=CARTESIAN_POINT('Ctrl Pts',(-1.4297748953104,0.407997959852219,5.37));
#45109=CARTESIAN_POINT('Ctrl Pts',(-1.50555934011936,0.426193737983704,
5.4));
#45110=CARTESIAN_POINT('Ctrl Pts',(-1.50555934011936,0.426193737983704,
5.37));
#45111=CARTESIAN_POINT('Ctrl Pts',(-1.53594817221165,0.442326062917709,
5.4));
#45112=CARTESIAN_POINT('Ctrl Pts',(-1.53594817221165,0.442326062917709,
5.37));
#45113=CARTESIAN_POINT('',(-1.4297748953104,0.407997959852219,5.4));
#45114=CARTESIAN_POINT('Ctrl Pts',(-1.4297748953104,0.407997959852219,5.4));
#45115=CARTESIAN_POINT('Ctrl Pts',(-1.50555934011936,0.426193737983704,
5.4));
#45116=CARTESIAN_POINT('Ctrl Pts',(-1.53594817221165,0.442326062917709,
5.4));
#45117=CARTESIAN_POINT('',(-1.4297748953104,0.407997959852219,5.37));
#45118=CARTESIAN_POINT('',(-1.4297748953104,0.407997959852219,5.4));
#45119=CARTESIAN_POINT('Ctrl Pts',(-1.4297748953104,0.407997959852219,5.37));
#45120=CARTESIAN_POINT('Ctrl Pts',(-1.50555934011936,0.426193737983704,
5.37));
#45121=CARTESIAN_POINT('Ctrl Pts',(-1.53594817221165,0.442326062917709,
5.37));
#45122=CARTESIAN_POINT('Ctrl Pts',(-1.33185543119907,0.381173276901245,
5.4));
#45123=CARTESIAN_POINT('Ctrl Pts',(-1.33185543119907,0.381173276901245,
5.37));
#45124=CARTESIAN_POINT('Ctrl Pts',(-1.35399045050144,0.389802196621895,
5.4));
#45125=CARTESIAN_POINT('Ctrl Pts',(-1.35399045050144,0.389802196621895,
5.37));
#45126=CARTESIAN_POINT('Ctrl Pts',(-1.4297748953104,0.407997959852219,5.4));
#45127=CARTESIAN_POINT('Ctrl Pts',(-1.4297748953104,0.407997959852219,5.37));
#45128=CARTESIAN_POINT('',(-1.33185543119907,0.381173276901245,5.4));
#45129=CARTESIAN_POINT('Ctrl Pts',(-1.33185543119907,0.381173276901245,
5.4));
#45130=CARTESIAN_POINT('Ctrl Pts',(-1.35399045050144,0.389802196621895,
5.4));
#45131=CARTESIAN_POINT('Ctrl Pts',(-1.4297748953104,0.407997959852219,5.4));
#45132=CARTESIAN_POINT('',(-1.33185543119907,0.381173276901245,5.37));
#45133=CARTESIAN_POINT('',(-1.33185543119907,0.381173276901245,5.4));
#45134=CARTESIAN_POINT('Ctrl Pts',(-1.33185543119907,0.381173276901245,
5.37));
#45135=CARTESIAN_POINT('Ctrl Pts',(-1.35399045050144,0.389802196621895,
5.37));
#45136=CARTESIAN_POINT('Ctrl Pts',(-1.4297748953104,0.407997959852219,5.37));
#45137=CARTESIAN_POINT('Ctrl Pts',(-1.28233291208744,0.348721021413803,
5.4));
#45138=CARTESIAN_POINT('Ctrl Pts',(-1.28233291208744,0.348721021413803,
5.37));
#45139=CARTESIAN_POINT('Ctrl Pts',(-1.29733969271183,0.368042299151421,
5.4));
#45140=CARTESIAN_POINT('Ctrl Pts',(-1.29733969271183,0.368042299151421,
5.37));
#45141=CARTESIAN_POINT('Ctrl Pts',(-1.33185543119907,0.381173276901245,
5.4));
#45142=CARTESIAN_POINT('Ctrl Pts',(-1.33185543119907,0.381173276901245,
5.37));
#45143=CARTESIAN_POINT('',(-1.28233291208744,0.348721021413803,5.4));
#45144=CARTESIAN_POINT('Ctrl Pts',(-1.28233291208744,0.348721021413803,
5.4));
#45145=CARTESIAN_POINT('Ctrl Pts',(-1.29733969271183,0.368042299151421,
5.4));
#45146=CARTESIAN_POINT('Ctrl Pts',(-1.33185543119907,0.381173276901245,
5.4));
#45147=CARTESIAN_POINT('',(-1.28233291208744,0.348721021413803,5.37));
#45148=CARTESIAN_POINT('',(-1.28233291208744,0.348721021413803,5.4));
#45149=CARTESIAN_POINT('Ctrl Pts',(-1.28233291208744,0.348721021413803,
5.37));
#45150=CARTESIAN_POINT('Ctrl Pts',(-1.29733969271183,0.368042299151421,
5.37));
#45151=CARTESIAN_POINT('Ctrl Pts',(-1.33185543119907,0.381173276901245,
5.37));
#45152=CARTESIAN_POINT('Ctrl Pts',(-1.26732613146305,0.303512969613075,
5.4));
#45153=CARTESIAN_POINT('Ctrl Pts',(-1.26732613146305,0.303512969613075,
5.37));
#45154=CARTESIAN_POINT('Ctrl Pts',(-1.26732613146305,0.329399743676186,
5.4));
#45155=CARTESIAN_POINT('Ctrl Pts',(-1.26732613146305,0.329399743676186,
5.37));
#45156=CARTESIAN_POINT('Ctrl Pts',(-1.28233291208744,0.348721021413803,
5.4));
#45157=CARTESIAN_POINT('Ctrl Pts',(-1.28233291208744,0.348721021413803,
5.37));
#45158=CARTESIAN_POINT('',(-1.26732613146305,0.303512969613075,5.4));
#45159=CARTESIAN_POINT('Ctrl Pts',(-1.26732613146305,0.303512969613075,
5.4));
#45160=CARTESIAN_POINT('Ctrl Pts',(-1.26732613146305,0.329399743676186,
5.4));
#45161=CARTESIAN_POINT('Ctrl Pts',(-1.28233291208744,0.348721021413803,
5.4));
#45162=CARTESIAN_POINT('',(-1.26732613146305,0.303512969613075,5.37));
#45163=CARTESIAN_POINT('',(-1.26732613146305,0.303512969613075,5.4));
#45164=CARTESIAN_POINT('Ctrl Pts',(-1.26732613146305,0.303512969613075,
5.37));
#45165=CARTESIAN_POINT('Ctrl Pts',(-1.26732613146305,0.329399743676186,
5.37));
#45166=CARTESIAN_POINT('Ctrl Pts',(-1.28233291208744,0.348721021413803,
5.37));
#45167=CARTESIAN_POINT('Ctrl Pts',(-1.28289557993412,0.256429070234299,
5.4));
#45168=CARTESIAN_POINT('Ctrl Pts',(-1.28289557993412,0.256429070234299,
5.37));
#45169=CARTESIAN_POINT('Ctrl Pts',(-1.26732613146305,0.278001391887665,
5.4));
#45170=CARTESIAN_POINT('Ctrl Pts',(-1.26732613146305,0.278001391887665,
5.37));
#45171=CARTESIAN_POINT('Ctrl Pts',(-1.26732613146305,0.303512969613075,
5.4));
#45172=CARTESIAN_POINT('Ctrl Pts',(-1.26732613146305,0.303512969613075,
5.37));
#45173=CARTESIAN_POINT('',(-1.28289557993412,0.256429070234299,5.4));
#45174=CARTESIAN_POINT('Ctrl Pts',(-1.28289557993412,0.256429070234299,
5.4));
#45175=CARTESIAN_POINT('Ctrl Pts',(-1.26732613146305,0.278001391887665,
5.4));
#45176=CARTESIAN_POINT('Ctrl Pts',(-1.26732613146305,0.303512969613075,
5.4));
#45177=CARTESIAN_POINT('',(-1.28289557993412,0.256429070234299,5.37));
#45178=CARTESIAN_POINT('',(-1.28289557993412,0.256429070234299,5.4));
#45179=CARTESIAN_POINT('Ctrl Pts',(-1.28289557993412,0.256429070234299,
5.37));
#45180=CARTESIAN_POINT('Ctrl Pts',(-1.26732613146305,0.278001391887665,
5.37));
#45181=CARTESIAN_POINT('Ctrl Pts',(-1.26732613146305,0.303512969613075,
5.37));
#45182=CARTESIAN_POINT('Ctrl Pts',(-1.33035470545292,0.222476148605347,
5.4));
#45183=CARTESIAN_POINT('Ctrl Pts',(-1.33035470545292,0.222476148605347,
5.37));
#45184=CARTESIAN_POINT('Ctrl Pts',(-1.29846526682377,0.234856748580933,
5.4));
#45185=CARTESIAN_POINT('Ctrl Pts',(-1.29846526682377,0.234856748580933,
5.37));
#45186=CARTESIAN_POINT('Ctrl Pts',(-1.28289557993412,0.256429070234299,
5.4));
#45187=CARTESIAN_POINT('Ctrl Pts',(-1.28289557993412,0.256429070234299,
5.37));
#45188=CARTESIAN_POINT('',(-1.33035470545292,0.222476148605347,5.4));
#45189=CARTESIAN_POINT('Ctrl Pts',(-1.33035470545292,0.222476148605347,
5.4));
#45190=CARTESIAN_POINT('Ctrl Pts',(-1.29846526682377,0.234856748580933,
5.4));
#45191=CARTESIAN_POINT('Ctrl Pts',(-1.28289557993412,0.256429070234299,
5.4));
#45192=CARTESIAN_POINT('',(-1.33035470545292,0.222476148605347,5.37));
#45193=CARTESIAN_POINT('',(-1.33035470545292,0.222476148605347,5.4));
#45194=CARTESIAN_POINT('Ctrl Pts',(-1.33035470545292,0.222476148605347,
5.37));
#45195=CARTESIAN_POINT('Ctrl Pts',(-1.29846526682377,0.234856748580933,
5.37));
#45196=CARTESIAN_POINT('Ctrl Pts',(-1.28289557993412,0.256429070234299,
5.37));
#45197=CARTESIAN_POINT('Ctrl Pts',(-1.40388812124729,0.210095518827438,
5.4));
#45198=CARTESIAN_POINT('Ctrl Pts',(-1.40388812124729,0.210095518827438,
5.37));
#45199=CARTESIAN_POINT('Ctrl Pts',(-1.36224426329136,0.210095518827438,
5.4));
#45200=CARTESIAN_POINT('Ctrl Pts',(-1.36224426329136,0.210095518827438,
5.37));
#45201=CARTESIAN_POINT('Ctrl Pts',(-1.33035470545292,0.222476148605347,
5.4));
#45202=CARTESIAN_POINT('Ctrl Pts',(-1.33035470545292,0.222476148605347,
5.37));
#45203=CARTESIAN_POINT('',(-1.40388812124729,0.210095518827438,5.4));
#45204=CARTESIAN_POINT('Ctrl Pts',(-1.40388812124729,0.210095518827438,
5.4));
#45205=CARTESIAN_POINT('Ctrl Pts',(-1.36224426329136,0.210095518827438,
5.4));
#45206=CARTESIAN_POINT('Ctrl Pts',(-1.33035470545292,0.222476148605347,
5.4));
#45207=CARTESIAN_POINT('',(-1.40388812124729,0.210095518827438,5.37));
#45208=CARTESIAN_POINT('',(-1.40388812124729,0.210095518827438,5.4));
#45209=CARTESIAN_POINT('Ctrl Pts',(-1.40388812124729,0.210095518827438,
5.37));
#45210=CARTESIAN_POINT('Ctrl Pts',(-1.36224426329136,0.210095518827438,
5.37));
#45211=CARTESIAN_POINT('Ctrl Pts',(-1.33035470545292,0.222476148605347,
5.37));
#45212=CARTESIAN_POINT('Ctrl Pts',(-1.48830153048038,0.226415419578552,
5.4));
#45213=CARTESIAN_POINT('Ctrl Pts',(-1.48830153048038,0.226415419578552,
5.37));
#45214=CARTESIAN_POINT('Ctrl Pts',(-1.45078445971012,0.210095518827438,
5.4));
#45215=CARTESIAN_POINT('Ctrl Pts',(-1.45078445971012,0.210095518827438,
5.37));
#45216=CARTESIAN_POINT('Ctrl Pts',(-1.40388812124729,0.210095518827438,
5.4));
#45217=CARTESIAN_POINT('Ctrl Pts',(-1.40388812124729,0.210095518827438,
5.37));
#45218=CARTESIAN_POINT('',(-1.48830153048038,0.226415419578552,5.4));
#45219=CARTESIAN_POINT('Ctrl Pts',(-1.48830153048038,0.226415419578552,
5.4));
#45220=CARTESIAN_POINT('Ctrl Pts',(-1.45078445971012,0.210095518827438,
5.4));
#45221=CARTESIAN_POINT('Ctrl Pts',(-1.40388812124729,0.210095518827438,
5.4));
#45222=CARTESIAN_POINT('',(-1.48830153048038,0.226415419578552,5.37));
#45223=CARTESIAN_POINT('',(-1.48830153048038,0.226415419578552,5.4));
#45224=CARTESIAN_POINT('Ctrl Pts',(-1.48830153048038,0.226415419578552,
5.37));
#45225=CARTESIAN_POINT('Ctrl Pts',(-1.45078445971012,0.210095518827438,
5.37));
#45226=CARTESIAN_POINT('Ctrl Pts',(-1.40388812124729,0.210095518827438,
5.37));
#45227=CARTESIAN_POINT('Ctrl Pts',(-1.54363919794559,0.269184851646423,
5.4));
#45228=CARTESIAN_POINT('Ctrl Pts',(-1.54363919794559,0.269184851646423,
5.37));
#45229=CARTESIAN_POINT('Ctrl Pts',(-1.52581860125065,0.242735350131989,
5.4));
#45230=CARTESIAN_POINT('Ctrl Pts',(-1.52581860125065,0.242735350131989,
5.37));
#45231=CARTESIAN_POINT('Ctrl Pts',(-1.48830153048038,0.226415419578552,
5.4));
#45232=CARTESIAN_POINT('Ctrl Pts',(-1.48830153048038,0.226415419578552,
5.37));
#45233=CARTESIAN_POINT('',(-1.54363919794559,0.269184851646423,5.4));
#45234=CARTESIAN_POINT('Ctrl Pts',(-1.54363919794559,0.269184851646423,
5.4));
#45235=CARTESIAN_POINT('Ctrl Pts',(-1.52581860125065,0.242735350131989,
5.4));
#45236=CARTESIAN_POINT('Ctrl Pts',(-1.48830153048038,0.226415419578552,
5.4));
#45237=CARTESIAN_POINT('',(-1.54363919794559,0.269184851646423,5.37));
#45238=CARTESIAN_POINT('',(-1.54363919794559,0.269184851646423,5.4));
#45239=CARTESIAN_POINT('Ctrl Pts',(-1.54363919794559,0.269184851646423,
5.37));
#45240=CARTESIAN_POINT('Ctrl Pts',(-1.52581860125065,0.242735350131989,
5.37));
#45241=CARTESIAN_POINT('Ctrl Pts',(-1.48830153048038,0.226415419578552,
5.37));
#45242=CARTESIAN_POINT('Ctrl Pts',(-1.56633700430393,0.336903148889542,
5.4));
#45243=CARTESIAN_POINT('Ctrl Pts',(-1.56633700430393,0.336903148889542,
5.37));
#45244=CARTESIAN_POINT('Ctrl Pts',(-1.56145979464054,0.295634382963181,
5.4));
#45245=CARTESIAN_POINT('Ctrl Pts',(-1.56145979464054,0.295634382963181,
5.37));
#45246=CARTESIAN_POINT('Ctrl Pts',(-1.54363919794559,0.269184851646423,
5.4));
#45247=CARTESIAN_POINT('Ctrl Pts',(-1.54363919794559,0.269184851646423,
5.37));
#45248=CARTESIAN_POINT('',(-1.56633700430393,0.336903148889542,5.4));
#45249=CARTESIAN_POINT('Ctrl Pts',(-1.56633700430393,0.336903148889542,
5.4));
#45250=CARTESIAN_POINT('Ctrl Pts',(-1.56145979464054,0.295634382963181,
5.4));
#45251=CARTESIAN_POINT('Ctrl Pts',(-1.54363919794559,0.269184851646423,
5.4));
#45252=CARTESIAN_POINT('',(-1.56633700430393,0.336903148889542,5.37));
#45253=CARTESIAN_POINT('',(-1.56633700430393,0.336903148889542,5.4));
#45254=CARTESIAN_POINT('Ctrl Pts',(-1.56633700430393,0.336903148889542,
5.37));
#45255=CARTESIAN_POINT('Ctrl Pts',(-1.56145979464054,0.295634382963181,
5.37));
#45256=CARTESIAN_POINT('Ctrl Pts',(-1.54363919794559,0.269184851646423,
5.37));
#45257=CARTESIAN_POINT('Origin',(-1.63499321043491,0.330900424718857,5.4));
#45258=CARTESIAN_POINT('',(-1.63499321043491,0.330900424718857,5.4));
#45259=CARTESIAN_POINT('',(-0.838054220366137,0.400578101477175,5.4));
#45260=CARTESIAN_POINT('',(-1.63499321043491,0.330900424718857,5.37));
#45261=CARTESIAN_POINT('',(-1.63499321043491,0.330900424718857,5.4));
#45262=CARTESIAN_POINT('',(-1.63499321043491,0.330900424718857,5.37));
#45263=CARTESIAN_POINT('Ctrl Pts',(-1.60479201376438,0.232042992115021,
5.4));
#45264=CARTESIAN_POINT('Ctrl Pts',(-1.60479201376438,0.232042992115021,
5.37));
#45265=CARTESIAN_POINT('Ctrl Pts',(-1.63349248468876,0.275750362873077,
5.4));
#45266=CARTESIAN_POINT('Ctrl Pts',(-1.63349248468876,0.275750362873077,
5.37));
#45267=CARTESIAN_POINT('Ctrl Pts',(-1.63499321043491,0.330900424718857,
5.4));
#45268=CARTESIAN_POINT('Ctrl Pts',(-1.63499321043491,0.330900424718857,
5.37));
#45269=CARTESIAN_POINT('',(-1.60479201376438,0.232042992115021,5.4));
#45270=CARTESIAN_POINT('Ctrl Pts',(-1.60479201376438,0.232042992115021,
5.4));
#45271=CARTESIAN_POINT('Ctrl Pts',(-1.63349248468876,0.275750362873077,
5.4));
#45272=CARTESIAN_POINT('Ctrl Pts',(-1.63499321043491,0.330900424718857,
5.4));
#45273=CARTESIAN_POINT('',(-1.60479201376438,0.232042992115021,5.37));
#45274=CARTESIAN_POINT('',(-1.60479201376438,0.232042992115021,5.4));
#45275=CARTESIAN_POINT('Ctrl Pts',(-1.60479201376438,0.232042992115021,
5.37));
#45276=CARTESIAN_POINT('Ctrl Pts',(-1.63349248468876,0.275750362873077,
5.37));
#45277=CARTESIAN_POINT('Ctrl Pts',(-1.63499321043491,0.330900424718857,
5.37));
#45278=CARTESIAN_POINT('Ctrl Pts',(-1.5256309658289,0.16657572388649,5.4));
#45279=CARTESIAN_POINT('Ctrl Pts',(-1.5256309658289,0.16657572388649,5.37));
#45280=CARTESIAN_POINT('Ctrl Pts',(-1.57609142363071,0.188335621356964,
5.4));
#45281=CARTESIAN_POINT('Ctrl Pts',(-1.57609142363071,0.188335621356964,
5.37));
#45282=CARTESIAN_POINT('Ctrl Pts',(-1.60479201376438,0.232042992115021,
5.4));
#45283=CARTESIAN_POINT('Ctrl Pts',(-1.60479201376438,0.232042992115021,
5.37));
#45284=CARTESIAN_POINT('Ctrl Pts',(-1.5256309658289,0.16657572388649,5.4));
#45285=CARTESIAN_POINT('Ctrl Pts',(-1.57609142363071,0.188335621356964,
5.4));
#45286=CARTESIAN_POINT('Ctrl Pts',(-1.60479201376438,0.232042992115021,
5.4));
#45287=CARTESIAN_POINT('Ctrl Pts',(-1.5256309658289,0.16657572388649,5.37));
#45288=CARTESIAN_POINT('Ctrl Pts',(-1.57609142363071,0.188335621356964,
5.37));
#45289=CARTESIAN_POINT('Ctrl Pts',(-1.60479201376438,0.232042992115021,
5.37));
#45290=CARTESIAN_POINT('Origin',(-1.41608120501041,0.429195100069046,5.37));
#45291=CARTESIAN_POINT('Ctrl Pts',(-0.561255231499672,0.194525921344757,
5.4));
#45292=CARTESIAN_POINT('Ctrl Pts',(-0.561255231499672,0.194525921344757,
5.37));
#45293=CARTESIAN_POINT('Ctrl Pts',(-0.613779082894325,0.144440674781799,
5.4));
#45294=CARTESIAN_POINT('Ctrl Pts',(-0.613779082894325,0.144440674781799,
5.37));
#45295=CARTESIAN_POINT('Ctrl Pts',(-0.69406558573246,0.144440674781799,
5.4));
#45296=CARTESIAN_POINT('Ctrl Pts',(-0.69406558573246,0.144440674781799,
5.37));
#45297=CARTESIAN_POINT('',(-0.561255231499672,0.194525921344757,5.4));
#45298=CARTESIAN_POINT('',(-0.69406558573246,0.144440674781799,5.4));
#45299=CARTESIAN_POINT('Ctrl Pts',(-0.561255231499672,0.194525921344757,
5.4));
#45300=CARTESIAN_POINT('Ctrl Pts',(-0.613779082894325,0.144440674781799,
5.4));
#45301=CARTESIAN_POINT('Ctrl Pts',(-0.69406558573246,0.144440674781799,
5.4));
#45302=CARTESIAN_POINT('',(-0.561255231499672,0.194525921344757,5.37));
#45303=CARTESIAN_POINT('',(-0.561255231499672,0.194525921344757,5.4));
#45304=CARTESIAN_POINT('',(-0.69406558573246,0.144440674781799,5.37));
#45305=CARTESIAN_POINT('Ctrl Pts',(-0.561255231499672,0.194525921344757,
5.37));
#45306=CARTESIAN_POINT('Ctrl Pts',(-0.613779082894325,0.144440674781799,
5.37));
#45307=CARTESIAN_POINT('Ctrl Pts',(-0.69406558573246,0.144440674781799,
5.37));
#45308=CARTESIAN_POINT('',(-0.69406558573246,0.144440674781799,5.4));
#45309=CARTESIAN_POINT('Ctrl Pts',(-0.508731380105019,0.316643932461739,
5.4));
#45310=CARTESIAN_POINT('Ctrl Pts',(-0.508731380105019,0.316643932461739,
5.37));
#45311=CARTESIAN_POINT('Ctrl Pts',(-0.508731380105019,0.244611197710037,
5.4));
#45312=CARTESIAN_POINT('Ctrl Pts',(-0.508731380105019,0.244611197710037,
5.37));
#45313=CARTESIAN_POINT('Ctrl Pts',(-0.561255231499672,0.194525921344757,
5.4));
#45314=CARTESIAN_POINT('Ctrl Pts',(-0.561255231499672,0.194525921344757,
5.37));
#45315=CARTESIAN_POINT('',(-0.508731380105019,0.316643932461739,5.4));
#45316=CARTESIAN_POINT('Ctrl Pts',(-0.508731380105019,0.316643932461739,
5.4));
#45317=CARTESIAN_POINT('Ctrl Pts',(-0.508731380105019,0.244611197710037,
5.4));
#45318=CARTESIAN_POINT('Ctrl Pts',(-0.561255231499672,0.194525921344757,
5.4));
#45319=CARTESIAN_POINT('',(-0.508731380105019,0.316643932461739,5.37));
#45320=CARTESIAN_POINT('',(-0.508731380105019,0.316643932461739,5.4));
#45321=CARTESIAN_POINT('Ctrl Pts',(-0.508731380105019,0.316643932461739,
5.37));
#45322=CARTESIAN_POINT('Ctrl Pts',(-0.508731380105019,0.244611197710037,
5.37));
#45323=CARTESIAN_POINT('Ctrl Pts',(-0.561255231499672,0.194525921344757,
5.37));
#45324=CARTESIAN_POINT('Ctrl Pts',(-0.535743728280067,0.405371749401093,
5.4));
#45325=CARTESIAN_POINT('Ctrl Pts',(-0.535743728280067,0.405371749401093,
5.37));
#45326=CARTESIAN_POINT('Ctrl Pts',(-0.508731380105019,0.369918146729469,
5.4));
#45327=CARTESIAN_POINT('Ctrl Pts',(-0.508731380105019,0.369918146729469,
5.37));
#45328=CARTESIAN_POINT('Ctrl Pts',(-0.508731380105019,0.316643932461739,
5.4));
#45329=CARTESIAN_POINT('Ctrl Pts',(-0.508731380105019,0.316643932461739,
5.37));
#45330=CARTESIAN_POINT('',(-0.535743728280067,0.405371749401093,5.4));
#45331=CARTESIAN_POINT('Ctrl Pts',(-0.535743728280067,0.405371749401093,
5.4));
#45332=CARTESIAN_POINT('Ctrl Pts',(-0.508731380105019,0.369918146729469,
5.4));
#45333=CARTESIAN_POINT('Ctrl Pts',(-0.508731380105019,0.316643932461739,
5.4));
#45334=CARTESIAN_POINT('',(-0.535743728280067,0.405371749401093,5.37));
#45335=CARTESIAN_POINT('',(-0.535743728280067,0.405371749401093,5.4));
#45336=CARTESIAN_POINT('Ctrl Pts',(-0.535743728280067,0.405371749401093,
5.37));
#45337=CARTESIAN_POINT('Ctrl Pts',(-0.508731380105019,0.369918146729469,
5.37));
#45338=CARTESIAN_POINT('Ctrl Pts',(-0.508731380105019,0.316643932461739,
5.37));
#45339=CARTESIAN_POINT('Ctrl Pts',(-0.611528173089027,0.452080512046814,
5.4));
#45340=CARTESIAN_POINT('Ctrl Pts',(-0.611528173089027,0.452080512046814,
5.37));
#45341=CARTESIAN_POINT('Ctrl Pts',(-0.562755838036537,0.440825366973877,
5.4));
#45342=CARTESIAN_POINT('Ctrl Pts',(-0.562755838036537,0.440825366973877,
5.37));
#45343=CARTESIAN_POINT('Ctrl Pts',(-0.535743728280067,0.405371749401093,
5.4));
#45344=CARTESIAN_POINT('Ctrl Pts',(-0.535743728280067,0.405371749401093,
5.37));
#45345=CARTESIAN_POINT('',(-0.611528173089027,0.452080512046814,5.4));
#45346=CARTESIAN_POINT('Ctrl Pts',(-0.611528173089027,0.452080512046814,
5.4));
#45347=CARTESIAN_POINT('Ctrl Pts',(-0.562755838036537,0.440825366973877,
5.4));
#45348=CARTESIAN_POINT('Ctrl Pts',(-0.535743728280067,0.405371749401093,
5.4));
#45349=CARTESIAN_POINT('',(-0.611528173089027,0.452080512046814,5.37));
#45350=CARTESIAN_POINT('',(-0.611528173089027,0.452080512046814,5.4));
#45351=CARTESIAN_POINT('Ctrl Pts',(-0.611528173089027,0.452080512046814,
5.37));
#45352=CARTESIAN_POINT('Ctrl Pts',(-0.562755838036537,0.440825366973877,
5.37));
#45353=CARTESIAN_POINT('Ctrl Pts',(-0.535743728280067,0.405371749401093,
5.37));
#45354=CARTESIAN_POINT('Ctrl Pts',(-0.554877296090126,0.498601639270782,
5.4));
#45355=CARTESIAN_POINT('Ctrl Pts',(-0.554877296090126,0.498601639270782,
5.37));
#45356=CARTESIAN_POINT('Ctrl Pts',(-0.574011102318764,0.469338321685791,
5.4));
#45357=CARTESIAN_POINT('Ctrl Pts',(-0.574011102318764,0.469338321685791,
5.37));
#45358=CARTESIAN_POINT('Ctrl Pts',(-0.611528173089027,0.452080512046814,
5.4));
#45359=CARTESIAN_POINT('Ctrl Pts',(-0.611528173089027,0.452080512046814,
5.37));
#45360=CARTESIAN_POINT('',(-0.554877296090126,0.498601639270782,5.4));
#45361=CARTESIAN_POINT('Ctrl Pts',(-0.554877296090126,0.498601639270782,
5.4));
#45362=CARTESIAN_POINT('Ctrl Pts',(-0.574011102318764,0.469338321685791,
5.4));
#45363=CARTESIAN_POINT('Ctrl Pts',(-0.611528173089027,0.452080512046814,
5.4));
#45364=CARTESIAN_POINT('',(-0.554877296090126,0.498601639270782,5.37));
#45365=CARTESIAN_POINT('',(-0.554877296090126,0.498601639270782,5.4));
#45366=CARTESIAN_POINT('Ctrl Pts',(-0.554877296090126,0.498601639270782,
5.37));
#45367=CARTESIAN_POINT('Ctrl Pts',(-0.574011102318764,0.469338321685791,
5.37));
#45368=CARTESIAN_POINT('Ctrl Pts',(-0.611528173089027,0.452080512046814,
5.37));
#45369=CARTESIAN_POINT('Ctrl Pts',(-0.535743728280067,0.563506150245667,
5.4));
#45370=CARTESIAN_POINT('Ctrl Pts',(-0.535743728280067,0.563506150245667,
5.37));
#45371=CARTESIAN_POINT('Ctrl Pts',(-0.535743728280067,0.527864956855774,
5.4));
#45372=CARTESIAN_POINT('Ctrl Pts',(-0.535743728280067,0.527864956855774,
5.37));
#45373=CARTESIAN_POINT('Ctrl Pts',(-0.554877296090126,0.498601639270782,
5.4));
#45374=CARTESIAN_POINT('Ctrl Pts',(-0.554877296090126,0.498601639270782,
5.37));
#45375=CARTESIAN_POINT('',(-0.535743728280067,0.563506150245667,5.4));
#45376=CARTESIAN_POINT('Ctrl Pts',(-0.535743728280067,0.563506150245667,
5.4));
#45377=CARTESIAN_POINT('Ctrl Pts',(-0.535743728280067,0.527864956855774,
5.4));
#45378=CARTESIAN_POINT('Ctrl Pts',(-0.554877296090126,0.498601639270782,
5.4));
#45379=CARTESIAN_POINT('',(-0.535743728280067,0.563506150245667,5.37));
#45380=CARTESIAN_POINT('',(-0.535743728280067,0.563506150245667,5.4));
#45381=CARTESIAN_POINT('Ctrl Pts',(-0.535743728280067,0.563506150245667,
5.37));
#45382=CARTESIAN_POINT('Ctrl Pts',(-0.535743728280067,0.527864956855774,
5.37));
#45383=CARTESIAN_POINT('Ctrl Pts',(-0.554877296090126,0.498601639270782,
5.37));
#45384=CARTESIAN_POINT('Ctrl Pts',(-0.555815234780312,0.634413385391235,
5.4));
#45385=CARTESIAN_POINT('Ctrl Pts',(-0.555815234780312,0.634413385391235,
5.37));
#45386=CARTESIAN_POINT('Ctrl Pts',(-0.535743728280067,0.601023161411285,
5.4));
#45387=CARTESIAN_POINT('Ctrl Pts',(-0.535743728280067,0.601023161411285,
5.37));
#45388=CARTESIAN_POINT('Ctrl Pts',(-0.535743728280067,0.563506150245667,
5.4));
#45389=CARTESIAN_POINT('Ctrl Pts',(-0.535743728280067,0.563506150245667,
5.37));
#45390=CARTESIAN_POINT('',(-0.555815234780312,0.634413385391235,5.4));
#45391=CARTESIAN_POINT('Ctrl Pts',(-0.555815234780312,0.634413385391235,
5.4));
#45392=CARTESIAN_POINT('Ctrl Pts',(-0.535743728280067,0.601023161411285,
5.4));
#45393=CARTESIAN_POINT('Ctrl Pts',(-0.535743728280067,0.563506150245667,
5.4));
#45394=CARTESIAN_POINT('',(-0.555815234780312,0.634413385391235,5.37));
#45395=CARTESIAN_POINT('',(-0.555815234780312,0.634413385391235,5.4));
#45396=CARTESIAN_POINT('Ctrl Pts',(-0.555815234780312,0.634413385391235,
5.37));
#45397=CARTESIAN_POINT('Ctrl Pts',(-0.535743728280067,0.601023161411285,
5.37));
#45398=CARTESIAN_POINT('Ctrl Pts',(-0.535743728280067,0.563506150245667,
5.37));
#45399=CARTESIAN_POINT('Ctrl Pts',(-0.613779082894325,0.687124812602997,
5.4));
#45400=CARTESIAN_POINT('Ctrl Pts',(-0.613779082894325,0.687124812602997,
5.37));
#45401=CARTESIAN_POINT('Ctrl Pts',(-0.575886741280556,0.667803549766541,
5.4));
#45402=CARTESIAN_POINT('Ctrl Pts',(-0.575886741280556,0.667803549766541,
5.37));
#45403=CARTESIAN_POINT('Ctrl Pts',(-0.555815234780312,0.634413385391235,
5.4));
#45404=CARTESIAN_POINT('Ctrl Pts',(-0.555815234780312,0.634413385391235,
5.37));
#45405=CARTESIAN_POINT('',(-0.613779082894325,0.687124812602997,5.4));
#45406=CARTESIAN_POINT('Ctrl Pts',(-0.613779082894325,0.687124812602997,
5.4));
#45407=CARTESIAN_POINT('Ctrl Pts',(-0.575886741280556,0.667803549766541,
5.4));
#45408=CARTESIAN_POINT('Ctrl Pts',(-0.555815234780312,0.634413385391235,
5.4));
#45409=CARTESIAN_POINT('',(-0.613779082894325,0.687124812602997,5.37));
#45410=CARTESIAN_POINT('',(-0.613779082894325,0.687124812602997,5.4));
#45411=CARTESIAN_POINT('Ctrl Pts',(-0.613779082894325,0.687124812602997,
5.37));
#45412=CARTESIAN_POINT('Ctrl Pts',(-0.575886741280556,0.667803549766541,
5.37));
#45413=CARTESIAN_POINT('Ctrl Pts',(-0.555815234780312,0.634413385391235,
5.37));
#45414=CARTESIAN_POINT('Ctrl Pts',(-0.696691766381264,0.706446135044098,
5.4));
#45415=CARTESIAN_POINT('Ctrl Pts',(-0.696691766381264,0.706446135044098,
5.37));
#45416=CARTESIAN_POINT('Ctrl Pts',(-0.651671424508095,0.706446135044098,
5.4));
#45417=CARTESIAN_POINT('Ctrl Pts',(-0.651671424508095,0.706446135044098,
5.37));
#45418=CARTESIAN_POINT('Ctrl Pts',(-0.613779082894325,0.687124812602997,
5.4));
#45419=CARTESIAN_POINT('Ctrl Pts',(-0.613779082894325,0.687124812602997,
5.37));
#45420=CARTESIAN_POINT('',(-0.696691766381264,0.706446135044098,5.4));
#45421=CARTESIAN_POINT('Ctrl Pts',(-0.696691766381264,0.706446135044098,
5.4));
#45422=CARTESIAN_POINT('Ctrl Pts',(-0.651671424508095,0.706446135044098,
5.4));
#45423=CARTESIAN_POINT('Ctrl Pts',(-0.613779082894325,0.687124812602997,
5.4));
#45424=CARTESIAN_POINT('',(-0.696691766381264,0.706446135044098,5.37));
#45425=CARTESIAN_POINT('',(-0.696691766381264,0.706446135044098,5.4));
#45426=CARTESIAN_POINT('Ctrl Pts',(-0.696691766381264,0.706446135044098,
5.37));
#45427=CARTESIAN_POINT('Ctrl Pts',(-0.651671424508095,0.706446135044098,
5.37));
#45428=CARTESIAN_POINT('Ctrl Pts',(-0.613779082894325,0.687124812602997,
5.37));
#45429=CARTESIAN_POINT('Ctrl Pts',(-0.805866494774818,0.669116640090942,
5.4));
#45430=CARTESIAN_POINT('Ctrl Pts',(-0.805866494774818,0.669116640090942,
5.37));
#45431=CARTESIAN_POINT('Ctrl Pts',(-0.761971488595009,0.706446135044098,
5.4));
#45432=CARTESIAN_POINT('Ctrl Pts',(-0.761971488595009,0.706446135044098,
5.37));
#45433=CARTESIAN_POINT('Ctrl Pts',(-0.696691766381264,0.706446135044098,
5.4));
#45434=CARTESIAN_POINT('Ctrl Pts',(-0.696691766381264,0.706446135044098,
5.37));
#45435=CARTESIAN_POINT('',(-0.805866494774818,0.669116640090942,5.4));
#45436=CARTESIAN_POINT('Ctrl Pts',(-0.805866494774818,0.669116640090942,
5.4));
#45437=CARTESIAN_POINT('Ctrl Pts',(-0.761971488595009,0.706446135044098,
5.4));
#45438=CARTESIAN_POINT('Ctrl Pts',(-0.696691766381264,0.706446135044098,
5.4));
#45439=CARTESIAN_POINT('',(-0.805866494774818,0.669116640090942,5.37));
#45440=CARTESIAN_POINT('',(-0.805866494774818,0.669116640090942,5.4));
#45441=CARTESIAN_POINT('Ctrl Pts',(-0.805866494774818,0.669116640090942,
5.37));
#45442=CARTESIAN_POINT('Ctrl Pts',(-0.761971488595009,0.706446135044098,
5.37));
#45443=CARTESIAN_POINT('Ctrl Pts',(-0.696691766381264,0.706446135044098,
5.37));
#45444=CARTESIAN_POINT('Ctrl Pts',(-0.862142100930214,0.563881301879883,
5.4));
#45445=CARTESIAN_POINT('Ctrl Pts',(-0.862142100930214,0.563881301879883,
5.37));
#45446=CARTESIAN_POINT('Ctrl Pts',(-0.849761500954628,0.631787145137787,
5.4));
#45447=CARTESIAN_POINT('Ctrl Pts',(-0.849761500954628,0.631787145137787,
5.37));
#45448=CARTESIAN_POINT('Ctrl Pts',(-0.805866494774818,0.669116640090942,
5.4));
#45449=CARTESIAN_POINT('Ctrl Pts',(-0.805866494774818,0.669116640090942,
5.37));
#45450=CARTESIAN_POINT('',(-0.862142100930214,0.563881301879883,5.4));
#45451=CARTESIAN_POINT('Ctrl Pts',(-0.862142100930214,0.563881301879883,
5.4));
#45452=CARTESIAN_POINT('Ctrl Pts',(-0.849761500954628,0.631787145137787,
5.4));
#45453=CARTESIAN_POINT('Ctrl Pts',(-0.805866494774818,0.669116640090942,
5.4));
#45454=CARTESIAN_POINT('',(-0.862142100930214,0.563881301879883,5.37));
#45455=CARTESIAN_POINT('',(-0.862142100930214,0.563881301879883,5.4));
#45456=CARTESIAN_POINT('Ctrl Pts',(-0.862142100930214,0.563881301879883,
5.37));
#45457=CARTESIAN_POINT('Ctrl Pts',(-0.849761500954628,0.631787145137787,
5.37));
#45458=CARTESIAN_POINT('Ctrl Pts',(-0.805866494774818,0.669116640090942,
5.37));
#45459=CARTESIAN_POINT('Origin',(-0.794611230492592,0.551875853538513,5.4));
#45460=CARTESIAN_POINT('',(-0.794611230492592,0.551875853538513,5.4));
#45461=CARTESIAN_POINT('',(-0.361925074901606,0.474954124922981,5.4));
#45462=CARTESIAN_POINT('',(-0.794611230492592,0.551875853538513,5.37));
#45463=CARTESIAN_POINT('',(-0.794611230492592,0.551875853538513,5.4));
#45464=CARTESIAN_POINT('',(-0.794611230492592,0.551875853538513,5.37));
#45465=CARTESIAN_POINT('Ctrl Pts',(-0.76084591448307,0.626159632205963,
5.4));
#45466=CARTESIAN_POINT('Ctrl Pts',(-0.76084591448307,0.626159632205963,
5.37));
#45467=CARTESIAN_POINT('Ctrl Pts',(-0.787107959389687,0.601398372650147,
5.4));
#45468=CARTESIAN_POINT('Ctrl Pts',(-0.787107959389687,0.601398372650147,
5.37));
#45469=CARTESIAN_POINT('Ctrl Pts',(-0.794611230492592,0.551875853538513,
5.4));
#45470=CARTESIAN_POINT('Ctrl Pts',(-0.794611230492592,0.551875853538513,
5.37));
#45471=CARTESIAN_POINT('',(-0.76084591448307,0.626159632205963,5.4));
#45472=CARTESIAN_POINT('Ctrl Pts',(-0.76084591448307,0.626159632205963,
5.4));
#45473=CARTESIAN_POINT('Ctrl Pts',(-0.787107959389687,0.601398372650147,
5.4));
#45474=CARTESIAN_POINT('Ctrl Pts',(-0.794611230492592,0.551875853538513,
5.4));
#45475=CARTESIAN_POINT('',(-0.76084591448307,0.626159632205963,5.37));
#45476=CARTESIAN_POINT('',(-0.76084591448307,0.626159632205963,5.4));
#45477=CARTESIAN_POINT('Ctrl Pts',(-0.76084591448307,0.626159632205963,
5.37));
#45478=CARTESIAN_POINT('Ctrl Pts',(-0.787107959389687,0.601398372650147,
5.37));
#45479=CARTESIAN_POINT('Ctrl Pts',(-0.794611230492592,0.551875853538513,
5.37));
#45480=CARTESIAN_POINT('Ctrl Pts',(-0.695191159844398,0.65092089176178,
5.4));
#45481=CARTESIAN_POINT('Ctrl Pts',(-0.695191159844398,0.65092089176178,
5.37));
#45482=CARTESIAN_POINT('Ctrl Pts',(-0.734584107995033,0.65092089176178,
5.4));
#45483=CARTESIAN_POINT('Ctrl Pts',(-0.734584107995033,0.65092089176178,
5.37));
#45484=CARTESIAN_POINT('Ctrl Pts',(-0.76084591448307,0.626159632205963,
5.4));
#45485=CARTESIAN_POINT('Ctrl Pts',(-0.76084591448307,0.626159632205963,
5.37));
#45486=CARTESIAN_POINT('',(-0.695191159844398,0.65092089176178,5.4));
#45487=CARTESIAN_POINT('Ctrl Pts',(-0.695191159844398,0.65092089176178,
5.4));
#45488=CARTESIAN_POINT('Ctrl Pts',(-0.734584107995033,0.65092089176178,
5.4));
#45489=CARTESIAN_POINT('Ctrl Pts',(-0.76084591448307,0.626159632205963,
5.4));
#45490=CARTESIAN_POINT('',(-0.695191159844398,0.65092089176178,5.37));
#45491=CARTESIAN_POINT('',(-0.695191159844398,0.65092089176178,5.4));
#45492=CARTESIAN_POINT('Ctrl Pts',(-0.695191159844398,0.65092089176178,
5.37));
#45493=CARTESIAN_POINT('Ctrl Pts',(-0.734584107995033,0.65092089176178,
5.37));
#45494=CARTESIAN_POINT('Ctrl Pts',(-0.76084591448307,0.626159632205963,
5.37));
#45495=CARTESIAN_POINT('Ctrl Pts',(-0.630286708474159,0.626534783840179,
5.4));
#45496=CARTESIAN_POINT('Ctrl Pts',(-0.630286708474159,0.626534783840179,
5.37));
#45497=CARTESIAN_POINT('Ctrl Pts',(-0.655422940850258,0.65092089176178,
5.4));
#45498=CARTESIAN_POINT('Ctrl Pts',(-0.655422940850258,0.65092089176178,
5.37));
#45499=CARTESIAN_POINT('Ctrl Pts',(-0.695191159844398,0.65092089176178,
5.4));
#45500=CARTESIAN_POINT('Ctrl Pts',(-0.695191159844398,0.65092089176178,
5.37));
#45501=CARTESIAN_POINT('',(-0.630286708474159,0.626534783840179,5.4));
#45502=CARTESIAN_POINT('Ctrl Pts',(-0.630286708474159,0.626534783840179,
5.4));
#45503=CARTESIAN_POINT('Ctrl Pts',(-0.655422940850258,0.65092089176178,
5.4));
#45504=CARTESIAN_POINT('Ctrl Pts',(-0.695191159844398,0.65092089176178,
5.4));
#45505=CARTESIAN_POINT('',(-0.630286708474159,0.626534783840179,5.37));
#45506=CARTESIAN_POINT('',(-0.630286708474159,0.626534783840179,5.4));
#45507=CARTESIAN_POINT('Ctrl Pts',(-0.630286708474159,0.626534783840179,
5.37));
#45508=CARTESIAN_POINT('Ctrl Pts',(-0.655422940850258,0.65092089176178,
5.37));
#45509=CARTESIAN_POINT('Ctrl Pts',(-0.695191159844398,0.65092089176178,
5.37));
#45510=CARTESIAN_POINT('Ctrl Pts',(-0.605150237679482,0.565006816387177,
5.4));
#45511=CARTESIAN_POINT('Ctrl Pts',(-0.605150237679482,0.565006816387177,
5.37));
#45512=CARTESIAN_POINT('Ctrl Pts',(-0.605150237679482,0.602148675918579,
5.4));
#45513=CARTESIAN_POINT('Ctrl Pts',(-0.605150237679482,0.602148675918579,
5.37));
#45514=CARTESIAN_POINT('Ctrl Pts',(-0.630286708474159,0.626534783840179,
5.4));
#45515=CARTESIAN_POINT('Ctrl Pts',(-0.630286708474159,0.626534783840179,
5.37));
#45516=CARTESIAN_POINT('',(-0.605150237679482,0.565006816387177,5.4));
#45517=CARTESIAN_POINT('Ctrl Pts',(-0.605150237679482,0.565006816387177,
5.4));
#45518=CARTESIAN_POINT('Ctrl Pts',(-0.605150237679482,0.602148675918579,
5.4));
#45519=CARTESIAN_POINT('Ctrl Pts',(-0.630286708474159,0.626534783840179,
5.4));
#45520=CARTESIAN_POINT('',(-0.605150237679482,0.565006816387177,5.37));
#45521=CARTESIAN_POINT('',(-0.605150237679482,0.565006816387177,5.4));
#45522=CARTESIAN_POINT('Ctrl Pts',(-0.605150237679482,0.565006816387177,
5.37));
#45523=CARTESIAN_POINT('Ctrl Pts',(-0.605150237679482,0.602148675918579,
5.37));
#45524=CARTESIAN_POINT('Ctrl Pts',(-0.630286708474159,0.626534783840179,
5.37));
#45525=CARTESIAN_POINT('Ctrl Pts',(-0.639665856957436,0.495600247383118,
5.4));
#45526=CARTESIAN_POINT('Ctrl Pts',(-0.639665856957436,0.495600247383118,
5.37));
#45527=CARTESIAN_POINT('Ctrl Pts',(-0.605150237679482,0.518110477924347,
5.4));
#45528=CARTESIAN_POINT('Ctrl Pts',(-0.605150237679482,0.518110477924347,
5.37));
#45529=CARTESIAN_POINT('Ctrl Pts',(-0.605150237679482,0.565006816387177,
5.4));
#45530=CARTESIAN_POINT('Ctrl Pts',(-0.605150237679482,0.565006816387177,
5.37));
#45531=CARTESIAN_POINT('',(-0.639665856957436,0.495600247383118,5.4));
#45532=CARTESIAN_POINT('Ctrl Pts',(-0.639665856957436,0.495600247383118,
5.4));
#45533=CARTESIAN_POINT('Ctrl Pts',(-0.605150237679482,0.518110477924347,
5.4));
#45534=CARTESIAN_POINT('Ctrl Pts',(-0.605150237679482,0.565006816387177,
5.4));
#45535=CARTESIAN_POINT('',(-0.639665856957436,0.495600247383118,5.37));
#45536=CARTESIAN_POINT('',(-0.639665856957436,0.495600247383118,5.4));
#45537=CARTESIAN_POINT('Ctrl Pts',(-0.639665856957436,0.495600247383118,
5.37));
#45538=CARTESIAN_POINT('Ctrl Pts',(-0.605150237679482,0.518110477924347,
5.37));
#45539=CARTESIAN_POINT('Ctrl Pts',(-0.605150237679482,0.565006816387177,
5.37));
#45540=CARTESIAN_POINT('Ctrl Pts',(-0.717326179146767,0.473090016841888,
5.4));
#45541=CARTESIAN_POINT('Ctrl Pts',(-0.717326179146767,0.473090016841888,
5.37));
#45542=CARTESIAN_POINT('Ctrl Pts',(-0.67418147623539,0.473090016841888,
5.4));
#45543=CARTESIAN_POINT('Ctrl Pts',(-0.67418147623539,0.473090016841888,
5.37));
#45544=CARTESIAN_POINT('Ctrl Pts',(-0.639665856957436,0.495600247383118,
5.4));
#45545=CARTESIAN_POINT('Ctrl Pts',(-0.639665856957436,0.495600247383118,
5.37));
#45546=CARTESIAN_POINT('',(-0.717326179146767,0.473090016841888,5.4));
#45547=CARTESIAN_POINT('Ctrl Pts',(-0.717326179146767,0.473090016841888,
5.4));
#45548=CARTESIAN_POINT('Ctrl Pts',(-0.67418147623539,0.473090016841888,
5.4));
#45549=CARTESIAN_POINT('Ctrl Pts',(-0.639665856957436,0.495600247383118,
5.4));
#45550=CARTESIAN_POINT('',(-0.717326179146767,0.473090016841888,5.37));
#45551=CARTESIAN_POINT('',(-0.717326179146767,0.473090016841888,5.4));
#45552=CARTESIAN_POINT('Ctrl Pts',(-0.717326179146767,0.473090016841888,
5.37));
#45553=CARTESIAN_POINT('Ctrl Pts',(-0.67418147623539,0.473090016841888,
5.37));
#45554=CARTESIAN_POINT('Ctrl Pts',(-0.639665856957436,0.495600247383118,
5.37));
#45555=CARTESIAN_POINT('Ctrl Pts',(-0.728206172585487,0.473840379714966,
5.4));
#45556=CARTESIAN_POINT('Ctrl Pts',(-0.728206172585487,0.473840379714966,
5.37));
#45557=CARTESIAN_POINT('Ctrl Pts',(-0.721452966332436,0.473090016841888,
5.4));
#45558=CARTESIAN_POINT('Ctrl Pts',(-0.721452966332436,0.473090016841888,
5.37));
#45559=CARTESIAN_POINT('Ctrl Pts',(-0.717326179146767,0.473090016841888,
5.4));
#45560=CARTESIAN_POINT('Ctrl Pts',(-0.717326179146767,0.473090016841888,
5.37));
#45561=CARTESIAN_POINT('',(-0.728206172585487,0.473840379714966,5.4));
#45562=CARTESIAN_POINT('Ctrl Pts',(-0.728206172585487,0.473840379714966,
5.4));
#45563=CARTESIAN_POINT('Ctrl Pts',(-0.721452966332436,0.473090016841888,
5.4));
#45564=CARTESIAN_POINT('Ctrl Pts',(-0.717326179146767,0.473090016841888,
5.4));
#45565=CARTESIAN_POINT('',(-0.728206172585487,0.473840379714966,5.37));
#45566=CARTESIAN_POINT('',(-0.728206172585487,0.473840379714966,5.4));
#45567=CARTESIAN_POINT('Ctrl Pts',(-0.728206172585487,0.473840379714966,
5.37));
#45568=CARTESIAN_POINT('Ctrl Pts',(-0.721452966332436,0.473090016841888,
5.37));
#45569=CARTESIAN_POINT('Ctrl Pts',(-0.717326179146767,0.473090016841888,
5.37));
#45570=CARTESIAN_POINT('Origin',(-0.735709443688393,0.41456344127655,5.4));
#45571=CARTESIAN_POINT('',(-0.735709443688393,0.41456344127655,5.4));
#45572=CARTESIAN_POINT('',(-0.755732388442078,0.256379251042444,5.4));
#45573=CARTESIAN_POINT('',(-0.735709443688393,0.41456344127655,5.37));
#45574=CARTESIAN_POINT('',(-0.735709443688393,0.41456344127655,5.4));
#45575=CARTESIAN_POINT('',(-0.735709443688393,0.41456344127655,5.37));
#45576=CARTESIAN_POINT('Ctrl Pts',(-0.68806292116642,0.422066831588745,
5.4));
#45577=CARTESIAN_POINT('Ctrl Pts',(-0.68806292116642,0.422066831588745,
5.37));
#45578=CARTESIAN_POINT('Ctrl Pts',(-0.707196488976479,0.422066831588745,
5.4));
#45579=CARTESIAN_POINT('Ctrl Pts',(-0.707196488976479,0.422066831588745,
5.37));
#45580=CARTESIAN_POINT('Ctrl Pts',(-0.735709443688393,0.41456344127655,
5.4));
#45581=CARTESIAN_POINT('Ctrl Pts',(-0.735709443688393,0.41456344127655,
5.37));
#45582=CARTESIAN_POINT('',(-0.68806292116642,0.422066831588745,5.4));
#45583=CARTESIAN_POINT('Ctrl Pts',(-0.68806292116642,0.422066831588745,
5.4));
#45584=CARTESIAN_POINT('Ctrl Pts',(-0.707196488976479,0.422066831588745,
5.4));
#45585=CARTESIAN_POINT('Ctrl Pts',(-0.735709443688393,0.41456344127655,
5.4));
#45586=CARTESIAN_POINT('',(-0.68806292116642,0.422066831588745,5.37));
#45587=CARTESIAN_POINT('',(-0.68806292116642,0.422066831588745,5.4));
#45588=CARTESIAN_POINT('Ctrl Pts',(-0.68806292116642,0.422066831588745,
5.37));
#45589=CARTESIAN_POINT('Ctrl Pts',(-0.707196488976479,0.422066831588745,
5.37));
#45590=CARTESIAN_POINT('Ctrl Pts',(-0.735709443688393,0.41456344127655,
5.37));
#45591=CARTESIAN_POINT('Ctrl Pts',(-0.610777631402016,0.391865620017052,
5.4));
#45592=CARTESIAN_POINT('Ctrl Pts',(-0.610777631402016,0.391865620017052,
5.37));
#45593=CARTESIAN_POINT('Ctrl Pts',(-0.641166463494301,0.422066831588745,
5.4));
#45594=CARTESIAN_POINT('Ctrl Pts',(-0.641166463494301,0.422066831588745,
5.37));
#45595=CARTESIAN_POINT('Ctrl Pts',(-0.68806292116642,0.422066831588745,
5.4));
#45596=CARTESIAN_POINT('Ctrl Pts',(-0.68806292116642,0.422066831588745,
5.37));
#45597=CARTESIAN_POINT('',(-0.610777631402016,0.391865620017052,5.4));
#45598=CARTESIAN_POINT('Ctrl Pts',(-0.610777631402016,0.391865620017052,
5.4));
#45599=CARTESIAN_POINT('Ctrl Pts',(-0.641166463494301,0.422066831588745,
5.4));
#45600=CARTESIAN_POINT('Ctrl Pts',(-0.68806292116642,0.422066831588745,
5.4));
#45601=CARTESIAN_POINT('',(-0.610777631402016,0.391865620017052,5.37));
#45602=CARTESIAN_POINT('',(-0.610777631402016,0.391865620017052,5.4));
#45603=CARTESIAN_POINT('Ctrl Pts',(-0.610777631402016,0.391865620017052,
5.37));
#45604=CARTESIAN_POINT('Ctrl Pts',(-0.641166463494301,0.422066831588745,
5.37));
#45605=CARTESIAN_POINT('Ctrl Pts',(-0.68806292116642,0.422066831588745,
5.37));
#45606=CARTESIAN_POINT('Ctrl Pts',(-0.58038903772831,0.315143251419067,
5.4));
#45607=CARTESIAN_POINT('Ctrl Pts',(-0.58038903772831,0.315143251419067,
5.37));
#45608=CARTESIAN_POINT('Ctrl Pts',(-0.58038903772831,0.361664393544197,
5.4));
#45609=CARTESIAN_POINT('Ctrl Pts',(-0.58038903772831,0.361664393544197,
5.37));
#45610=CARTESIAN_POINT('Ctrl Pts',(-0.610777631402016,0.391865620017052,
5.4));
#45611=CARTESIAN_POINT('Ctrl Pts',(-0.610777631402016,0.391865620017052,
5.37));
#45612=CARTESIAN_POINT('',(-0.58038903772831,0.315143251419067,5.4));
#45613=CARTESIAN_POINT('Ctrl Pts',(-0.58038903772831,0.315143251419067,
5.4));
#45614=CARTESIAN_POINT('Ctrl Pts',(-0.58038903772831,0.361664393544197,
5.4));
#45615=CARTESIAN_POINT('Ctrl Pts',(-0.610777631402016,0.391865620017052,
5.4));
#45616=CARTESIAN_POINT('',(-0.58038903772831,0.315143251419067,5.37));
#45617=CARTESIAN_POINT('',(-0.58038903772831,0.315143251419067,5.4));
#45618=CARTESIAN_POINT('Ctrl Pts',(-0.58038903772831,0.315143251419067,
5.37));
#45619=CARTESIAN_POINT('Ctrl Pts',(-0.58038903772831,0.361664393544197,
5.37));
#45620=CARTESIAN_POINT('Ctrl Pts',(-0.610777631402016,0.391865620017052,
5.37));
#45621=CARTESIAN_POINT('Ctrl Pts',(-0.613216415047646,0.233356082439423,
5.4));
#45622=CARTESIAN_POINT('Ctrl Pts',(-0.613216415047646,0.233356082439423,
5.37));
#45623=CARTESIAN_POINT('Ctrl Pts',(-0.58038903772831,0.266371095180511,
5.4));
#45624=CARTESIAN_POINT('Ctrl Pts',(-0.58038903772831,0.266371095180511,
5.37));
#45625=CARTESIAN_POINT('Ctrl Pts',(-0.58038903772831,0.315143251419067,
5.4));
#45626=CARTESIAN_POINT('Ctrl Pts',(-0.58038903772831,0.315143251419067,
5.37));
#45627=CARTESIAN_POINT('',(-0.613216415047646,0.233356082439423,5.4));
#45628=CARTESIAN_POINT('Ctrl Pts',(-0.613216415047646,0.233356082439423,
5.4));
#45629=CARTESIAN_POINT('Ctrl Pts',(-0.58038903772831,0.266371095180511,
5.4));
#45630=CARTESIAN_POINT('Ctrl Pts',(-0.58038903772831,0.315143251419067,
5.4));
#45631=CARTESIAN_POINT('',(-0.613216415047646,0.233356082439423,5.37));
#45632=CARTESIAN_POINT('',(-0.613216415047646,0.233356082439423,5.4));
#45633=CARTESIAN_POINT('Ctrl Pts',(-0.613216415047646,0.233356082439423,
5.37));
#45634=CARTESIAN_POINT('Ctrl Pts',(-0.58038903772831,0.266371095180511,
5.37));
#45635=CARTESIAN_POINT('Ctrl Pts',(-0.58038903772831,0.315143251419067,
5.37));
#45636=CARTESIAN_POINT('Ctrl Pts',(-0.693690314888954,0.200341069698334,
5.4));
#45637=CARTESIAN_POINT('Ctrl Pts',(-0.693690314888954,0.200341069698334,
5.37));
#45638=CARTESIAN_POINT('Ctrl Pts',(-0.646043792366982,0.200341069698334,
5.4));
#45639=CARTESIAN_POINT('Ctrl Pts',(-0.646043792366982,0.200341069698334,
5.37));
#45640=CARTESIAN_POINT('Ctrl Pts',(-0.613216415047646,0.233356082439423,
5.4));
#45641=CARTESIAN_POINT('Ctrl Pts',(-0.613216415047646,0.233356082439423,
5.37));
#45642=CARTESIAN_POINT('',(-0.693690314888954,0.200341069698334,5.4));
#45643=CARTESIAN_POINT('Ctrl Pts',(-0.693690314888954,0.200341069698334,
5.4));
#45644=CARTESIAN_POINT('Ctrl Pts',(-0.646043792366982,0.200341069698334,
5.4));
#45645=CARTESIAN_POINT('Ctrl Pts',(-0.613216415047646,0.233356082439423,
5.4));
#45646=CARTESIAN_POINT('',(-0.693690314888954,0.200341069698334,5.37));
#45647=CARTESIAN_POINT('',(-0.693690314888954,0.200341069698334,5.4));
#45648=CARTESIAN_POINT('Ctrl Pts',(-0.693690314888954,0.200341069698334,
5.37));
#45649=CARTESIAN_POINT('Ctrl Pts',(-0.646043792366982,0.200341069698334,
5.37));
#45650=CARTESIAN_POINT('Ctrl Pts',(-0.613216415047646,0.233356082439423,
5.37));
#45651=CARTESIAN_POINT('Ctrl Pts',(-0.761783853173256,0.225665086507797,
5.4));
#45652=CARTESIAN_POINT('Ctrl Pts',(-0.761783853173256,0.225665086507797,
5.37));
#45653=CARTESIAN_POINT('Ctrl Pts',(-0.733833566308022,0.200341069698334,
5.4));
#45654=CARTESIAN_POINT('Ctrl Pts',(-0.733833566308022,0.200341069698334,
5.37));
#45655=CARTESIAN_POINT('Ctrl Pts',(-0.693690314888954,0.200341069698334,
5.4));
#45656=CARTESIAN_POINT('Ctrl Pts',(-0.693690314888954,0.200341069698334,
5.37));
#45657=CARTESIAN_POINT('',(-0.761783853173256,0.225665086507797,5.4));
#45658=CARTESIAN_POINT('Ctrl Pts',(-0.761783853173256,0.225665086507797,
5.4));
#45659=CARTESIAN_POINT('Ctrl Pts',(-0.733833566308022,0.200341069698334,
5.4));
#45660=CARTESIAN_POINT('Ctrl Pts',(-0.693690314888954,0.200341069698334,
5.4));
#45661=CARTESIAN_POINT('',(-0.761783853173256,0.225665086507797,5.37));
#45662=CARTESIAN_POINT('',(-0.761783853173256,0.225665086507797,5.4));
#45663=CARTESIAN_POINT('Ctrl Pts',(-0.761783853173256,0.225665086507797,
5.37));
#45664=CARTESIAN_POINT('Ctrl Pts',(-0.733833566308022,0.200341069698334,
5.37));
#45665=CARTESIAN_POINT('Ctrl Pts',(-0.693690314888954,0.200341069698334,
5.37));
#45666=CARTESIAN_POINT('Ctrl Pts',(-0.801364436745644,0.308390179276466,
5.4));
#45667=CARTESIAN_POINT('Ctrl Pts',(-0.801364436745644,0.308390179276466,
5.37));
#45668=CARTESIAN_POINT('Ctrl Pts',(-0.78973414003849,0.250989103317261,
5.4));
#45669=CARTESIAN_POINT('Ctrl Pts',(-0.78973414003849,0.250989103317261,
5.37));
#45670=CARTESIAN_POINT('Ctrl Pts',(-0.761783853173256,0.225665086507797,
5.4));
#45671=CARTESIAN_POINT('Ctrl Pts',(-0.761783853173256,0.225665086507797,
5.37));
#45672=CARTESIAN_POINT('',(-0.801364436745644,0.308390179276466,5.4));
#45673=CARTESIAN_POINT('Ctrl Pts',(-0.801364436745644,0.308390179276466,
5.4));
#45674=CARTESIAN_POINT('Ctrl Pts',(-0.78973414003849,0.250989103317261,
5.4));
#45675=CARTESIAN_POINT('Ctrl Pts',(-0.761783853173256,0.225665086507797,
5.4));
#45676=CARTESIAN_POINT('',(-0.801364436745644,0.308390179276466,5.37));
#45677=CARTESIAN_POINT('',(-0.801364436745644,0.308390179276466,5.4));
#45678=CARTESIAN_POINT('Ctrl Pts',(-0.801364436745644,0.308390179276466,
5.37));
#45679=CARTESIAN_POINT('Ctrl Pts',(-0.78973414003849,0.250989103317261,
5.37));
#45680=CARTESIAN_POINT('Ctrl Pts',(-0.761783853173256,0.225665086507797,
5.37));
#45681=CARTESIAN_POINT('Origin',(-0.868895068764687,0.299386093020439,5.4));
#45682=CARTESIAN_POINT('',(-0.868895068764687,0.299386093020439,5.4));
#45683=CARTESIAN_POINT('',(-0.461646587843761,0.353685902458237,5.4));
#45684=CARTESIAN_POINT('',(-0.868895068764687,0.299386093020439,5.37));
#45685=CARTESIAN_POINT('',(-0.868895068764687,0.299386093020439,5.4));
#45686=CARTESIAN_POINT('',(-0.868895068764687,0.299386093020439,5.37));
#45687=CARTESIAN_POINT('Ctrl Pts',(-0.814307704567909,0.187585258483887,
5.4));
#45688=CARTESIAN_POINT('Ctrl Pts',(-0.814307704567909,0.187585258483887,
5.37));
#45689=CARTESIAN_POINT('Ctrl Pts',(-0.862142100930214,0.230729871988297,
5.4));
#45690=CARTESIAN_POINT('Ctrl Pts',(-0.862142100930214,0.230729871988297,
5.37));
#45691=CARTESIAN_POINT('Ctrl Pts',(-0.868895068764687,0.299386093020439,
5.4));
#45692=CARTESIAN_POINT('Ctrl Pts',(-0.868895068764687,0.299386093020439,
5.37));
#45693=CARTESIAN_POINT('',(-0.814307704567909,0.187585258483887,5.4));
#45694=CARTESIAN_POINT('Ctrl Pts',(-0.814307704567909,0.187585258483887,
5.4));
#45695=CARTESIAN_POINT('Ctrl Pts',(-0.862142100930214,0.230729871988297,
5.4));
#45696=CARTESIAN_POINT('Ctrl Pts',(-0.868895068764687,0.299386093020439,
5.4));
#45697=CARTESIAN_POINT('',(-0.814307704567909,0.187585258483887,5.37));
#45698=CARTESIAN_POINT('',(-0.814307704567909,0.187585258483887,5.4));
#45699=CARTESIAN_POINT('Ctrl Pts',(-0.814307704567909,0.187585258483887,
5.37));
#45700=CARTESIAN_POINT('Ctrl Pts',(-0.862142100930214,0.230729871988297,
5.37));
#45701=CARTESIAN_POINT('Ctrl Pts',(-0.868895068764687,0.299386093020439,
5.37));
#45702=CARTESIAN_POINT('Ctrl Pts',(-0.69406558573246,0.144440674781799,
5.4));
#45703=CARTESIAN_POINT('Ctrl Pts',(-0.69406558573246,0.144440674781799,
5.37));
#45704=CARTESIAN_POINT('Ctrl Pts',(-0.766473546624184,0.144440674781799,
5.4));
#45705=CARTESIAN_POINT('Ctrl Pts',(-0.766473546624184,0.144440674781799,
5.37));
#45706=CARTESIAN_POINT('Ctrl Pts',(-0.814307704567909,0.187585258483887,
5.4));
#45707=CARTESIAN_POINT('Ctrl Pts',(-0.814307704567909,0.187585258483887,
5.37));
#45708=CARTESIAN_POINT('Ctrl Pts',(-0.69406558573246,0.144440674781799,
5.4));
#45709=CARTESIAN_POINT('Ctrl Pts',(-0.766473546624184,0.144440674781799,
5.4));
#45710=CARTESIAN_POINT('Ctrl Pts',(-0.814307704567909,0.187585258483887,
5.4));
#45711=CARTESIAN_POINT('Ctrl Pts',(-0.69406558573246,0.144440674781799,
5.37));
#45712=CARTESIAN_POINT('Ctrl Pts',(-0.766473546624184,0.144440674781799,
5.37));
#45713=CARTESIAN_POINT('Ctrl Pts',(-0.814307704567909,0.187585258483887,
5.37));
#45714=CARTESIAN_POINT('Origin',(-0.688813224434853,0.425443404912949,5.37));
#45715=CARTESIAN_POINT('Ctrl Pts',(0.177080616354942,0.324897700548172,
5.4));
#45716=CARTESIAN_POINT('Ctrl Pts',(0.177080616354942,0.324897700548172,
5.37));
#45717=CARTESIAN_POINT('Ctrl Pts',(0.116302952170372,0.273874485492706,
5.4));
#45718=CARTESIAN_POINT('Ctrl Pts',(0.116302952170372,0.273874485492706,
5.37));
#45719=CARTESIAN_POINT('Ctrl Pts',(0.0990450233221054,0.255678737163544,
5.4));
#45720=CARTESIAN_POINT('Ctrl Pts',(0.0990450233221054,0.255678737163544,
5.37));
#45721=CARTESIAN_POINT('',(0.177080616354942,0.324897700548172,5.4));
#45722=CARTESIAN_POINT('',(0.0990450233221054,0.255678737163544,5.4));
#45723=CARTESIAN_POINT('Ctrl Pts',(0.177080616354942,0.324897700548172,
5.4));
#45724=CARTESIAN_POINT('Ctrl Pts',(0.116302952170372,0.273874485492706,
5.4));
#45725=CARTESIAN_POINT('Ctrl Pts',(0.0990450233221054,0.255678737163544,
5.4));
#45726=CARTESIAN_POINT('',(0.177080616354942,0.324897700548172,5.37));
#45727=CARTESIAN_POINT('',(0.177080616354942,0.324897700548172,5.4));
#45728=CARTESIAN_POINT('',(0.0990450233221054,0.255678737163544,5.37));
#45729=CARTESIAN_POINT('Ctrl Pts',(0.177080616354942,0.324897700548172,
5.37));
#45730=CARTESIAN_POINT('Ctrl Pts',(0.116302952170372,0.273874485492706,
5.37));
#45731=CARTESIAN_POINT('Ctrl Pts',(0.0990450233221054,0.255678737163544,
5.37));
#45732=CARTESIAN_POINT('',(0.0990450233221054,0.255678737163544,5.4));
#45733=CARTESIAN_POINT('Ctrl Pts',(0.281190380454063,0.421691709756851,
5.4));
#45734=CARTESIAN_POINT('Ctrl Pts',(0.281190380454063,0.421691709756851,
5.37));
#45735=CARTESIAN_POINT('Ctrl Pts',(0.249863609671593,0.386425668001175,
5.4));
#45736=CARTESIAN_POINT('Ctrl Pts',(0.249863609671593,0.386425668001175,
5.37));
#45737=CARTESIAN_POINT('Ctrl Pts',(0.177080616354942,0.324897700548172,
5.4));
#45738=CARTESIAN_POINT('Ctrl Pts',(0.177080616354942,0.324897700548172,
5.37));
#45739=CARTESIAN_POINT('',(0.281190380454063,0.421691709756851,5.4));
#45740=CARTESIAN_POINT('Ctrl Pts',(0.281190380454063,0.421691709756851,
5.4));
#45741=CARTESIAN_POINT('Ctrl Pts',(0.249863609671593,0.386425668001175,
5.4));
#45742=CARTESIAN_POINT('Ctrl Pts',(0.177080616354942,0.324897700548172,
5.4));
#45743=CARTESIAN_POINT('',(0.281190380454063,0.421691709756851,5.37));
#45744=CARTESIAN_POINT('',(0.281190380454063,0.421691709756851,5.4));
#45745=CARTESIAN_POINT('Ctrl Pts',(0.281190380454063,0.421691709756851,
5.37));
#45746=CARTESIAN_POINT('Ctrl Pts',(0.249863609671593,0.386425668001175,
5.37));
#45747=CARTESIAN_POINT('Ctrl Pts',(0.177080616354942,0.324897700548172,
5.37));
#45748=CARTESIAN_POINT('Ctrl Pts',(0.326023086905479,0.488847219944,5.4));
#45749=CARTESIAN_POINT('Ctrl Pts',(0.326023086905479,0.488847219944,5.37));
#45750=CARTESIAN_POINT('Ctrl Pts',(0.312517151236534,0.456957721710205,
5.4));
#45751=CARTESIAN_POINT('Ctrl Pts',(0.312517151236534,0.456957721710205,
5.37));
#45752=CARTESIAN_POINT('Ctrl Pts',(0.281190380454063,0.421691709756851,
5.4));
#45753=CARTESIAN_POINT('Ctrl Pts',(0.281190380454063,0.421691709756851,
5.37));
#45754=CARTESIAN_POINT('',(0.326023086905479,0.488847219944,5.4));
#45755=CARTESIAN_POINT('Ctrl Pts',(0.326023086905479,0.488847219944,5.4));
#45756=CARTESIAN_POINT('Ctrl Pts',(0.312517151236534,0.456957721710205,
5.4));
#45757=CARTESIAN_POINT('Ctrl Pts',(0.281190380454063,0.421691709756851,
5.4));
#45758=CARTESIAN_POINT('',(0.326023086905479,0.488847219944,5.37));
#45759=CARTESIAN_POINT('',(0.326023086905479,0.488847219944,5.4));
#45760=CARTESIAN_POINT('Ctrl Pts',(0.326023086905479,0.488847219944,5.37));
#45761=CARTESIAN_POINT('Ctrl Pts',(0.312517151236534,0.456957721710205,
5.37));
#45762=CARTESIAN_POINT('Ctrl Pts',(0.281190380454063,0.421691709756851,
5.37));
#45763=CARTESIAN_POINT('Ctrl Pts',(0.339529260993004,0.553751730918884,
5.4));
#45764=CARTESIAN_POINT('Ctrl Pts',(0.339529260993004,0.553751730918884,
5.37));
#45765=CARTESIAN_POINT('Ctrl Pts',(0.339529260993004,0.520736718177795,
5.4));
#45766=CARTESIAN_POINT('Ctrl Pts',(0.339529260993004,0.520736718177795,
5.37));
#45767=CARTESIAN_POINT('Ctrl Pts',(0.326023086905479,0.488847219944,5.4));
#45768=CARTESIAN_POINT('Ctrl Pts',(0.326023086905479,0.488847219944,5.37));
#45769=CARTESIAN_POINT('',(0.339529260993004,0.553751730918884,5.4));
#45770=CARTESIAN_POINT('Ctrl Pts',(0.339529260993004,0.553751730918884,
5.4));
#45771=CARTESIAN_POINT('Ctrl Pts',(0.339529260993004,0.520736718177795,
5.4));
#45772=CARTESIAN_POINT('Ctrl Pts',(0.326023086905479,0.488847219944,5.4));
#45773=CARTESIAN_POINT('',(0.339529260993004,0.553751730918884,5.37));
#45774=CARTESIAN_POINT('',(0.339529260993004,0.553751730918884,5.4));
#45775=CARTESIAN_POINT('Ctrl Pts',(0.339529260993004,0.553751730918884,
5.37));
#45776=CARTESIAN_POINT('Ctrl Pts',(0.339529260993004,0.520736718177795,
5.37));
#45777=CARTESIAN_POINT('Ctrl Pts',(0.326023086905479,0.488847219944,5.37));
#45778=CARTESIAN_POINT('Ctrl Pts',(0.293383345007896,0.662551188468933,
5.4));
#45779=CARTESIAN_POINT('Ctrl Pts',(0.293383345007896,0.662551188468933,
5.37));
#45780=CARTESIAN_POINT('Ctrl Pts',(0.339529260993004,0.618656241893768,
5.4));
#45781=CARTESIAN_POINT('Ctrl Pts',(0.339529260993004,0.618656241893768,
5.37));
#45782=CARTESIAN_POINT('Ctrl Pts',(0.339529260993004,0.553751730918884,
5.4));
#45783=CARTESIAN_POINT('Ctrl Pts',(0.339529260993004,0.553751730918884,
5.37));
#45784=CARTESIAN_POINT('',(0.293383345007896,0.662551188468933,5.4));
#45785=CARTESIAN_POINT('Ctrl Pts',(0.293383345007896,0.662551188468933,
5.4));
#45786=CARTESIAN_POINT('Ctrl Pts',(0.339529260993004,0.618656241893768,
5.4));
#45787=CARTESIAN_POINT('Ctrl Pts',(0.339529260993004,0.553751730918884,
5.4));
#45788=CARTESIAN_POINT('',(0.293383345007896,0.662551188468933,5.37));
#45789=CARTESIAN_POINT('',(0.293383345007896,0.662551188468933,5.4));
#45790=CARTESIAN_POINT('Ctrl Pts',(0.293383345007896,0.662551188468933,
5.37));
#45791=CARTESIAN_POINT('Ctrl Pts',(0.339529260993004,0.618656241893768,
5.37));
#45792=CARTESIAN_POINT('Ctrl Pts',(0.339529260993004,0.553751730918884,
5.37));
#45793=CARTESIAN_POINT('Ctrl Pts',(0.168076500296593,0.706446135044098,
5.4));
#45794=CARTESIAN_POINT('Ctrl Pts',(0.168076500296593,0.706446135044098,
5.37));
#45795=CARTESIAN_POINT('Ctrl Pts',(0.247237429022789,0.706446135044098,
5.4));
#45796=CARTESIAN_POINT('Ctrl Pts',(0.247237429022789,0.706446135044098,
5.37));
#45797=CARTESIAN_POINT('Ctrl Pts',(0.293383345007896,0.662551188468933,
5.4));
#45798=CARTESIAN_POINT('Ctrl Pts',(0.293383345007896,0.662551188468933,
5.37));
#45799=CARTESIAN_POINT('',(0.168076500296593,0.706446135044098,5.4));
#45800=CARTESIAN_POINT('Ctrl Pts',(0.168076500296593,0.706446135044098,
5.4));
#45801=CARTESIAN_POINT('Ctrl Pts',(0.247237429022789,0.706446135044098,
5.4));
#45802=CARTESIAN_POINT('Ctrl Pts',(0.293383345007896,0.662551188468933,
5.4));
#45803=CARTESIAN_POINT('',(0.168076500296593,0.706446135044098,5.37));
#45804=CARTESIAN_POINT('',(0.168076500296593,0.706446135044098,5.4));
#45805=CARTESIAN_POINT('Ctrl Pts',(0.168076500296593,0.706446135044098,
5.37));
#45806=CARTESIAN_POINT('Ctrl Pts',(0.247237429022789,0.706446135044098,
5.37));
#45807=CARTESIAN_POINT('Ctrl Pts',(0.293383345007896,0.662551188468933,
5.37));
#45808=CARTESIAN_POINT('Ctrl Pts',(0.0431446880102158,0.665740156173706,
5.4));
#45809=CARTESIAN_POINT('Ctrl Pts',(0.0431446880102158,0.665740156173706,
5.37));
#45810=CARTESIAN_POINT('Ctrl Pts',(0.089665874838829,0.706446135044098,
5.4));
#45811=CARTESIAN_POINT('Ctrl Pts',(0.089665874838829,0.706446135044098,
5.37));
#45812=CARTESIAN_POINT('Ctrl Pts',(0.168076500296593,0.706446135044098,
5.4));
#45813=CARTESIAN_POINT('Ctrl Pts',(0.168076500296593,0.706446135044098,
5.37));
#45814=CARTESIAN_POINT('',(0.0431446880102158,0.665740156173706,5.4));
#45815=CARTESIAN_POINT('Ctrl Pts',(0.0431446880102158,0.665740156173706,
5.4));
#45816=CARTESIAN_POINT('Ctrl Pts',(0.089665874838829,0.706446135044098,
5.4));
#45817=CARTESIAN_POINT('Ctrl Pts',(0.168076500296593,0.706446135044098,
5.4));
#45818=CARTESIAN_POINT('',(0.0431446880102158,0.665740156173706,5.37));
#45819=CARTESIAN_POINT('',(0.0431446880102158,0.665740156173706,5.4));
#45820=CARTESIAN_POINT('Ctrl Pts',(0.0431446880102158,0.665740156173706,
5.37));
#45821=CARTESIAN_POINT('Ctrl Pts',(0.089665874838829,0.706446135044098,
5.37));
#45822=CARTESIAN_POINT('Ctrl Pts',(0.168076500296593,0.706446135044098,
5.37));
#45823=CARTESIAN_POINT('Ctrl Pts',(-0.010504737496376,0.547373825311661,
5.4));
#45824=CARTESIAN_POINT('Ctrl Pts',(-0.010504737496376,0.547373825311661,
5.37));
#45825=CARTESIAN_POINT('Ctrl Pts',(-0.00337649881839752,0.625034147500992,
5.4));
#45826=CARTESIAN_POINT('Ctrl Pts',(-0.00337649881839752,0.625034147500992,
5.37));
#45827=CARTESIAN_POINT('Ctrl Pts',(0.0431446880102158,0.665740156173706,
5.4));
#45828=CARTESIAN_POINT('Ctrl Pts',(0.0431446880102158,0.665740156173706,
5.37));
#45829=CARTESIAN_POINT('',(-0.010504737496376,0.547373825311661,5.4));
#45830=CARTESIAN_POINT('Ctrl Pts',(-0.010504737496376,0.547373825311661,
5.4));
#45831=CARTESIAN_POINT('Ctrl Pts',(-0.00337649881839752,0.625034147500992,
5.4));
#45832=CARTESIAN_POINT('Ctrl Pts',(0.0431446880102158,0.665740156173706,
5.4));
#45833=CARTESIAN_POINT('',(-0.010504737496376,0.547373825311661,5.37));
#45834=CARTESIAN_POINT('',(-0.010504737496376,0.547373825311661,5.4));
#45835=CARTESIAN_POINT('Ctrl Pts',(-0.010504737496376,0.547373825311661,
5.37));
#45836=CARTESIAN_POINT('Ctrl Pts',(-0.00337649881839752,0.625034147500992,
5.37));
#45837=CARTESIAN_POINT('Ctrl Pts',(0.0431446880102158,0.665740156173706,
5.37));
#45838=CARTESIAN_POINT('Origin',(0.058901771903038,0.540245586633682,5.4));
#45839=CARTESIAN_POINT('',(0.058901771903038,0.540245586633682,5.4));
#45840=CARTESIAN_POINT('',(0.0572110701908508,0.540419226331774,5.4));
#45841=CARTESIAN_POINT('',(0.058901771903038,0.540245586633682,5.37));
#45842=CARTESIAN_POINT('',(0.058901771903038,0.540245586633682,5.4));
#45843=CARTESIAN_POINT('',(0.058901771903038,0.540245586633682,5.37));
#45844=CARTESIAN_POINT('Ctrl Pts',(0.0885403007268906,0.621282422542572,
5.4));
#45845=CARTESIAN_POINT('Ctrl Pts',(0.0885403007268906,0.621282422542572,
5.37));
#45846=CARTESIAN_POINT('Ctrl Pts',(0.0592770427465439,0.592019134759903,
5.4));
#45847=CARTESIAN_POINT('Ctrl Pts',(0.0592770427465439,0.592019134759903,
5.37));
#45848=CARTESIAN_POINT('Ctrl Pts',(0.058901771903038,0.540245586633682,
5.4));
#45849=CARTESIAN_POINT('Ctrl Pts',(0.058901771903038,0.540245586633682,
5.37));
#45850=CARTESIAN_POINT('',(0.0885403007268906,0.621282422542572,5.4));
#45851=CARTESIAN_POINT('Ctrl Pts',(0.0885403007268906,0.621282422542572,
5.4));
#45852=CARTESIAN_POINT('Ctrl Pts',(0.0592770427465439,0.592019134759903,
5.4));
#45853=CARTESIAN_POINT('Ctrl Pts',(0.058901771903038,0.540245586633682,
5.4));
#45854=CARTESIAN_POINT('',(0.0885403007268906,0.621282422542572,5.37));
#45855=CARTESIAN_POINT('',(0.0885403007268906,0.621282422542572,5.4));
#45856=CARTESIAN_POINT('Ctrl Pts',(0.0885403007268906,0.621282422542572,
5.37));
#45857=CARTESIAN_POINT('Ctrl Pts',(0.0592770427465439,0.592019134759903,
5.37));
#45858=CARTESIAN_POINT('Ctrl Pts',(0.058901771903038,0.540245586633682,
5.37));
#45859=CARTESIAN_POINT('Ctrl Pts',(0.166575655341148,0.650545740127563,
5.4));
#45860=CARTESIAN_POINT('Ctrl Pts',(0.166575655341148,0.650545740127563,
5.37));
#45861=CARTESIAN_POINT('Ctrl Pts',(0.117803558707237,0.650545740127563,
5.4));
#45862=CARTESIAN_POINT('Ctrl Pts',(0.117803558707237,0.650545740127563,
5.37));
#45863=CARTESIAN_POINT('Ctrl Pts',(0.0885403007268906,0.621282422542572,
5.4));
#45864=CARTESIAN_POINT('Ctrl Pts',(0.0885403007268906,0.621282422542572,
5.37));
#45865=CARTESIAN_POINT('',(0.166575655341148,0.650545740127563,5.4));
#45866=CARTESIAN_POINT('Ctrl Pts',(0.166575655341148,0.650545740127563,
5.4));
#45867=CARTESIAN_POINT('Ctrl Pts',(0.117803558707237,0.650545740127563,
5.4));
#45868=CARTESIAN_POINT('Ctrl Pts',(0.0885403007268906,0.621282422542572,
5.4));
#45869=CARTESIAN_POINT('',(0.166575655341148,0.650545740127563,5.37));
#45870=CARTESIAN_POINT('',(0.166575655341148,0.650545740127563,5.4));
#45871=CARTESIAN_POINT('Ctrl Pts',(0.166575655341148,0.650545740127563,
5.37));
#45872=CARTESIAN_POINT('Ctrl Pts',(0.117803558707237,0.650545740127563,
5.37));
#45873=CARTESIAN_POINT('Ctrl Pts',(0.0885403007268906,0.621282422542572,
5.37));
#45874=CARTESIAN_POINT('Ctrl Pts',(0.241422161459923,0.622970694303513,
5.4));
#45875=CARTESIAN_POINT('Ctrl Pts',(0.241422161459923,0.622970694303513,
5.37));
#45876=CARTESIAN_POINT('Ctrl Pts',(0.212721809744835,0.650545740127563,
5.4));
#45877=CARTESIAN_POINT('Ctrl Pts',(0.212721809744835,0.650545740127563,
5.37));
#45878=CARTESIAN_POINT('Ctrl Pts',(0.166575655341148,0.650545740127563,
5.4));
#45879=CARTESIAN_POINT('Ctrl Pts',(0.166575655341148,0.650545740127563,
5.37));
#45880=CARTESIAN_POINT('',(0.241422161459923,0.622970694303513,5.4));
#45881=CARTESIAN_POINT('Ctrl Pts',(0.241422161459923,0.622970694303513,
5.4));
#45882=CARTESIAN_POINT('Ctrl Pts',(0.212721809744835,0.650545740127563,
5.4));
#45883=CARTESIAN_POINT('Ctrl Pts',(0.166575655341148,0.650545740127563,
5.4));
#45884=CARTESIAN_POINT('',(0.241422161459923,0.622970694303513,5.37));
#45885=CARTESIAN_POINT('',(0.241422161459923,0.622970694303513,5.4));
#45886=CARTESIAN_POINT('Ctrl Pts',(0.241422161459923,0.622970694303513,
5.37));
#45887=CARTESIAN_POINT('Ctrl Pts',(0.212721809744835,0.650545740127563,
5.37));
#45888=CARTESIAN_POINT('Ctrl Pts',(0.166575655341148,0.650545740127563,
5.37));
#45889=CARTESIAN_POINT('Ctrl Pts',(0.27012275159359,0.555252426862717,5.4));
#45890=CARTESIAN_POINT('Ctrl Pts',(0.27012275159359,0.555252426862717,5.37));
#45891=CARTESIAN_POINT('Ctrl Pts',(0.27012275159359,0.595395648479462,5.4));
#45892=CARTESIAN_POINT('Ctrl Pts',(0.27012275159359,0.595395648479462,5.37));
#45893=CARTESIAN_POINT('Ctrl Pts',(0.241422161459923,0.622970694303513,
5.4));
#45894=CARTESIAN_POINT('Ctrl Pts',(0.241422161459923,0.622970694303513,
5.37));
#45895=CARTESIAN_POINT('',(0.27012275159359,0.555252426862717,5.4));
#45896=CARTESIAN_POINT('Ctrl Pts',(0.27012275159359,0.555252426862717,5.4));
#45897=CARTESIAN_POINT('Ctrl Pts',(0.27012275159359,0.595395648479462,5.4));
#45898=CARTESIAN_POINT('Ctrl Pts',(0.241422161459923,0.622970694303513,
5.4));
#45899=CARTESIAN_POINT('',(0.27012275159359,0.555252426862717,5.37));
#45900=CARTESIAN_POINT('',(0.27012275159359,0.555252426862717,5.4));
#45901=CARTESIAN_POINT('Ctrl Pts',(0.27012275159359,0.555252426862717,5.37));
#45902=CARTESIAN_POINT('Ctrl Pts',(0.27012275159359,0.595395648479462,5.37));
#45903=CARTESIAN_POINT('Ctrl Pts',(0.241422161459923,0.622970694303513,
5.37));
#45904=CARTESIAN_POINT('Ctrl Pts',(0.238608345389366,0.474027985334396,
5.4));
#45905=CARTESIAN_POINT('Ctrl Pts',(0.238608345389366,0.474027985334396,
5.37));
#45906=CARTESIAN_POINT('Ctrl Pts',(0.27012275159359,0.516985023021698,5.4));
#45907=CARTESIAN_POINT('Ctrl Pts',(0.27012275159359,0.516985023021698,5.37));
#45908=CARTESIAN_POINT('Ctrl Pts',(0.27012275159359,0.555252426862717,5.4));
#45909=CARTESIAN_POINT('Ctrl Pts',(0.27012275159359,0.555252426862717,5.37));
#45910=CARTESIAN_POINT('',(0.238608345389366,0.474027985334396,5.4));
#45911=CARTESIAN_POINT('Ctrl Pts',(0.238608345389366,0.474027985334396,
5.4));
#45912=CARTESIAN_POINT('Ctrl Pts',(0.27012275159359,0.516985023021698,5.4));
#45913=CARTESIAN_POINT('Ctrl Pts',(0.27012275159359,0.555252426862717,5.4));
#45914=CARTESIAN_POINT('',(0.238608345389366,0.474027985334396,5.37));
#45915=CARTESIAN_POINT('',(0.238608345389366,0.474027985334396,5.4));
#45916=CARTESIAN_POINT('Ctrl Pts',(0.238608345389366,0.474027985334396,
5.37));
#45917=CARTESIAN_POINT('Ctrl Pts',(0.27012275159359,0.516985023021698,5.37));
#45918=CARTESIAN_POINT('Ctrl Pts',(0.27012275159359,0.555252426862717,5.37));
#45919=CARTESIAN_POINT('Ctrl Pts',(0.117428287863731,0.357537531852722,
5.4));
#45920=CARTESIAN_POINT('Ctrl Pts',(0.117428287863731,0.357537531852722,
5.37));
#45921=CARTESIAN_POINT('Ctrl Pts',(0.207094177603722,0.431070947647095,
5.4));
#45922=CARTESIAN_POINT('Ctrl Pts',(0.207094177603722,0.431070947647095,
5.37));
#45923=CARTESIAN_POINT('Ctrl Pts',(0.238608345389366,0.474027985334396,
5.4));
#45924=CARTESIAN_POINT('Ctrl Pts',(0.238608345389366,0.474027985334396,
5.37));
#45925=CARTESIAN_POINT('',(0.117428287863731,0.357537531852722,5.4));
#45926=CARTESIAN_POINT('Ctrl Pts',(0.117428287863731,0.357537531852722,
5.4));
#45927=CARTESIAN_POINT('Ctrl Pts',(0.207094177603722,0.431070947647095,
5.4));
#45928=CARTESIAN_POINT('Ctrl Pts',(0.238608345389366,0.474027985334396,
5.4));
#45929=CARTESIAN_POINT('',(0.117428287863731,0.357537531852722,5.37));
#45930=CARTESIAN_POINT('',(0.117428287863731,0.357537531852722,5.4));
#45931=CARTESIAN_POINT('Ctrl Pts',(0.117428287863731,0.357537531852722,
5.37));
#45932=CARTESIAN_POINT('Ctrl Pts',(0.207094177603722,0.431070947647095,
5.37));
#45933=CARTESIAN_POINT('Ctrl Pts',(0.238608345389366,0.474027985334396,
5.37));
#45934=CARTESIAN_POINT('Ctrl Pts',(0.0290756076574326,0.274249666929245,
5.4));
#45935=CARTESIAN_POINT('Ctrl Pts',(0.0290756076574326,0.274249666929245,
5.37));
#45936=CARTESIAN_POINT('Ctrl Pts',(0.0596520751714706,0.310266041755676,
5.4));
#45937=CARTESIAN_POINT('Ctrl Pts',(0.0596520751714706,0.310266041755676,
5.37));
#45938=CARTESIAN_POINT('Ctrl Pts',(0.117428287863731,0.357537531852722,
5.4));
#45939=CARTESIAN_POINT('Ctrl Pts',(0.117428287863731,0.357537531852722,
5.37));
#45940=CARTESIAN_POINT('',(0.0290756076574326,0.274249666929245,5.4));
#45941=CARTESIAN_POINT('Ctrl Pts',(0.0290756076574326,0.274249666929245,
5.4));
#45942=CARTESIAN_POINT('Ctrl Pts',(0.0596520751714706,0.310266041755676,
5.4));
#45943=CARTESIAN_POINT('Ctrl Pts',(0.117428287863731,0.357537531852722,
5.4));
#45944=CARTESIAN_POINT('',(0.0290756076574326,0.274249666929245,5.37));
#45945=CARTESIAN_POINT('',(0.0290756076574326,0.274249666929245,5.4));
#45946=CARTESIAN_POINT('Ctrl Pts',(0.0290756076574326,0.274249666929245,
5.37));
#45947=CARTESIAN_POINT('Ctrl Pts',(0.0596520751714706,0.310266041755676,
5.37));
#45948=CARTESIAN_POINT('Ctrl Pts',(0.117428287863731,0.357537531852722,
5.37));
#45949=CARTESIAN_POINT('Ctrl Pts',(-0.0153820663690567,0.201091402769089,
5.4));
#45950=CARTESIAN_POINT('Ctrl Pts',(-0.0153820663690567,0.201091402769089,
5.37));
#45951=CARTESIAN_POINT('Ctrl Pts',(-0.00150062143802643,0.238233292102814,
5.4));
#45952=CARTESIAN_POINT('Ctrl Pts',(-0.00150062143802643,0.238233292102814,
5.37));
#45953=CARTESIAN_POINT('Ctrl Pts',(0.0290756076574326,0.274249666929245,
5.4));
#45954=CARTESIAN_POINT('Ctrl Pts',(0.0290756076574326,0.274249666929245,
5.37));
#45955=CARTESIAN_POINT('',(-0.0153820663690567,0.201091402769089,5.4));
#45956=CARTESIAN_POINT('Ctrl Pts',(-0.0153820663690567,0.201091402769089,
5.4));
#45957=CARTESIAN_POINT('Ctrl Pts',(-0.00150062143802643,0.238233292102814,
5.4));
#45958=CARTESIAN_POINT('Ctrl Pts',(0.0290756076574326,0.274249666929245,
5.4));
#45959=CARTESIAN_POINT('',(-0.0153820663690567,0.201091402769089,5.37));
#45960=CARTESIAN_POINT('',(-0.0153820663690567,0.201091402769089,5.4));
#45961=CARTESIAN_POINT('Ctrl Pts',(-0.0153820663690567,0.201091402769089,
5.37));
#45962=CARTESIAN_POINT('Ctrl Pts',(-0.00150062143802643,0.238233292102814,
5.37));
#45963=CARTESIAN_POINT('Ctrl Pts',(0.0290756076574326,0.274249666929245,
5.37));
#45964=CARTESIAN_POINT('Ctrl Pts',(-0.0232606083154678,0.154195094108582,
5.4));
#45965=CARTESIAN_POINT('Ctrl Pts',(-0.0232606083154678,0.154195094108582,
5.37));
#45966=CARTESIAN_POINT('Ctrl Pts',(-0.0240109115839005,0.17858117222786,
5.4));
#45967=CARTESIAN_POINT('Ctrl Pts',(-0.0240109115839005,0.17858117222786,
5.37));
#45968=CARTESIAN_POINT('Ctrl Pts',(-0.0153820663690567,0.201091402769089,
5.4));
#45969=CARTESIAN_POINT('Ctrl Pts',(-0.0153820663690567,0.201091402769089,
5.37));
#45970=CARTESIAN_POINT('',(-0.0232606083154678,0.154195094108582,5.4));
#45971=CARTESIAN_POINT('Ctrl Pts',(-0.0232606083154678,0.154195094108582,
5.4));
#45972=CARTESIAN_POINT('Ctrl Pts',(-0.0240109115839005,0.17858117222786,
5.4));
#45973=CARTESIAN_POINT('Ctrl Pts',(-0.0153820663690567,0.201091402769089,
5.4));
#45974=CARTESIAN_POINT('',(-0.0232606083154678,0.154195094108582,5.37));
#45975=CARTESIAN_POINT('',(-0.0232606083154678,0.154195094108582,5.4));
#45976=CARTESIAN_POINT('Ctrl Pts',(-0.0232606083154678,0.154195094108582,
5.37));
#45977=CARTESIAN_POINT('Ctrl Pts',(-0.0240109115839005,0.17858117222786,
5.37));
#45978=CARTESIAN_POINT('Ctrl Pts',(-0.0153820663690567,0.201091402769089,
5.37));
#45979=CARTESIAN_POINT('Origin',(0.340279564261436,0.154195094108582,5.4));
#45980=CARTESIAN_POINT('',(0.340279564261436,0.154195094108582,5.4));
#45981=CARTESIAN_POINT('',(0.170139782130718,0.154195094108582,5.4));
#45982=CARTESIAN_POINT('',(0.340279564261436,0.154195094108582,5.37));
#45983=CARTESIAN_POINT('',(0.340279564261436,0.154195094108582,5.4));
#45984=CARTESIAN_POINT('',(0.340279564261436,0.154195094108582,5.37));
#45985=CARTESIAN_POINT('Origin',(0.340279564261436,0.219099605083466,5.4));
#45986=CARTESIAN_POINT('',(0.340279564261436,0.219099605083466,5.4));
#45987=CARTESIAN_POINT('',(0.340279564261436,0.109549802541733,5.4));
#45988=CARTESIAN_POINT('',(0.340279564261436,0.219099605083466,5.37));
#45989=CARTESIAN_POINT('',(0.340279564261436,0.219099605083466,5.4));
#45990=CARTESIAN_POINT('',(0.340279564261436,0.219099605083466,5.37));
#45991=CARTESIAN_POINT('Origin',(0.0705320686101913,0.219099605083466,5.4));
#45992=CARTESIAN_POINT('',(0.0705320686101913,0.219099605083466,5.4));
#45993=CARTESIAN_POINT('',(0.0352660343050957,0.219099605083466,5.4));
#45994=CARTESIAN_POINT('',(0.0705320686101913,0.219099605083466,5.37));
#45995=CARTESIAN_POINT('',(0.0705320686101913,0.219099605083466,5.4));
#45996=CARTESIAN_POINT('',(0.0705320686101913,0.219099605083466,5.37));
#45997=CARTESIAN_POINT('Ctrl Pts',(0.0990450233221054,0.255678737163544,
5.4));
#45998=CARTESIAN_POINT('Ctrl Pts',(0.0990450233221054,0.255678737163544,
5.37));
#45999=CARTESIAN_POINT('Ctrl Pts',(0.0817870944738388,0.237482959032059,
5.4));
#46000=CARTESIAN_POINT('Ctrl Pts',(0.0817870944738388,0.237482959032059,
5.37));
#46001=CARTESIAN_POINT('Ctrl Pts',(0.0705320686101913,0.219099605083466,
5.4));
#46002=CARTESIAN_POINT('Ctrl Pts',(0.0705320686101913,0.219099605083466,
5.37));
#46003=CARTESIAN_POINT('Ctrl Pts',(0.0990450233221054,0.255678737163544,
5.4));
#46004=CARTESIAN_POINT('Ctrl Pts',(0.0817870944738388,0.237482959032059,
5.4));
#46005=CARTESIAN_POINT('Ctrl Pts',(0.0705320686101913,0.219099605083466,
5.4));
#46006=CARTESIAN_POINT('Ctrl Pts',(0.0990450233221054,0.255678737163544,
5.37));
#46007=CARTESIAN_POINT('Ctrl Pts',(0.0817870944738388,0.237482959032059,
5.37));
#46008=CARTESIAN_POINT('Ctrl Pts',(0.0705320686101913,0.219099605083466,
5.37));
#46009=CARTESIAN_POINT('Origin',(0.158134326338768,0.43032061457634,5.37));
#46010=CARTESIAN_POINT('Origin',(1.08049105107784,0.639290624856949,5.4));
#46011=CARTESIAN_POINT('',(1.08049105107784,0.639290624856949,5.4));
#46012=CARTESIAN_POINT('',(0.939802154898643,0.639290624856949,5.4));
#46013=CARTESIAN_POINT('',(0.540245525538921,0.639290624856949,5.4));
#46014=CARTESIAN_POINT('',(1.08049105107784,0.639290624856949,5.37));
#46015=CARTESIAN_POINT('',(1.08049105107784,0.639290624856949,5.4));
#46016=CARTESIAN_POINT('',(0.939802154898643,0.639290624856949,5.37));
#46017=CARTESIAN_POINT('',(1.08049105107784,0.639290624856949,5.37));
#46018=CARTESIAN_POINT('',(0.939802154898643,0.639290624856949,5.4));
#46019=CARTESIAN_POINT('Ctrl Pts',(1.14839695394039,0.634413385391235,5.4));
#46020=CARTESIAN_POINT('Ctrl Pts',(1.14839695394039,0.634413385391235,5.37));
#46021=CARTESIAN_POINT('Ctrl Pts',(1.13001345098019,0.639290624856949,5.4));
#46022=CARTESIAN_POINT('Ctrl Pts',(1.13001345098019,0.639290624856949,5.37));
#46023=CARTESIAN_POINT('Ctrl Pts',(1.08049105107784,0.639290624856949,5.4));
#46024=CARTESIAN_POINT('Ctrl Pts',(1.08049105107784,0.639290624856949,5.37));
#46025=CARTESIAN_POINT('',(1.14839695394039,0.634413385391235,5.4));
#46026=CARTESIAN_POINT('Ctrl Pts',(1.14839695394039,0.634413385391235,5.4));
#46027=CARTESIAN_POINT('Ctrl Pts',(1.13001345098019,0.639290624856949,5.4));
#46028=CARTESIAN_POINT('Ctrl Pts',(1.08049105107784,0.639290624856949,5.4));
#46029=CARTESIAN_POINT('',(1.14839695394039,0.634413385391235,5.37));
#46030=CARTESIAN_POINT('',(1.14839695394039,0.634413385391235,5.4));
#46031=CARTESIAN_POINT('Ctrl Pts',(1.14839695394039,0.634413385391235,5.37));
#46032=CARTESIAN_POINT('Ctrl Pts',(1.13001345098019,0.639290624856949,5.37));
#46033=CARTESIAN_POINT('Ctrl Pts',(1.08049105107784,0.639290624856949,5.37));
#46034=CARTESIAN_POINT('Ctrl Pts',(1.19435547292233,0.601961159706116,5.4));
#46035=CARTESIAN_POINT('Ctrl Pts',(1.19435547292233,0.601961159706116,5.37));
#46036=CARTESIAN_POINT('Ctrl Pts',(1.17690990865231,0.626534813642502,5.4));
#46037=CARTESIAN_POINT('Ctrl Pts',(1.17690990865231,0.626534813642502,5.37));
#46038=CARTESIAN_POINT('Ctrl Pts',(1.14839695394039,0.634413385391235,5.4));
#46039=CARTESIAN_POINT('Ctrl Pts',(1.14839695394039,0.634413385391235,5.37));
#46040=CARTESIAN_POINT('',(1.19435547292233,0.601961159706116,5.4));
#46041=CARTESIAN_POINT('Ctrl Pts',(1.19435547292233,0.601961159706116,5.4));
#46042=CARTESIAN_POINT('Ctrl Pts',(1.17690990865231,0.626534813642502,5.4));
#46043=CARTESIAN_POINT('Ctrl Pts',(1.14839695394039,0.634413385391235,5.4));
#46044=CARTESIAN_POINT('',(1.19435547292233,0.601961159706116,5.37));
#46045=CARTESIAN_POINT('',(1.19435547292233,0.601961159706116,5.4));
#46046=CARTESIAN_POINT('Ctrl Pts',(1.19435547292233,0.601961159706116,5.37));
#46047=CARTESIAN_POINT('Ctrl Pts',(1.17690990865231,0.626534813642502,5.37));
#46048=CARTESIAN_POINT('Ctrl Pts',(1.14839695394039,0.634413385391235,5.37));
#46049=CARTESIAN_POINT('Ctrl Pts',(1.21180103719234,0.542871797084808,5.4));
#46050=CARTESIAN_POINT('Ctrl Pts',(1.21180103719234,0.542871797084808,5.37));
#46051=CARTESIAN_POINT('Ctrl Pts',(1.21180103719234,0.577387475967407,5.4));
#46052=CARTESIAN_POINT('Ctrl Pts',(1.21180103719234,0.577387475967407,5.37));
#46053=CARTESIAN_POINT('Ctrl Pts',(1.19435547292233,0.601961159706116,5.4));
#46054=CARTESIAN_POINT('Ctrl Pts',(1.19435547292233,0.601961159706116,5.37));
#46055=CARTESIAN_POINT('',(1.21180103719234,0.542871797084808,5.4));
#46056=CARTESIAN_POINT('Ctrl Pts',(1.21180103719234,0.542871797084808,5.4));
#46057=CARTESIAN_POINT('Ctrl Pts',(1.21180103719234,0.577387475967407,5.4));
#46058=CARTESIAN_POINT('Ctrl Pts',(1.19435547292233,0.601961159706116,5.4));
#46059=CARTESIAN_POINT('',(1.21180103719234,0.542871797084808,5.37));
#46060=CARTESIAN_POINT('',(1.21180103719234,0.542871797084808,5.4));
#46061=CARTESIAN_POINT('Ctrl Pts',(1.21180103719234,0.542871797084808,5.37));
#46062=CARTESIAN_POINT('Ctrl Pts',(1.21180103719234,0.577387475967407,5.37));
#46063=CARTESIAN_POINT('Ctrl Pts',(1.19435547292233,0.601961159706116,5.37));
#46064=CARTESIAN_POINT('Ctrl Pts',(1.18216226994991,0.468963199853897,5.4));
#46065=CARTESIAN_POINT('Ctrl Pts',(1.18216226994991,0.468963199853897,5.37));
#46066=CARTESIAN_POINT('Ctrl Pts',(1.21180103719234,0.495225125551224,5.4));
#46067=CARTESIAN_POINT('Ctrl Pts',(1.21180103719234,0.495225125551224,5.37));
#46068=CARTESIAN_POINT('Ctrl Pts',(1.21180103719234,0.542871797084808,5.4));
#46069=CARTESIAN_POINT('Ctrl Pts',(1.21180103719234,0.542871797084808,5.37));
#46070=CARTESIAN_POINT('',(1.18216226994991,0.468963199853897,5.4));
#46071=CARTESIAN_POINT('Ctrl Pts',(1.18216226994991,0.468963199853897,5.4));
#46072=CARTESIAN_POINT('Ctrl Pts',(1.21180103719234,0.495225125551224,5.4));
#46073=CARTESIAN_POINT('Ctrl Pts',(1.21180103719234,0.542871797084808,5.4));
#46074=CARTESIAN_POINT('',(1.18216226994991,0.468963199853897,5.37));
#46075=CARTESIAN_POINT('',(1.18216226994991,0.468963199853897,5.4));
#46076=CARTESIAN_POINT('Ctrl Pts',(1.18216226994991,0.468963199853897,5.37));
#46077=CARTESIAN_POINT('Ctrl Pts',(1.21180103719234,0.495225125551224,5.37));
#46078=CARTESIAN_POINT('Ctrl Pts',(1.21180103719234,0.542871797084808,5.37));
#46079=CARTESIAN_POINT('Ctrl Pts',(1.08199213445187,0.442701244354248,5.4));
#46080=CARTESIAN_POINT('Ctrl Pts',(1.08199213445187,0.442701244354248,5.37));
#46081=CARTESIAN_POINT('Ctrl Pts',(1.15252397954464,0.442701244354248,5.4));
#46082=CARTESIAN_POINT('Ctrl Pts',(1.15252397954464,0.442701244354248,5.37));
#46083=CARTESIAN_POINT('Ctrl Pts',(1.18216226994991,0.468963199853897,5.4));
#46084=CARTESIAN_POINT('Ctrl Pts',(1.18216226994991,0.468963199853897,5.37));
#46085=CARTESIAN_POINT('',(1.08199213445187,0.442701244354248,5.4));
#46086=CARTESIAN_POINT('Ctrl Pts',(1.08199213445187,0.442701244354248,5.4));
#46087=CARTESIAN_POINT('Ctrl Pts',(1.15252397954464,0.442701244354248,5.4));
#46088=CARTESIAN_POINT('Ctrl Pts',(1.18216226994991,0.468963199853897,5.4));
#46089=CARTESIAN_POINT('',(1.08199213445187,0.442701244354248,5.37));
#46090=CARTESIAN_POINT('',(1.08199213445187,0.442701244354248,5.4));
#46091=CARTESIAN_POINT('Ctrl Pts',(1.08199213445187,0.442701244354248,5.37));
#46092=CARTESIAN_POINT('Ctrl Pts',(1.15252397954464,0.442701244354248,5.37));
#46093=CARTESIAN_POINT('Ctrl Pts',(1.18216226994991,0.468963199853897,5.37));
#46094=CARTESIAN_POINT('Origin',(0.939802154898643,0.442701244354248,5.4));
#46095=CARTESIAN_POINT('',(0.939802154898643,0.442701244354248,5.4));
#46096=CARTESIAN_POINT('',(0.469901077449322,0.442701244354248,5.4));
#46097=CARTESIAN_POINT('',(0.939802154898643,0.442701244354248,5.37));
#46098=CARTESIAN_POINT('',(0.939802154898643,0.442701244354248,5.4));
#46099=CARTESIAN_POINT('',(0.939802154898643,0.442701244354248,5.37));
#46100=CARTESIAN_POINT('Origin',(0.939802154898643,0.639290624856949,5.4));
#46101=CARTESIAN_POINT('',(0.939802154898643,0.319645312428474,5.4));
#46102=CARTESIAN_POINT('',(0.939802154898643,0.639290624856949,5.37));
#46103=CARTESIAN_POINT('Origin',(1.08086632192135,0.377796748280525,5.4));
#46104=CARTESIAN_POINT('',(1.08086632192135,0.377796748280525,5.4));
#46105=CARTESIAN_POINT('',(0.939802154898643,0.377796748280525,5.4));
#46106=CARTESIAN_POINT('',(0.540433160960674,0.377796748280525,5.4));
#46107=CARTESIAN_POINT('',(1.08086632192135,0.377796748280525,5.37));
#46108=CARTESIAN_POINT('',(1.08086632192135,0.377796748280525,5.4));
#46109=CARTESIAN_POINT('',(0.939802154898643,0.377796748280525,5.37));
#46110=CARTESIAN_POINT('',(1.08086632192135,0.377796748280525,5.37));
#46111=CARTESIAN_POINT('',(0.939802154898643,0.377796748280525,5.4));
#46112=CARTESIAN_POINT('Ctrl Pts',(1.24218986928463,0.426381343603134,5.4));
#46113=CARTESIAN_POINT('Ctrl Pts',(1.24218986928463,0.426381343603134,5.37));
#46114=CARTESIAN_POINT('Ctrl Pts',(1.19754455983639,0.377796748280525,5.4));
#46115=CARTESIAN_POINT('Ctrl Pts',(1.19754455983639,0.377796748280525,5.37));
#46116=CARTESIAN_POINT('Ctrl Pts',(1.08086632192135,0.377796748280525,5.4));
#46117=CARTESIAN_POINT('Ctrl Pts',(1.08086632192135,0.377796748280525,5.37));
#46118=CARTESIAN_POINT('',(1.24218986928463,0.426381343603134,5.4));
#46119=CARTESIAN_POINT('Ctrl Pts',(1.24218986928463,0.426381343603134,5.4));
#46120=CARTESIAN_POINT('Ctrl Pts',(1.19754455983639,0.377796748280525,5.4));
#46121=CARTESIAN_POINT('Ctrl Pts',(1.08086632192135,0.377796748280525,5.4));
#46122=CARTESIAN_POINT('',(1.24218986928463,0.426381343603134,5.37));
#46123=CARTESIAN_POINT('',(1.24218986928463,0.426381343603134,5.4));
#46124=CARTESIAN_POINT('Ctrl Pts',(1.24218986928463,0.426381343603134,5.37));
#46125=CARTESIAN_POINT('Ctrl Pts',(1.19754455983639,0.377796748280525,5.37));
#46126=CARTESIAN_POINT('Ctrl Pts',(1.08086632192135,0.377796748280525,5.37));
#46127=CARTESIAN_POINT('Ctrl Pts',(1.28683517873287,0.545122796297073,5.4));
#46128=CARTESIAN_POINT('Ctrl Pts',(1.28683517873287,0.545122796297073,5.37));
#46129=CARTESIAN_POINT('Ctrl Pts',(1.28683517873287,0.474965924024582,5.4));
#46130=CARTESIAN_POINT('Ctrl Pts',(1.28683517873287,0.474965924024582,5.37));
#46131=CARTESIAN_POINT('Ctrl Pts',(1.24218986928463,0.426381343603134,5.4));
#46132=CARTESIAN_POINT('Ctrl Pts',(1.24218986928463,0.426381343603134,5.37));
#46133=CARTESIAN_POINT('',(1.28683517873287,0.545122796297073,5.4));
#46134=CARTESIAN_POINT('Ctrl Pts',(1.28683517873287,0.545122796297073,5.4));
#46135=CARTESIAN_POINT('Ctrl Pts',(1.28683517873287,0.474965924024582,5.4));
#46136=CARTESIAN_POINT('Ctrl Pts',(1.24218986928463,0.426381343603134,5.4));
#46137=CARTESIAN_POINT('',(1.28683517873287,0.545122796297073,5.37));
#46138=CARTESIAN_POINT('',(1.28683517873287,0.545122796297073,5.4));
#46139=CARTESIAN_POINT('Ctrl Pts',(1.28683517873287,0.545122796297073,5.37));
#46140=CARTESIAN_POINT('Ctrl Pts',(1.28683517873287,0.474965924024582,5.37));
#46141=CARTESIAN_POINT('Ctrl Pts',(1.24218986928463,0.426381343603134,5.37));
#46142=CARTESIAN_POINT('Ctrl Pts',(1.27013967931271,0.620156908035278,5.4));
#46143=CARTESIAN_POINT('Ctrl Pts',(1.27013967931271,0.620156908035278,5.37));
#46144=CARTESIAN_POINT('Ctrl Pts',(1.28683517873287,0.586016410589218,5.4));
#46145=CARTESIAN_POINT('Ctrl Pts',(1.28683517873287,0.586016410589218,5.37));
#46146=CARTESIAN_POINT('Ctrl Pts',(1.28683517873287,0.545122796297073,5.4));
#46147=CARTESIAN_POINT('Ctrl Pts',(1.28683517873287,0.545122796297073,5.37));
#46148=CARTESIAN_POINT('',(1.27013967931271,0.620156908035278,5.4));
#46149=CARTESIAN_POINT('Ctrl Pts',(1.27013967931271,0.620156908035278,5.4));
#46150=CARTESIAN_POINT('Ctrl Pts',(1.28683517873287,0.586016410589218,5.4));
#46151=CARTESIAN_POINT('Ctrl Pts',(1.28683517873287,0.545122796297073,5.4));
#46152=CARTESIAN_POINT('',(1.27013967931271,0.620156908035278,5.37));
#46153=CARTESIAN_POINT('',(1.27013967931271,0.620156908035278,5.4));
#46154=CARTESIAN_POINT('Ctrl Pts',(1.27013967931271,0.620156908035278,5.37));
#46155=CARTESIAN_POINT('Ctrl Pts',(1.28683517873287,0.586016410589218,5.37));
#46156=CARTESIAN_POINT('Ctrl Pts',(1.28683517873287,0.545122796297073,5.37));
#46157=CARTESIAN_POINT('Ctrl Pts',(1.2260575145483,0.673243546485901,5.4));
#46158=CARTESIAN_POINT('Ctrl Pts',(1.2260575145483,0.673243546485901,5.37));
#46159=CARTESIAN_POINT('Ctrl Pts',(1.2534446567297,0.654297435283661,5.4));
#46160=CARTESIAN_POINT('Ctrl Pts',(1.2534446567297,0.654297435283661,5.37));
#46161=CARTESIAN_POINT('Ctrl Pts',(1.27013967931271,0.620156908035278,5.4));
#46162=CARTESIAN_POINT('Ctrl Pts',(1.27013967931271,0.620156908035278,5.37));
#46163=CARTESIAN_POINT('',(1.2260575145483,0.673243546485901,5.4));
#46164=CARTESIAN_POINT('Ctrl Pts',(1.2260575145483,0.673243546485901,5.4));
#46165=CARTESIAN_POINT('Ctrl Pts',(1.2534446567297,0.654297435283661,5.4));
#46166=CARTESIAN_POINT('Ctrl Pts',(1.27013967931271,0.620156908035278,5.4));
#46167=CARTESIAN_POINT('',(1.2260575145483,0.673243546485901,5.37));
#46168=CARTESIAN_POINT('',(1.2260575145483,0.673243546485901,5.4));
#46169=CARTESIAN_POINT('Ctrl Pts',(1.2260575145483,0.673243546485901,5.37));
#46170=CARTESIAN_POINT('Ctrl Pts',(1.2534446567297,0.654297435283661,5.37));
#46171=CARTESIAN_POINT('Ctrl Pts',(1.27013967931271,0.620156908035278,5.37));
#46172=CARTESIAN_POINT('Ctrl Pts',(1.15815161168575,0.698942744731903,5.4));
#46173=CARTESIAN_POINT('Ctrl Pts',(1.15815161168575,0.698942744731903,5.37));
#46174=CARTESIAN_POINT('Ctrl Pts',(1.19866989552975,0.692189657688141,5.4));
#46175=CARTESIAN_POINT('Ctrl Pts',(1.19866989552975,0.692189657688141,5.37));
#46176=CARTESIAN_POINT('Ctrl Pts',(1.2260575145483,0.673243546485901,5.4));
#46177=CARTESIAN_POINT('Ctrl Pts',(1.2260575145483,0.673243546485901,5.37));
#46178=CARTESIAN_POINT('',(1.15815161168575,0.698942744731903,5.4));
#46179=CARTESIAN_POINT('Ctrl Pts',(1.15815161168575,0.698942744731903,5.4));
#46180=CARTESIAN_POINT('Ctrl Pts',(1.19866989552975,0.692189657688141,5.4));
#46181=CARTESIAN_POINT('Ctrl Pts',(1.2260575145483,0.673243546485901,5.4));
#46182=CARTESIAN_POINT('',(1.15815161168575,0.698942744731903,5.37));
#46183=CARTESIAN_POINT('',(1.15815161168575,0.698942744731903,5.4));
#46184=CARTESIAN_POINT('Ctrl Pts',(1.15815161168575,0.698942744731903,5.37));
#46185=CARTESIAN_POINT('Ctrl Pts',(1.19866989552975,0.692189657688141,5.37));
#46186=CARTESIAN_POINT('Ctrl Pts',(1.2260575145483,0.673243546485901,5.37));
#46187=CARTESIAN_POINT('Ctrl Pts',(1.07448862493038,0.704195106029511,5.4));
#46188=CARTESIAN_POINT('Ctrl Pts',(1.07448862493038,0.704195106029511,5.37));
#46189=CARTESIAN_POINT('Ctrl Pts',(1.12926338613033,0.704195106029511,5.4));
#46190=CARTESIAN_POINT('Ctrl Pts',(1.12926338613033,0.704195106029511,5.37));
#46191=CARTESIAN_POINT('Ctrl Pts',(1.15815161168575,0.698942744731903,5.4));
#46192=CARTESIAN_POINT('Ctrl Pts',(1.15815161168575,0.698942744731903,5.37));
#46193=CARTESIAN_POINT('',(1.07448862493038,0.704195106029511,5.4));
#46194=CARTESIAN_POINT('Ctrl Pts',(1.07448862493038,0.704195106029511,5.4));
#46195=CARTESIAN_POINT('Ctrl Pts',(1.12926338613033,0.704195106029511,5.4));
#46196=CARTESIAN_POINT('Ctrl Pts',(1.15815161168575,0.698942744731903,5.4));
#46197=CARTESIAN_POINT('',(1.07448862493038,0.704195106029511,5.37));
#46198=CARTESIAN_POINT('',(1.07448862493038,0.704195106029511,5.4));
#46199=CARTESIAN_POINT('Ctrl Pts',(1.07448862493038,0.704195106029511,5.37));
#46200=CARTESIAN_POINT('Ctrl Pts',(1.12926338613033,0.704195106029511,5.37));
#46201=CARTESIAN_POINT('Ctrl Pts',(1.15815161168575,0.698942744731903,5.37));
#46202=CARTESIAN_POINT('Origin',(0.867019161581993,0.704195106029511,5.4));
#46203=CARTESIAN_POINT('',(0.867019161581993,0.704195106029511,5.4));
#46204=CARTESIAN_POINT('',(0.433509580790997,0.704195106029511,5.4));
#46205=CARTESIAN_POINT('',(0.867019161581993,0.704195106029511,5.37));
#46206=CARTESIAN_POINT('',(0.867019161581993,0.704195106029511,5.4));
#46207=CARTESIAN_POINT('',(0.867019161581993,0.704195106029511,5.37));
#46208=CARTESIAN_POINT('Origin',(0.867019161581993,0.154195094108582,5.4));
#46209=CARTESIAN_POINT('',(0.867019161581993,0.154195094108582,5.4));
#46210=CARTESIAN_POINT('',(0.867019161581993,0.0770975470542908,5.4));
#46211=CARTESIAN_POINT('',(0.867019161581993,0.154195094108582,5.37));
#46212=CARTESIAN_POINT('',(0.867019161581993,0.154195094108582,5.4));
#46213=CARTESIAN_POINT('',(0.867019161581993,0.154195094108582,5.37));
#46214=CARTESIAN_POINT('Origin',(0.939802154898643,0.154195094108582,5.4));
#46215=CARTESIAN_POINT('',(0.939802154898643,0.154195094108582,5.4));
#46216=CARTESIAN_POINT('',(0.469901077449322,0.154195094108582,5.4));
#46217=CARTESIAN_POINT('',(0.939802154898643,0.154195094108582,5.37));
#46218=CARTESIAN_POINT('',(0.939802154898643,0.154195094108582,5.4));
#46219=CARTESIAN_POINT('',(0.939802154898643,0.154195094108582,5.37));
#46220=CARTESIAN_POINT('Origin',(0.939802154898643,0.377796748280525,5.4));
#46221=CARTESIAN_POINT('',(0.939802154898643,0.188898374140263,5.4));
#46222=CARTESIAN_POINT('',(0.939802154898643,0.377796748280525,5.37));
#46223=CARTESIAN_POINT('Origin',(1.07692717015743,0.429195100069046,5.37));
#46224=CARTESIAN_POINT('Ctrl Pts',(2.16323326528072,0.451330178976059,5.4));
#46225=CARTESIAN_POINT('Ctrl Pts',(2.16323326528072,0.451330178976059,5.37));
#46226=CARTESIAN_POINT('Ctrl Pts',(2.11746262013912,0.451330178976059,5.4));
#46227=CARTESIAN_POINT('Ctrl Pts',(2.11746262013912,0.451330178976059,5.37));
#46228=CARTESIAN_POINT('Ctrl Pts',(2.08557318150997,0.418502742052078,5.4));
#46229=CARTESIAN_POINT('Ctrl Pts',(2.08557318150997,0.418502742052078,5.37));
#46230=CARTESIAN_POINT('',(2.16323326528072,0.451330178976059,5.4));
#46231=CARTESIAN_POINT('',(2.08557318150997,0.418502742052078,5.4));
#46232=CARTESIAN_POINT('Ctrl Pts',(2.16323326528072,0.451330178976059,5.4));
#46233=CARTESIAN_POINT('Ctrl Pts',(2.11746262013912,0.451330178976059,5.4));
#46234=CARTESIAN_POINT('Ctrl Pts',(2.08557318150997,0.418502742052078,5.4));
#46235=CARTESIAN_POINT('',(2.16323326528072,0.451330178976059,5.37));
#46236=CARTESIAN_POINT('',(2.16323326528072,0.451330178976059,5.4));
#46237=CARTESIAN_POINT('',(2.08557318150997,0.418502742052078,5.37));
#46238=CARTESIAN_POINT('Ctrl Pts',(2.16323326528072,0.451330178976059,5.37));
#46239=CARTESIAN_POINT('Ctrl Pts',(2.11746262013912,0.451330178976059,5.37));
#46240=CARTESIAN_POINT('Ctrl Pts',(2.08557318150997,0.418502742052078,5.37));
#46241=CARTESIAN_POINT('',(2.08557318150997,0.418502742052078,5.4));
#46242=CARTESIAN_POINT('Ctrl Pts',(2.23976801335812,0.418502742052078,5.4));
#46243=CARTESIAN_POINT('Ctrl Pts',(2.23976801335812,0.418502742052078,5.37));
#46244=CARTESIAN_POINT('Ctrl Pts',(2.20937918126583,0.451330178976059,5.4));
#46245=CARTESIAN_POINT('Ctrl Pts',(2.20937918126583,0.451330178976059,5.37));
#46246=CARTESIAN_POINT('Ctrl Pts',(2.16323326528072,0.451330178976059,5.4));
#46247=CARTESIAN_POINT('Ctrl Pts',(2.16323326528072,0.451330178976059,5.37));
#46248=CARTESIAN_POINT('',(2.23976801335812,0.418502742052078,5.4));
#46249=CARTESIAN_POINT('Ctrl Pts',(2.23976801335812,0.418502742052078,5.4));
#46250=CARTESIAN_POINT('Ctrl Pts',(2.20937918126583,0.451330178976059,5.4));
#46251=CARTESIAN_POINT('Ctrl Pts',(2.16323326528072,0.451330178976059,5.4));
#46252=CARTESIAN_POINT('',(2.23976801335812,0.418502742052078,5.37));
#46253=CARTESIAN_POINT('',(2.23976801335812,0.418502742052078,5.4));
#46254=CARTESIAN_POINT('Ctrl Pts',(2.23976801335812,0.418502742052078,5.37));
#46255=CARTESIAN_POINT('Ctrl Pts',(2.20937918126583,0.451330178976059,5.37));
#46256=CARTESIAN_POINT('Ctrl Pts',(2.16323326528072,0.451330178976059,5.37));
#46257=CARTESIAN_POINT('Ctrl Pts',(2.2701568454504,0.328649395704269,5.4));
#46258=CARTESIAN_POINT('Ctrl Pts',(2.2701568454504,0.328649395704269,5.37));
#46259=CARTESIAN_POINT('Ctrl Pts',(2.2701568454504,0.385675320029259,5.4));
#46260=CARTESIAN_POINT('Ctrl Pts',(2.2701568454504,0.385675320029259,5.37));
#46261=CARTESIAN_POINT('Ctrl Pts',(2.23976801335812,0.418502742052078,5.4));
#46262=CARTESIAN_POINT('Ctrl Pts',(2.23976801335812,0.418502742052078,5.37));
#46263=CARTESIAN_POINT('',(2.2701568454504,0.328649395704269,5.4));
#46264=CARTESIAN_POINT('Ctrl Pts',(2.2701568454504,0.328649395704269,5.4));
#46265=CARTESIAN_POINT('Ctrl Pts',(2.2701568454504,0.385675320029259,5.4));
#46266=CARTESIAN_POINT('Ctrl Pts',(2.23976801335812,0.418502742052078,5.4));
#46267=CARTESIAN_POINT('',(2.2701568454504,0.328649395704269,5.37));
#46268=CARTESIAN_POINT('',(2.2701568454504,0.328649395704269,5.4));
#46269=CARTESIAN_POINT('Ctrl Pts',(2.2701568454504,0.328649395704269,5.37));
#46270=CARTESIAN_POINT('Ctrl Pts',(2.2701568454504,0.385675320029259,5.37));
#46271=CARTESIAN_POINT('Ctrl Pts',(2.23976801335812,0.418502742052078,5.37));
#46272=CARTESIAN_POINT('Ctrl Pts',(2.23939274251461,0.234856748580933,5.4));
#46273=CARTESIAN_POINT('Ctrl Pts',(2.23939274251461,0.234856748580933,5.37));
#46274=CARTESIAN_POINT('Ctrl Pts',(2.2701568454504,0.269372457265854,5.4));
#46275=CARTESIAN_POINT('Ctrl Pts',(2.2701568454504,0.269372457265854,5.37));
#46276=CARTESIAN_POINT('Ctrl Pts',(2.2701568454504,0.328649395704269,5.4));
#46277=CARTESIAN_POINT('Ctrl Pts',(2.2701568454504,0.328649395704269,5.37));
#46278=CARTESIAN_POINT('',(2.23939274251461,0.234856748580933,5.4));
#46279=CARTESIAN_POINT('Ctrl Pts',(2.23939274251461,0.234856748580933,5.4));
#46280=CARTESIAN_POINT('Ctrl Pts',(2.2701568454504,0.269372457265854,5.4));
#46281=CARTESIAN_POINT('Ctrl Pts',(2.2701568454504,0.328649395704269,5.4));
#46282=CARTESIAN_POINT('',(2.23939274251461,0.234856748580933,5.37));
#46283=CARTESIAN_POINT('',(2.23939274251461,0.234856748580933,5.4));
#46284=CARTESIAN_POINT('Ctrl Pts',(2.23939274251461,0.234856748580933,5.37));
#46285=CARTESIAN_POINT('Ctrl Pts',(2.2701568454504,0.269372457265854,5.37));
#46286=CARTESIAN_POINT('Ctrl Pts',(2.2701568454504,0.328649395704269,5.37));
#46287=CARTESIAN_POINT('Ctrl Pts',(2.16585968434811,0.200341069698334,5.4));
#46288=CARTESIAN_POINT('Ctrl Pts',(2.16585968434811,0.200341069698334,5.37));
#46289=CARTESIAN_POINT('Ctrl Pts',(2.20862911641598,0.200341069698334,5.4));
#46290=CARTESIAN_POINT('Ctrl Pts',(2.20862911641598,0.200341069698334,5.37));
#46291=CARTESIAN_POINT('Ctrl Pts',(2.23939274251461,0.234856748580933,5.4));
#46292=CARTESIAN_POINT('Ctrl Pts',(2.23939274251461,0.234856748580933,5.37));
#46293=CARTESIAN_POINT('',(2.16585968434811,0.200341069698334,5.4));
#46294=CARTESIAN_POINT('Ctrl Pts',(2.16585968434811,0.200341069698334,5.4));
#46295=CARTESIAN_POINT('Ctrl Pts',(2.20862911641598,0.200341069698334,5.4));
#46296=CARTESIAN_POINT('Ctrl Pts',(2.23939274251461,0.234856748580933,5.4));
#46297=CARTESIAN_POINT('',(2.16585968434811,0.200341069698334,5.37));
#46298=CARTESIAN_POINT('',(2.16585968434811,0.200341069698334,5.4));
#46299=CARTESIAN_POINT('Ctrl Pts',(2.16585968434811,0.200341069698334,5.37));
#46300=CARTESIAN_POINT('Ctrl Pts',(2.20862911641598,0.200341069698334,5.37));
#46301=CARTESIAN_POINT('Ctrl Pts',(2.23939274251461,0.234856748580933,5.37));
#46302=CARTESIAN_POINT('Ctrl Pts',(2.10995911061764,0.217036151885986,5.4));
#46303=CARTESIAN_POINT('Ctrl Pts',(2.10995911061764,0.217036151885986,5.37));
#46304=CARTESIAN_POINT('Ctrl Pts',(2.13659618794918,0.200341069698334,5.4));
#46305=CARTESIAN_POINT('Ctrl Pts',(2.13659618794918,0.200341069698334,5.37));
#46306=CARTESIAN_POINT('Ctrl Pts',(2.16585968434811,0.200341069698334,5.4));
#46307=CARTESIAN_POINT('Ctrl Pts',(2.16585968434811,0.200341069698334,5.37));
#46308=CARTESIAN_POINT('',(2.10995911061764,0.217036151885986,5.4));
#46309=CARTESIAN_POINT('Ctrl Pts',(2.10995911061764,0.217036151885986,5.4));
#46310=CARTESIAN_POINT('Ctrl Pts',(2.13659618794918,0.200341069698334,5.4));
#46311=CARTESIAN_POINT('Ctrl Pts',(2.16585968434811,0.200341069698334,5.4));
#46312=CARTESIAN_POINT('',(2.10995911061764,0.217036151885986,5.37));
#46313=CARTESIAN_POINT('',(2.10995911061764,0.217036151885986,5.4));
#46314=CARTESIAN_POINT('Ctrl Pts',(2.10995911061764,0.217036151885986,5.37));
#46315=CARTESIAN_POINT('Ctrl Pts',(2.13659618794918,0.200341069698334,5.37));
#46316=CARTESIAN_POINT('Ctrl Pts',(2.16585968434811,0.200341069698334,5.37));
#46317=CARTESIAN_POINT('Ctrl Pts',(2.06850288808346,0.265620732307434,5.4));
#46318=CARTESIAN_POINT('Ctrl Pts',(2.06850288808346,0.265620732307434,5.37));
#46319=CARTESIAN_POINT('Ctrl Pts',(2.08332203328609,0.233731234073639,5.4));
#46320=CARTESIAN_POINT('Ctrl Pts',(2.08332203328609,0.233731234073639,5.37));
#46321=CARTESIAN_POINT('Ctrl Pts',(2.10995911061764,0.217036151885986,5.4));
#46322=CARTESIAN_POINT('Ctrl Pts',(2.10995911061764,0.217036151885986,5.37));
#46323=CARTESIAN_POINT('',(2.06850288808346,0.265620732307434,5.4));
#46324=CARTESIAN_POINT('Ctrl Pts',(2.06850288808346,0.265620732307434,5.4));
#46325=CARTESIAN_POINT('Ctrl Pts',(2.08332203328609,0.233731234073639,5.4));
#46326=CARTESIAN_POINT('Ctrl Pts',(2.10995911061764,0.217036151885986,5.4));
#46327=CARTESIAN_POINT('',(2.06850288808346,0.265620732307434,5.37));
#46328=CARTESIAN_POINT('',(2.06850288808346,0.265620732307434,5.4));
#46329=CARTESIAN_POINT('Ctrl Pts',(2.06850288808346,0.265620732307434,5.37));
#46330=CARTESIAN_POINT('Ctrl Pts',(2.08332203328609,0.233731234073639,5.37));
#46331=CARTESIAN_POINT('Ctrl Pts',(2.10995911061764,0.217036151885986,5.37));
#46332=CARTESIAN_POINT('Ctrl Pts',(2.05368326604366,0.332401105761528,5.4));
#46333=CARTESIAN_POINT('Ctrl Pts',(2.05368326604366,0.332401105761528,5.37));
#46334=CARTESIAN_POINT('Ctrl Pts',(2.05368326604366,0.29751024544239,5.4));
#46335=CARTESIAN_POINT('Ctrl Pts',(2.05368326604366,0.29751024544239,5.37));
#46336=CARTESIAN_POINT('Ctrl Pts',(2.06850288808346,0.265620732307434,5.4));
#46337=CARTESIAN_POINT('Ctrl Pts',(2.06850288808346,0.265620732307434,5.37));
#46338=CARTESIAN_POINT('',(2.05368326604366,0.332401105761528,5.4));
#46339=CARTESIAN_POINT('Ctrl Pts',(2.05368326604366,0.332401105761528,5.4));
#46340=CARTESIAN_POINT('Ctrl Pts',(2.05368326604366,0.29751024544239,5.4));
#46341=CARTESIAN_POINT('Ctrl Pts',(2.06850288808346,0.265620732307434,5.4));
#46342=CARTESIAN_POINT('',(2.05368326604366,0.332401105761528,5.37));
#46343=CARTESIAN_POINT('',(2.05368326604366,0.332401105761528,5.4));
#46344=CARTESIAN_POINT('Ctrl Pts',(2.05368326604366,0.332401105761528,5.37));
#46345=CARTESIAN_POINT('Ctrl Pts',(2.05368326604366,0.29751024544239,5.37));
#46346=CARTESIAN_POINT('Ctrl Pts',(2.06850288808346,0.265620732307434,5.37));
#46347=CARTESIAN_POINT('Ctrl Pts',(2.08557318150997,0.418502742052078,5.4));
#46348=CARTESIAN_POINT('Ctrl Pts',(2.08557318150997,0.418502742052078,5.37));
#46349=CARTESIAN_POINT('Ctrl Pts',(2.05368326604366,0.385675320029259,5.4));
#46350=CARTESIAN_POINT('Ctrl Pts',(2.05368326604366,0.385675320029259,5.37));
#46351=CARTESIAN_POINT('Ctrl Pts',(2.05368326604366,0.332401105761528,5.4));
#46352=CARTESIAN_POINT('Ctrl Pts',(2.05368326604366,0.332401105761528,5.37));
#46353=CARTESIAN_POINT('Ctrl Pts',(2.08557318150997,0.418502742052078,5.4));
#46354=CARTESIAN_POINT('Ctrl Pts',(2.05368326604366,0.385675320029259,5.4));
#46355=CARTESIAN_POINT('Ctrl Pts',(2.05368326604366,0.332401105761528,5.4));
#46356=CARTESIAN_POINT('Ctrl Pts',(2.08557318150997,0.418502742052078,5.37));
#46357=CARTESIAN_POINT('Ctrl Pts',(2.05368326604366,0.385675320029259,5.37));
#46358=CARTESIAN_POINT('Ctrl Pts',(2.05368326604366,0.332401105761528,5.37));
#46359=CARTESIAN_POINT('Ctrl Pts',(2.03492496907711,0.643417501449585,5.4));
#46360=CARTESIAN_POINT('Ctrl Pts',(2.03492496907711,0.643417501449585,5.37));
#46361=CARTESIAN_POINT('Ctrl Pts',(2.08632324635983,0.706446135044098,5.4));
#46362=CARTESIAN_POINT('Ctrl Pts',(2.08632324635983,0.706446135044098,5.37));
#46363=CARTESIAN_POINT('Ctrl Pts',(2.17336271703243,0.706446135044098,5.4));
#46364=CARTESIAN_POINT('Ctrl Pts',(2.17336271703243,0.706446135044098,5.37));
#46365=CARTESIAN_POINT('',(2.03492496907711,0.643417501449585,5.4));
#46366=CARTESIAN_POINT('',(2.17336271703243,0.706446135044098,5.4));
#46367=CARTESIAN_POINT('Ctrl Pts',(2.03492496907711,0.643417501449585,5.4));
#46368=CARTESIAN_POINT('Ctrl Pts',(2.08632324635983,0.706446135044098,5.4));
#46369=CARTESIAN_POINT('Ctrl Pts',(2.17336271703243,0.706446135044098,5.4));
#46370=CARTESIAN_POINT('',(2.03492496907711,0.643417501449585,5.37));
#46371=CARTESIAN_POINT('',(2.03492496907711,0.643417501449585,5.4));
#46372=CARTESIAN_POINT('',(2.17336271703243,0.706446135044098,5.37));
#46373=CARTESIAN_POINT('Ctrl Pts',(2.03492496907711,0.643417501449585,5.37));
#46374=CARTESIAN_POINT('Ctrl Pts',(2.08632324635983,0.706446135044098,5.37));
#46375=CARTESIAN_POINT('Ctrl Pts',(2.17336271703243,0.706446135044098,5.37));
#46376=CARTESIAN_POINT('',(2.17336271703243,0.706446135044098,5.4));
#46377=CARTESIAN_POINT('Ctrl Pts',(1.97602318227291,0.411562079191208,5.4));
#46378=CARTESIAN_POINT('Ctrl Pts',(1.97602318227291,0.411562079191208,5.37));
#46379=CARTESIAN_POINT('Ctrl Pts',(1.97602318227291,0.571009570360184,5.4));
#46380=CARTESIAN_POINT('Ctrl Pts',(1.97602318227291,0.571009570360184,5.37));
#46381=CARTESIAN_POINT('Ctrl Pts',(2.03492496907711,0.643417501449585,5.4));
#46382=CARTESIAN_POINT('Ctrl Pts',(2.03492496907711,0.643417501449585,5.37));
#46383=CARTESIAN_POINT('',(1.97602318227291,0.411562079191208,5.4));
#46384=CARTESIAN_POINT('Ctrl Pts',(1.97602318227291,0.411562079191208,5.4));
#46385=CARTESIAN_POINT('Ctrl Pts',(1.97602318227291,0.571009570360184,5.4));
#46386=CARTESIAN_POINT('Ctrl Pts',(2.03492496907711,0.643417501449585,5.4));
#46387=CARTESIAN_POINT('',(1.97602318227291,0.411562079191208,5.37));
#46388=CARTESIAN_POINT('',(1.97602318227291,0.411562079191208,5.4));
#46389=CARTESIAN_POINT('Ctrl Pts',(1.97602318227291,0.411562079191208,5.37));
#46390=CARTESIAN_POINT('Ctrl Pts',(1.97602318227291,0.571009570360184,5.37));
#46391=CARTESIAN_POINT('Ctrl Pts',(2.03492496907711,0.643417501449585,5.37));
#46392=CARTESIAN_POINT('Ctrl Pts',(2.029297336936,0.206906551122665,5.4));
#46393=CARTESIAN_POINT('Ctrl Pts',(2.029297336936,0.206906551122665,5.37));
#46394=CARTESIAN_POINT('Ctrl Pts',(1.97602318227291,0.268997275829315,5.4));
#46395=CARTESIAN_POINT('Ctrl Pts',(1.97602318227291,0.268997275829315,5.37));
#46396=CARTESIAN_POINT('Ctrl Pts',(1.97602318227291,0.411562079191208,5.4));
#46397=CARTESIAN_POINT('Ctrl Pts',(1.97602318227291,0.411562079191208,5.37));
#46398=CARTESIAN_POINT('',(2.029297336936,0.206906551122665,5.4));
#46399=CARTESIAN_POINT('Ctrl Pts',(2.029297336936,0.206906551122665,5.4));
#46400=CARTESIAN_POINT('Ctrl Pts',(1.97602318227291,0.268997275829315,5.4));
#46401=CARTESIAN_POINT('Ctrl Pts',(1.97602318227291,0.411562079191208,5.4));
#46402=CARTESIAN_POINT('',(2.029297336936,0.206906551122665,5.37));
#46403=CARTESIAN_POINT('',(2.029297336936,0.206906551122665,5.4));
#46404=CARTESIAN_POINT('Ctrl Pts',(2.029297336936,0.206906551122665,5.37));
#46405=CARTESIAN_POINT('Ctrl Pts',(1.97602318227291,0.268997275829315,5.37));
#46406=CARTESIAN_POINT('Ctrl Pts',(1.97602318227291,0.411562079191208,5.37));
#46407=CARTESIAN_POINT('Ctrl Pts',(2.16698502004147,0.144815826416016,5.4));
#46408=CARTESIAN_POINT('Ctrl Pts',(2.16698502004147,0.144815826416016,5.37));
#46409=CARTESIAN_POINT('Ctrl Pts',(2.08257149159908,0.144815826416016,5.4));
#46410=CARTESIAN_POINT('Ctrl Pts',(2.08257149159908,0.144815826416016,5.37));
#46411=CARTESIAN_POINT('Ctrl Pts',(2.029297336936,0.206906551122665,5.4));
#46412=CARTESIAN_POINT('Ctrl Pts',(2.029297336936,0.206906551122665,5.37));
#46413=CARTESIAN_POINT('',(2.16698502004147,0.144815826416016,5.4));
#46414=CARTESIAN_POINT('Ctrl Pts',(2.16698502004147,0.144815826416016,5.4));
#46415=CARTESIAN_POINT('Ctrl Pts',(2.08257149159908,0.144815826416016,5.4));
#46416=CARTESIAN_POINT('Ctrl Pts',(2.029297336936,0.206906551122665,5.4));
#46417=CARTESIAN_POINT('',(2.16698502004147,0.144815826416016,5.37));
#46418=CARTESIAN_POINT('',(2.16698502004147,0.144815826416016,5.4));
#46419=CARTESIAN_POINT('Ctrl Pts',(2.16698502004147,0.144815826416016,5.37));
#46420=CARTESIAN_POINT('Ctrl Pts',(2.08257149159908,0.144815826416016,5.37));
#46421=CARTESIAN_POINT('Ctrl Pts',(2.029297336936,0.206906551122665,5.37));
#46422=CARTESIAN_POINT('Ctrl Pts',(2.25552509725094,0.168451571464539,5.4));
#46423=CARTESIAN_POINT('Ctrl Pts',(2.25552509725094,0.168451571464539,5.37));
#46424=CARTESIAN_POINT('Ctrl Pts',(2.21650741994381,0.144815826416016,5.4));
#46425=CARTESIAN_POINT('Ctrl Pts',(2.21650741994381,0.144815826416016,5.37));
#46426=CARTESIAN_POINT('Ctrl Pts',(2.16698502004147,0.144815826416016,5.4));
#46427=CARTESIAN_POINT('Ctrl Pts',(2.16698502004147,0.144815826416016,5.37));
#46428=CARTESIAN_POINT('',(2.25552509725094,0.168451571464539,5.4));
#46429=CARTESIAN_POINT('Ctrl Pts',(2.25552509725094,0.168451571464539,5.4));
#46430=CARTESIAN_POINT('Ctrl Pts',(2.21650741994381,0.144815826416016,5.4));
#46431=CARTESIAN_POINT('Ctrl Pts',(2.16698502004147,0.144815826416016,5.4));
#46432=CARTESIAN_POINT('',(2.25552509725094,0.168451571464539,5.37));
#46433=CARTESIAN_POINT('',(2.25552509725094,0.168451571464539,5.4));
#46434=CARTESIAN_POINT('Ctrl Pts',(2.25552509725094,0.168451571464539,5.37));
#46435=CARTESIAN_POINT('Ctrl Pts',(2.21650741994381,0.144815826416016,5.37));
#46436=CARTESIAN_POINT('Ctrl Pts',(2.16698502004147,0.144815826416016,5.37));
#46437=CARTESIAN_POINT('Ctrl Pts',(2.31686542928219,0.236545050144196,5.4));
#46438=CARTESIAN_POINT('Ctrl Pts',(2.31686542928219,0.236545050144196,5.37));
#46439=CARTESIAN_POINT('Ctrl Pts',(2.29454277455807,0.192087316513062,5.4));
#46440=CARTESIAN_POINT('Ctrl Pts',(2.29454277455807,0.192087316513062,5.37));
#46441=CARTESIAN_POINT('Ctrl Pts',(2.25552509725094,0.168451571464539,5.4));
#46442=CARTESIAN_POINT('Ctrl Pts',(2.25552509725094,0.168451571464539,5.37));
#46443=CARTESIAN_POINT('',(2.31686542928219,0.236545050144196,5.4));
#46444=CARTESIAN_POINT('Ctrl Pts',(2.31686542928219,0.236545050144196,5.4));
#46445=CARTESIAN_POINT('Ctrl Pts',(2.29454277455807,0.192087316513062,5.4));
#46446=CARTESIAN_POINT('Ctrl Pts',(2.25552509725094,0.168451571464539,5.4));
#46447=CARTESIAN_POINT('',(2.31686542928219,0.236545050144196,5.37));
#46448=CARTESIAN_POINT('',(2.31686542928219,0.236545050144196,5.4));
#46449=CARTESIAN_POINT('Ctrl Pts',(2.31686542928219,0.236545050144196,5.37));
#46450=CARTESIAN_POINT('Ctrl Pts',(2.29454277455807,0.192087316513062,5.37));
#46451=CARTESIAN_POINT('Ctrl Pts',(2.25552509725094,0.168451571464539,5.37));
#46452=CARTESIAN_POINT('Ctrl Pts',(2.33918808400631,0.332776272296906,5.4));
#46453=CARTESIAN_POINT('Ctrl Pts',(2.33918808400631,0.332776272296906,5.37));
#46454=CARTESIAN_POINT('Ctrl Pts',(2.33918808400631,0.281002724170685,5.4));
#46455=CARTESIAN_POINT('Ctrl Pts',(2.33918808400631,0.281002724170685,5.37));
#46456=CARTESIAN_POINT('Ctrl Pts',(2.31686542928219,0.236545050144196,5.4));
#46457=CARTESIAN_POINT('Ctrl Pts',(2.31686542928219,0.236545050144196,5.37));
#46458=CARTESIAN_POINT('',(2.33918808400631,0.332776272296906,5.4));
#46459=CARTESIAN_POINT('Ctrl Pts',(2.33918808400631,0.332776272296906,5.4));
#46460=CARTESIAN_POINT('Ctrl Pts',(2.33918808400631,0.281002724170685,5.4));
#46461=CARTESIAN_POINT('Ctrl Pts',(2.31686542928219,0.236545050144196,5.4));
#46462=CARTESIAN_POINT('',(2.33918808400631,0.332776272296906,5.37));
#46463=CARTESIAN_POINT('',(2.33918808400631,0.332776272296906,5.4));
#46464=CARTESIAN_POINT('Ctrl Pts',(2.33918808400631,0.332776272296906,5.37));
#46465=CARTESIAN_POINT('Ctrl Pts',(2.33918808400631,0.281002724170685,5.37));
#46466=CARTESIAN_POINT('Ctrl Pts',(2.31686542928219,0.236545050144196,5.37));
#46467=CARTESIAN_POINT('Ctrl Pts',(2.29172895848751,0.461272174119949,5.4));
#46468=CARTESIAN_POINT('Ctrl Pts',(2.29172895848751,0.461272174119949,5.37));
#46469=CARTESIAN_POINT('Ctrl Pts',(2.33918808400631,0.411562079191208,5.4));
#46470=CARTESIAN_POINT('Ctrl Pts',(2.33918808400631,0.411562079191208,5.37));
#46471=CARTESIAN_POINT('Ctrl Pts',(2.33918808400631,0.332776272296906,5.4));
#46472=CARTESIAN_POINT('Ctrl Pts',(2.33918808400631,0.332776272296906,5.37));
#46473=CARTESIAN_POINT('',(2.29172895848751,0.461272174119949,5.4));
#46474=CARTESIAN_POINT('Ctrl Pts',(2.29172895848751,0.461272174119949,5.4));
#46475=CARTESIAN_POINT('Ctrl Pts',(2.33918808400631,0.411562079191208,5.4));
#46476=CARTESIAN_POINT('Ctrl Pts',(2.33918808400631,0.332776272296906,5.4));
#46477=CARTESIAN_POINT('',(2.29172895848751,0.461272174119949,5.37));
#46478=CARTESIAN_POINT('',(2.29172895848751,0.461272174119949,5.4));
#46479=CARTESIAN_POINT('Ctrl Pts',(2.29172895848751,0.461272174119949,5.37));
#46480=CARTESIAN_POINT('Ctrl Pts',(2.33918808400631,0.411562079191208,5.37));
#46481=CARTESIAN_POINT('Ctrl Pts',(2.33918808400631,0.332776272296906,5.37));
#46482=CARTESIAN_POINT('Ctrl Pts',(2.17673920094967,0.510982298851013,5.4));
#46483=CARTESIAN_POINT('Ctrl Pts',(2.17673920094967,0.510982298851013,5.37));
#46484=CARTESIAN_POINT('Ctrl Pts',(2.24427030980587,0.510982298851013,5.4));
#46485=CARTESIAN_POINT('Ctrl Pts',(2.24427030980587,0.510982298851013,5.37));
#46486=CARTESIAN_POINT('Ctrl Pts',(2.29172895848751,0.461272174119949,5.4));
#46487=CARTESIAN_POINT('Ctrl Pts',(2.29172895848751,0.461272174119949,5.37));
#46488=CARTESIAN_POINT('',(2.17673920094967,0.510982298851013,5.4));
#46489=CARTESIAN_POINT('Ctrl Pts',(2.17673920094967,0.510982298851013,5.4));
#46490=CARTESIAN_POINT('Ctrl Pts',(2.24427030980587,0.510982298851013,5.4));
#46491=CARTESIAN_POINT('Ctrl Pts',(2.29172895848751,0.461272174119949,5.4));
#46492=CARTESIAN_POINT('',(2.17673920094967,0.510982298851013,5.37));
#46493=CARTESIAN_POINT('',(2.17673920094967,0.510982298851013,5.4));
#46494=CARTESIAN_POINT('Ctrl Pts',(2.17673920094967,0.510982298851013,5.37));
#46495=CARTESIAN_POINT('Ctrl Pts',(2.24427030980587,0.510982298851013,5.37));
#46496=CARTESIAN_POINT('Ctrl Pts',(2.29172895848751,0.461272174119949,5.37));
#46497=CARTESIAN_POINT('Ctrl Pts',(2.10283087193966,0.492974096536636,5.4));
#46498=CARTESIAN_POINT('Ctrl Pts',(2.10283087193966,0.492974096536636,5.37));
#46499=CARTESIAN_POINT('Ctrl Pts',(2.13809679448605,0.510982298851013,5.4));
#46500=CARTESIAN_POINT('Ctrl Pts',(2.13809679448605,0.510982298851013,5.37));
#46501=CARTESIAN_POINT('Ctrl Pts',(2.17673920094967,0.510982298851013,5.4));
#46502=CARTESIAN_POINT('Ctrl Pts',(2.17673920094967,0.510982298851013,5.37));
#46503=CARTESIAN_POINT('',(2.10283087193966,0.492974096536636,5.4));
#46504=CARTESIAN_POINT('Ctrl Pts',(2.10283087193966,0.492974096536636,5.4));
#46505=CARTESIAN_POINT('Ctrl Pts',(2.13809679448605,0.510982298851013,5.4));
#46506=CARTESIAN_POINT('Ctrl Pts',(2.17673920094967,0.510982298851013,5.4));
#46507=CARTESIAN_POINT('',(2.10283087193966,0.492974096536636,5.37));
#46508=CARTESIAN_POINT('',(2.10283087193966,0.492974096536636,5.4));
#46509=CARTESIAN_POINT('Ctrl Pts',(2.10283087193966,0.492974096536636,5.37));
#46510=CARTESIAN_POINT('Ctrl Pts',(2.13809679448605,0.510982298851013,5.37));
#46511=CARTESIAN_POINT('Ctrl Pts',(2.17673920094967,0.510982298851013,5.37));
#46512=CARTESIAN_POINT('Ctrl Pts',(2.04317854344845,0.437824034690857,5.4));
#46513=CARTESIAN_POINT('Ctrl Pts',(2.04317854344845,0.437824034690857,5.37));
#46514=CARTESIAN_POINT('Ctrl Pts',(2.06756494939327,0.474965924024582,5.4));
#46515=CARTESIAN_POINT('Ctrl Pts',(2.06756494939327,0.474965924024582,5.37));
#46516=CARTESIAN_POINT('Ctrl Pts',(2.10283087193966,0.492974096536636,5.4));
#46517=CARTESIAN_POINT('Ctrl Pts',(2.10283087193966,0.492974096536636,5.37));
#46518=CARTESIAN_POINT('',(2.04317854344845,0.437824034690857,5.4));
#46519=CARTESIAN_POINT('Ctrl Pts',(2.04317854344845,0.437824034690857,5.4));
#46520=CARTESIAN_POINT('Ctrl Pts',(2.06756494939327,0.474965924024582,5.4));
#46521=CARTESIAN_POINT('Ctrl Pts',(2.10283087193966,0.492974096536636,5.4));
#46522=CARTESIAN_POINT('',(2.04317854344845,0.437824034690857,5.37));
#46523=CARTESIAN_POINT('',(2.04317854344845,0.437824034690857,5.4));
#46524=CARTESIAN_POINT('Ctrl Pts',(2.04317854344845,0.437824034690857,5.37));
#46525=CARTESIAN_POINT('Ctrl Pts',(2.06756494939327,0.474965924024582,5.37));
#46526=CARTESIAN_POINT('Ctrl Pts',(2.10283087193966,0.492974096536636,5.37));
#46527=CARTESIAN_POINT('Ctrl Pts',(2.06231258809566,0.565006846189499,5.4));
#46528=CARTESIAN_POINT('Ctrl Pts',(2.06231258809566,0.565006846189499,5.37));
#46529=CARTESIAN_POINT('Ctrl Pts',(2.04392908513546,0.520361536741257,5.4));
#46530=CARTESIAN_POINT('Ctrl Pts',(2.04392908513546,0.520361536741257,5.37));
#46531=CARTESIAN_POINT('Ctrl Pts',(2.04317854344845,0.437824034690857,5.4));
#46532=CARTESIAN_POINT('Ctrl Pts',(2.04317854344845,0.437824034690857,5.37));
#46533=CARTESIAN_POINT('',(2.06231258809566,0.565006846189499,5.4));
#46534=CARTESIAN_POINT('Ctrl Pts',(2.06231258809566,0.565006846189499,5.4));
#46535=CARTESIAN_POINT('Ctrl Pts',(2.04392908513546,0.520361536741257,5.4));
#46536=CARTESIAN_POINT('Ctrl Pts',(2.04317854344845,0.437824034690857,5.4));
#46537=CARTESIAN_POINT('',(2.06231258809566,0.565006846189499,5.37));
#46538=CARTESIAN_POINT('',(2.06231258809566,0.565006846189499,5.4));
#46539=CARTESIAN_POINT('Ctrl Pts',(2.06231258809566,0.565006846189499,5.37));
#46540=CARTESIAN_POINT('Ctrl Pts',(2.04392908513546,0.520361536741257,5.37));
#46541=CARTESIAN_POINT('Ctrl Pts',(2.04317854344845,0.437824034690857,5.37));
#46542=CARTESIAN_POINT('Ctrl Pts',(2.11258505284786,0.632912719249725,5.4));
#46543=CARTESIAN_POINT('Ctrl Pts',(2.11258505284786,0.632912719249725,5.37));
#46544=CARTESIAN_POINT('Ctrl Pts',(2.08069561421871,0.609652125835419,5.4));
#46545=CARTESIAN_POINT('Ctrl Pts',(2.08069561421871,0.609652125835419,5.37));
#46546=CARTESIAN_POINT('Ctrl Pts',(2.06231258809566,0.565006846189499,5.4));
#46547=CARTESIAN_POINT('Ctrl Pts',(2.06231258809566,0.565006846189499,5.37));
#46548=CARTESIAN_POINT('',(2.11258505284786,0.632912719249725,5.4));
#46549=CARTESIAN_POINT('Ctrl Pts',(2.11258505284786,0.632912719249725,5.4));
#46550=CARTESIAN_POINT('Ctrl Pts',(2.08069561421871,0.609652125835419,5.4));
#46551=CARTESIAN_POINT('Ctrl Pts',(2.06231258809566,0.565006846189499,5.4));
#46552=CARTESIAN_POINT('',(2.11258505284786,0.632912719249725,5.37));
#46553=CARTESIAN_POINT('',(2.11258505284786,0.632912719249725,5.4));
#46554=CARTESIAN_POINT('Ctrl Pts',(2.11258505284786,0.632912719249725,5.37));
#46555=CARTESIAN_POINT('Ctrl Pts',(2.08069561421871,0.609652125835419,5.37));
#46556=CARTESIAN_POINT('Ctrl Pts',(2.06231258809566,0.565006846189499,5.37));
#46557=CARTESIAN_POINT('Ctrl Pts',(2.16923616826534,0.65092089176178,5.4));
#46558=CARTESIAN_POINT('Ctrl Pts',(2.16923616826534,0.65092089176178,5.37));
#46559=CARTESIAN_POINT('Ctrl Pts',(2.13697145879269,0.65092089176178,5.4));
#46560=CARTESIAN_POINT('Ctrl Pts',(2.13697145879269,0.65092089176178,5.37));
#46561=CARTESIAN_POINT('Ctrl Pts',(2.11258505284786,0.632912719249725,5.4));
#46562=CARTESIAN_POINT('Ctrl Pts',(2.11258505284786,0.632912719249725,5.37));
#46563=CARTESIAN_POINT('',(2.16923616826534,0.65092089176178,5.4));
#46564=CARTESIAN_POINT('Ctrl Pts',(2.16923616826534,0.65092089176178,5.4));
#46565=CARTESIAN_POINT('Ctrl Pts',(2.13697145879269,0.65092089176178,5.4));
#46566=CARTESIAN_POINT('Ctrl Pts',(2.11258505284786,0.632912719249725,5.4));
#46567=CARTESIAN_POINT('',(2.16923616826534,0.65092089176178,5.37));
#46568=CARTESIAN_POINT('',(2.16923616826534,0.65092089176178,5.4));
#46569=CARTESIAN_POINT('Ctrl Pts',(2.16923616826534,0.65092089176178,5.37));
#46570=CARTESIAN_POINT('Ctrl Pts',(2.13697145879269,0.65092089176178,5.37));
#46571=CARTESIAN_POINT('Ctrl Pts',(2.11258505284786,0.632912719249725,5.37));
#46572=CARTESIAN_POINT('Ctrl Pts',(2.23676680028439,0.622032755613327,5.4));
#46573=CARTESIAN_POINT('Ctrl Pts',(2.23676680028439,0.622032755613327,5.37));
#46574=CARTESIAN_POINT('Ctrl Pts',(2.20937918126583,0.65092089176178,5.4));
#46575=CARTESIAN_POINT('Ctrl Pts',(2.20937918126583,0.65092089176178,5.37));
#46576=CARTESIAN_POINT('Ctrl Pts',(2.16923616826534,0.65092089176178,5.4));
#46577=CARTESIAN_POINT('Ctrl Pts',(2.16923616826534,0.65092089176178,5.37));
#46578=CARTESIAN_POINT('',(2.23676680028439,0.622032755613327,5.4));
#46579=CARTESIAN_POINT('Ctrl Pts',(2.23676680028439,0.622032755613327,5.4));
#46580=CARTESIAN_POINT('Ctrl Pts',(2.20937918126583,0.65092089176178,5.4));
#46581=CARTESIAN_POINT('Ctrl Pts',(2.16923616826534,0.65092089176178,5.4));
#46582=CARTESIAN_POINT('',(2.23676680028439,0.622032755613327,5.37));
#46583=CARTESIAN_POINT('',(2.23676680028439,0.622032755613327,5.4));
#46584=CARTESIAN_POINT('Ctrl Pts',(2.23676680028439,0.622032755613327,5.37));
#46585=CARTESIAN_POINT('Ctrl Pts',(2.20937918126583,0.65092089176178,5.37));
#46586=CARTESIAN_POINT('Ctrl Pts',(2.16923616826534,0.65092089176178,5.37));
#46587=CARTESIAN_POINT('Ctrl Pts',(2.26227854192257,0.564256513118744,5.4));
#46588=CARTESIAN_POINT('Ctrl Pts',(2.26227854192257,0.564256513118744,5.37));
#46589=CARTESIAN_POINT('Ctrl Pts',(2.25327442586422,0.604024583101273,5.4));
#46590=CARTESIAN_POINT('Ctrl Pts',(2.25327442586422,0.604024583101273,5.37));
#46591=CARTESIAN_POINT('Ctrl Pts',(2.23676680028439,0.622032755613327,5.4));
#46592=CARTESIAN_POINT('Ctrl Pts',(2.23676680028439,0.622032755613327,5.37));
#46593=CARTESIAN_POINT('',(2.26227854192257,0.564256513118744,5.4));
#46594=CARTESIAN_POINT('Ctrl Pts',(2.26227854192257,0.564256513118744,5.4));
#46595=CARTESIAN_POINT('Ctrl Pts',(2.25327442586422,0.604024583101273,5.4));
#46596=CARTESIAN_POINT('Ctrl Pts',(2.23676680028439,0.622032755613327,5.4));
#46597=CARTESIAN_POINT('',(2.26227854192257,0.564256513118744,5.37));
#46598=CARTESIAN_POINT('',(2.26227854192257,0.564256513118744,5.4));
#46599=CARTESIAN_POINT('Ctrl Pts',(2.26227854192257,0.564256513118744,5.37));
#46600=CARTESIAN_POINT('Ctrl Pts',(2.25327442586422,0.604024583101273,5.37));
#46601=CARTESIAN_POINT('Ctrl Pts',(2.23676680028439,0.622032755613327,5.37));
#46602=CARTESIAN_POINT('Origin',(2.32943390309811,0.569508904218674,5.4));
#46603=CARTESIAN_POINT('',(2.32943390309811,0.569508904218674,5.4));
#46604=CARTESIAN_POINT('',(1.14966248238161,0.477235989567443,5.4));
#46605=CARTESIAN_POINT('',(2.32943390309811,0.569508904218674,5.37));
#46606=CARTESIAN_POINT('',(2.32943390309811,0.569508904218674,5.4));
#46607=CARTESIAN_POINT('',(2.32943390309811,0.569508904218674,5.37));
#46608=CARTESIAN_POINT('Ctrl Pts',(2.27972362935543,0.670054578781128,5.4));
#46609=CARTESIAN_POINT('Ctrl Pts',(2.27972362935543,0.670054578781128,5.37));
#46610=CARTESIAN_POINT('Ctrl Pts',(2.32118032872677,0.63366305232048,5.4));
#46611=CARTESIAN_POINT('Ctrl Pts',(2.32118032872677,0.63366305232048,5.37));
#46612=CARTESIAN_POINT('Ctrl Pts',(2.32943390309811,0.569508904218674,5.4));
#46613=CARTESIAN_POINT('Ctrl Pts',(2.32943390309811,0.569508904218674,5.37));
#46614=CARTESIAN_POINT('',(2.27972362935543,0.670054578781128,5.4));
#46615=CARTESIAN_POINT('Ctrl Pts',(2.27972362935543,0.670054578781128,5.4));
#46616=CARTESIAN_POINT('Ctrl Pts',(2.32118032872677,0.63366305232048,5.4));
#46617=CARTESIAN_POINT('Ctrl Pts',(2.32943390309811,0.569508904218674,5.4));
#46618=CARTESIAN_POINT('',(2.27972362935543,0.670054578781128,5.37));
#46619=CARTESIAN_POINT('',(2.27972362935543,0.670054578781128,5.4));
#46620=CARTESIAN_POINT('Ctrl Pts',(2.27972362935543,0.670054578781128,5.37));
#46621=CARTESIAN_POINT('Ctrl Pts',(2.32118032872677,0.63366305232048,5.37));
#46622=CARTESIAN_POINT('Ctrl Pts',(2.32943390309811,0.569508904218674,5.37));
#46623=CARTESIAN_POINT('Ctrl Pts',(2.17336271703243,0.706446135044098,5.4));
#46624=CARTESIAN_POINT('Ctrl Pts',(2.17336271703243,0.706446135044098,5.37));
#46625=CARTESIAN_POINT('Ctrl Pts',(2.23826740682125,0.706446135044098,5.4));
#46626=CARTESIAN_POINT('Ctrl Pts',(2.23826740682125,0.706446135044098,5.37));
#46627=CARTESIAN_POINT('Ctrl Pts',(2.27972362935543,0.670054578781128,5.4));
#46628=CARTESIAN_POINT('Ctrl Pts',(2.27972362935543,0.670054578781128,5.37));
#46629=CARTESIAN_POINT('Ctrl Pts',(2.17336271703243,0.706446135044098,5.4));
#46630=CARTESIAN_POINT('Ctrl Pts',(2.23826740682125,0.706446135044098,5.4));
#46631=CARTESIAN_POINT('Ctrl Pts',(2.27972362935543,0.670054578781128,5.4));
#46632=CARTESIAN_POINT('Ctrl Pts',(2.17336271703243,0.706446135044098,5.37));
#46633=CARTESIAN_POINT('Ctrl Pts',(2.23826740682125,0.706446135044098,5.37));
#46634=CARTESIAN_POINT('Ctrl Pts',(2.27972362935543,0.670054578781128,5.37));
#46635=CARTESIAN_POINT('Origin',(2.15760563313961,0.425630980730057,5.37));
#46636=CARTESIAN_POINT('Ctrl Pts',(-0.344406619668007,-0.352285182476044,
5.4));
#46637=CARTESIAN_POINT('Ctrl Pts',(-0.344406619668007,-0.352285182476044,
5.37));
#46638=CARTESIAN_POINT('Ctrl Pts',(-0.388676658272743,-0.352285182476044,
5.4));
#46639=CARTESIAN_POINT('Ctrl Pts',(-0.388676658272743,-0.352285182476044,
5.37));
#46640=CARTESIAN_POINT('Ctrl Pts',(-0.420941367745399,-0.390740191936493,
5.4));
#46641=CARTESIAN_POINT('Ctrl Pts',(-0.420941367745399,-0.390740191936493,
5.37));
#46642=CARTESIAN_POINT('',(-0.344406619668007,-0.352285182476044,5.4));
#46643=CARTESIAN_POINT('',(-0.420941367745399,-0.390740191936493,5.4));
#46644=CARTESIAN_POINT('Ctrl Pts',(-0.344406619668007,-0.352285182476044,
5.4));
#46645=CARTESIAN_POINT('Ctrl Pts',(-0.388676658272743,-0.352285182476044,
5.4));
#46646=CARTESIAN_POINT('Ctrl Pts',(-0.420941367745399,-0.390740191936493,
5.4));
#46647=CARTESIAN_POINT('',(-0.344406619668007,-0.352285182476044,5.37));
#46648=CARTESIAN_POINT('',(-0.344406619668007,-0.352285182476044,5.4));
#46649=CARTESIAN_POINT('',(-0.420941367745399,-0.390740191936493,5.37));
#46650=CARTESIAN_POINT('Ctrl Pts',(-0.344406619668007,-0.352285182476044,
5.37));
#46651=CARTESIAN_POINT('Ctrl Pts',(-0.388676658272743,-0.352285182476044,
5.37));
#46652=CARTESIAN_POINT('Ctrl Pts',(-0.420941367745399,-0.390740191936493,
5.37));
#46653=CARTESIAN_POINT('',(-0.420941367745399,-0.390740191936493,5.4));
#46654=CARTESIAN_POINT('Ctrl Pts',(-0.269560113549232,-0.389427101612091,
5.4));
#46655=CARTESIAN_POINT('Ctrl Pts',(-0.269560113549232,-0.389427101612091,
5.37));
#46656=CARTESIAN_POINT('Ctrl Pts',(-0.300511613488197,-0.352285182476044,
5.4));
#46657=CARTESIAN_POINT('Ctrl Pts',(-0.300511613488197,-0.352285182476044,
5.37));
#46658=CARTESIAN_POINT('Ctrl Pts',(-0.344406619668007,-0.352285182476044,
5.4));
#46659=CARTESIAN_POINT('Ctrl Pts',(-0.344406619668007,-0.352285182476044,
5.37));
#46660=CARTESIAN_POINT('',(-0.269560113549232,-0.389427101612091,5.4));
#46661=CARTESIAN_POINT('Ctrl Pts',(-0.269560113549232,-0.389427101612091,
5.4));
#46662=CARTESIAN_POINT('Ctrl Pts',(-0.300511613488197,-0.352285182476044,
5.4));
#46663=CARTESIAN_POINT('Ctrl Pts',(-0.344406619668007,-0.352285182476044,
5.4));
#46664=CARTESIAN_POINT('',(-0.269560113549232,-0.389427101612091,5.37));
#46665=CARTESIAN_POINT('',(-0.269560113549232,-0.389427101612091,5.4));
#46666=CARTESIAN_POINT('Ctrl Pts',(-0.269560113549232,-0.389427101612091,
5.37));
#46667=CARTESIAN_POINT('Ctrl Pts',(-0.300511613488197,-0.352285182476044,
5.37));
#46668=CARTESIAN_POINT('Ctrl Pts',(-0.344406619668007,-0.352285182476044,
5.37));
#46669=CARTESIAN_POINT('Ctrl Pts',(-0.238608375191689,-0.504604494571686,
5.4));
#46670=CARTESIAN_POINT('Ctrl Pts',(-0.238608375191689,-0.504604494571686,
5.37));
#46671=CARTESIAN_POINT('Ctrl Pts',(-0.238608375191689,-0.426568961143494,
5.4));
#46672=CARTESIAN_POINT('Ctrl Pts',(-0.238608375191689,-0.426568961143494,
5.37));
#46673=CARTESIAN_POINT('Ctrl Pts',(-0.269560113549232,-0.389427101612091,
5.4));
#46674=CARTESIAN_POINT('Ctrl Pts',(-0.269560113549232,-0.389427101612091,
5.37));
#46675=CARTESIAN_POINT('',(-0.238608375191689,-0.504604494571686,5.4));
#46676=CARTESIAN_POINT('Ctrl Pts',(-0.238608375191689,-0.504604494571686,
5.4));
#46677=CARTESIAN_POINT('Ctrl Pts',(-0.238608375191689,-0.426568961143494,
5.4));
#46678=CARTESIAN_POINT('Ctrl Pts',(-0.269560113549232,-0.389427101612091,
5.4));
#46679=CARTESIAN_POINT('',(-0.238608375191689,-0.504604494571686,5.37));
#46680=CARTESIAN_POINT('',(-0.238608375191689,-0.504604494571686,5.4));
#46681=CARTESIAN_POINT('Ctrl Pts',(-0.238608375191689,-0.504604494571686,
5.37));
#46682=CARTESIAN_POINT('Ctrl Pts',(-0.238608375191689,-0.426568961143494,
5.37));
#46683=CARTESIAN_POINT('Ctrl Pts',(-0.269560113549232,-0.389427101612091,
5.37));
#46684=CARTESIAN_POINT('Ctrl Pts',(-0.270873084664345,-0.619219100475311,
5.4));
#46685=CARTESIAN_POINT('Ctrl Pts',(-0.270873084664345,-0.619219100475311,
5.37));
#46686=CARTESIAN_POINT('Ctrl Pts',(-0.238608375191689,-0.580764091014862,
5.4));
#46687=CARTESIAN_POINT('Ctrl Pts',(-0.238608375191689,-0.580764091014862,
5.37));
#46688=CARTESIAN_POINT('Ctrl Pts',(-0.238608375191689,-0.504604494571686,
5.4));
#46689=CARTESIAN_POINT('Ctrl Pts',(-0.238608375191689,-0.504604494571686,
5.37));
#46690=CARTESIAN_POINT('',(-0.270873084664345,-0.619219100475311,5.4));
#46691=CARTESIAN_POINT('Ctrl Pts',(-0.270873084664345,-0.619219100475311,
5.4));
#46692=CARTESIAN_POINT('Ctrl Pts',(-0.238608375191689,-0.580764091014862,
5.4));
#46693=CARTESIAN_POINT('Ctrl Pts',(-0.238608375191689,-0.504604494571686,
5.4));
#46694=CARTESIAN_POINT('',(-0.270873084664345,-0.619219100475311,5.37));
#46695=CARTESIAN_POINT('',(-0.270873084664345,-0.619219100475311,5.4));
#46696=CARTESIAN_POINT('Ctrl Pts',(-0.270873084664345,-0.619219100475311,
5.37));
#46697=CARTESIAN_POINT('Ctrl Pts',(-0.238608375191689,-0.580764091014862,
5.37));
#46698=CARTESIAN_POINT('Ctrl Pts',(-0.238608375191689,-0.504604494571686,
5.37));
#46699=CARTESIAN_POINT('Ctrl Pts',(-0.347407832741737,-0.657673990726471,
5.4));
#46700=CARTESIAN_POINT('Ctrl Pts',(-0.347407832741737,-0.657673990726471,
5.37));
#46701=CARTESIAN_POINT('Ctrl Pts',(-0.303137794137001,-0.657673990726471,
5.4));
#46702=CARTESIAN_POINT('Ctrl Pts',(-0.303137794137001,-0.657673990726471,
5.37));
#46703=CARTESIAN_POINT('Ctrl Pts',(-0.270873084664345,-0.619219100475311,
5.4));
#46704=CARTESIAN_POINT('Ctrl Pts',(-0.270873084664345,-0.619219100475311,
5.37));
#46705=CARTESIAN_POINT('',(-0.347407832741737,-0.657673990726471,5.4));
#46706=CARTESIAN_POINT('Ctrl Pts',(-0.347407832741737,-0.657673990726471,
5.4));
#46707=CARTESIAN_POINT('Ctrl Pts',(-0.303137794137001,-0.657673990726471,
5.4));
#46708=CARTESIAN_POINT('Ctrl Pts',(-0.270873084664345,-0.619219100475311,
5.4));
#46709=CARTESIAN_POINT('',(-0.347407832741737,-0.657673990726471,5.37));
#46710=CARTESIAN_POINT('',(-0.347407832741737,-0.657673990726471,5.4));
#46711=CARTESIAN_POINT('Ctrl Pts',(-0.347407832741737,-0.657673990726471,
5.37));
#46712=CARTESIAN_POINT('Ctrl Pts',(-0.303137794137001,-0.657673990726471,
5.37));
#46713=CARTESIAN_POINT('Ctrl Pts',(-0.270873084664345,-0.619219100475311,
5.37));
#46714=CARTESIAN_POINT('Ctrl Pts',(-0.433697238564491,-0.605525290966034,
5.4));
#46715=CARTESIAN_POINT('Ctrl Pts',(-0.433697238564491,-0.605525290966034,
5.37));
#46716=CARTESIAN_POINT('Ctrl Pts',(-0.401807561516762,-0.657673990726471,
5.4));
#46717=CARTESIAN_POINT('Ctrl Pts',(-0.401807561516762,-0.657673990726471,
5.37));
#46718=CARTESIAN_POINT('Ctrl Pts',(-0.347407832741737,-0.657673990726471,
5.4));
#46719=CARTESIAN_POINT('Ctrl Pts',(-0.347407832741737,-0.657673990726471,
5.37));
#46720=CARTESIAN_POINT('',(-0.433697238564491,-0.605525290966034,5.4));
#46721=CARTESIAN_POINT('Ctrl Pts',(-0.433697238564491,-0.605525290966034,
5.4));
#46722=CARTESIAN_POINT('Ctrl Pts',(-0.401807561516762,-0.657673990726471,
5.4));
#46723=CARTESIAN_POINT('Ctrl Pts',(-0.347407832741737,-0.657673990726471,
5.4));
#46724=CARTESIAN_POINT('',(-0.433697238564491,-0.605525290966034,5.37));
#46725=CARTESIAN_POINT('',(-0.433697238564491,-0.605525290966034,5.4));
#46726=CARTESIAN_POINT('Ctrl Pts',(-0.433697238564491,-0.605525290966034,
5.37));
#46727=CARTESIAN_POINT('Ctrl Pts',(-0.401807561516762,-0.657673990726471,
5.37));
#46728=CARTESIAN_POINT('Ctrl Pts',(-0.347407832741737,-0.657673990726471,
5.37));
#46729=CARTESIAN_POINT('Ctrl Pts',(-0.453206077218056,-0.501978313922882,
5.4));
#46730=CARTESIAN_POINT('Ctrl Pts',(-0.453206077218056,-0.501978313922882,
5.37));
#46731=CARTESIAN_POINT('Ctrl Pts',(-0.453206077218056,-0.573635852336884,
5.4));
#46732=CARTESIAN_POINT('Ctrl Pts',(-0.453206077218056,-0.573635852336884,
5.37));
#46733=CARTESIAN_POINT('Ctrl Pts',(-0.433697238564491,-0.605525290966034,
5.4));
#46734=CARTESIAN_POINT('Ctrl Pts',(-0.433697238564491,-0.605525290966034,
5.37));
#46735=CARTESIAN_POINT('',(-0.453206077218056,-0.501978313922882,5.4));
#46736=CARTESIAN_POINT('Ctrl Pts',(-0.453206077218056,-0.501978313922882,
5.4));
#46737=CARTESIAN_POINT('Ctrl Pts',(-0.453206077218056,-0.573635852336884,
5.4));
#46738=CARTESIAN_POINT('Ctrl Pts',(-0.433697238564491,-0.605525290966034,
5.4));
#46739=CARTESIAN_POINT('',(-0.453206077218056,-0.501978313922882,5.37));
#46740=CARTESIAN_POINT('',(-0.453206077218056,-0.501978313922882,5.4));
#46741=CARTESIAN_POINT('Ctrl Pts',(-0.453206077218056,-0.501978313922882,
5.37));
#46742=CARTESIAN_POINT('Ctrl Pts',(-0.453206077218056,-0.573635852336884,
5.37));
#46743=CARTESIAN_POINT('Ctrl Pts',(-0.433697238564491,-0.605525290966034,
5.37));
#46744=CARTESIAN_POINT('Ctrl Pts',(-0.420941367745399,-0.390740191936493,
5.4));
#46745=CARTESIAN_POINT('Ctrl Pts',(-0.420941367745399,-0.390740191936493,
5.37));
#46746=CARTESIAN_POINT('Ctrl Pts',(-0.453206077218056,-0.429195141792297,
5.4));
#46747=CARTESIAN_POINT('Ctrl Pts',(-0.453206077218056,-0.429195141792297,
5.37));
#46748=CARTESIAN_POINT('Ctrl Pts',(-0.453206077218056,-0.501978313922882,
5.4));
#46749=CARTESIAN_POINT('Ctrl Pts',(-0.453206077218056,-0.501978313922882,
5.37));
#46750=CARTESIAN_POINT('Ctrl Pts',(-0.420941367745399,-0.390740191936493,
5.4));
#46751=CARTESIAN_POINT('Ctrl Pts',(-0.453206077218056,-0.429195141792297,
5.4));
#46752=CARTESIAN_POINT('Ctrl Pts',(-0.453206077218056,-0.501978313922882,
5.4));
#46753=CARTESIAN_POINT('Ctrl Pts',(-0.420941367745399,-0.390740191936493,
5.37));
#46754=CARTESIAN_POINT('Ctrl Pts',(-0.453206077218056,-0.429195141792297,
5.37));
#46755=CARTESIAN_POINT('Ctrl Pts',(-0.453206077218056,-0.501978313922882,
5.37));
#46756=CARTESIAN_POINT('Ctrl Pts',(-0.220225110650063,-0.657298839092255,
5.4));
#46757=CARTESIAN_POINT('Ctrl Pts',(-0.220225110650063,-0.657298839092255,
5.37));
#46758=CARTESIAN_POINT('Ctrl Pts',(-0.270873084664345,-0.713199293613434,
5.4));
#46759=CARTESIAN_POINT('Ctrl Pts',(-0.270873084664345,-0.713199293613434,
5.37));
#46760=CARTESIAN_POINT('Ctrl Pts',(-0.341780439019203,-0.713199293613434,
5.4));
#46761=CARTESIAN_POINT('Ctrl Pts',(-0.341780439019203,-0.713199293613434,
5.37));
#46762=CARTESIAN_POINT('',(-0.220225110650063,-0.657298839092255,5.4));
#46763=CARTESIAN_POINT('',(-0.341780439019203,-0.713199293613434,5.4));
#46764=CARTESIAN_POINT('Ctrl Pts',(-0.220225110650063,-0.657298839092255,
5.4));
#46765=CARTESIAN_POINT('Ctrl Pts',(-0.270873084664345,-0.713199293613434,
5.4));
#46766=CARTESIAN_POINT('Ctrl Pts',(-0.341780439019203,-0.713199293613434,
5.4));
#46767=CARTESIAN_POINT('',(-0.220225110650063,-0.657298839092255,5.37));
#46768=CARTESIAN_POINT('',(-0.220225110650063,-0.657298839092255,5.4));
#46769=CARTESIAN_POINT('',(-0.341780439019203,-0.713199293613434,5.37));
#46770=CARTESIAN_POINT('Ctrl Pts',(-0.220225110650063,-0.657298839092255,
5.37));
#46771=CARTESIAN_POINT('Ctrl Pts',(-0.270873084664345,-0.713199293613434,
5.37));
#46772=CARTESIAN_POINT('Ctrl Pts',(-0.341780439019203,-0.713199293613434,
5.37));
#46773=CARTESIAN_POINT('',(-0.341780439019203,-0.713199293613434,5.4));
#46774=CARTESIAN_POINT('Ctrl Pts',(-0.16957713663578,-0.498976862430572,
5.4));
#46775=CARTESIAN_POINT('Ctrl Pts',(-0.16957713663578,-0.498976862430572,
5.37));
#46776=CARTESIAN_POINT('Ctrl Pts',(-0.16957713663578,-0.601398384571075,
5.4));
#46777=CARTESIAN_POINT('Ctrl Pts',(-0.16957713663578,-0.601398384571075,
5.37));
#46778=CARTESIAN_POINT('Ctrl Pts',(-0.220225110650063,-0.657298839092255,
5.4));
#46779=CARTESIAN_POINT('Ctrl Pts',(-0.220225110650063,-0.657298839092255,
5.37));
#46780=CARTESIAN_POINT('',(-0.16957713663578,-0.498976862430572,5.4));
#46781=CARTESIAN_POINT('Ctrl Pts',(-0.16957713663578,-0.498976862430572,
5.4));
#46782=CARTESIAN_POINT('Ctrl Pts',(-0.16957713663578,-0.601398384571075,
5.4));
#46783=CARTESIAN_POINT('Ctrl Pts',(-0.220225110650063,-0.657298839092255,
5.4));
#46784=CARTESIAN_POINT('',(-0.16957713663578,-0.498976862430572,5.37));
#46785=CARTESIAN_POINT('',(-0.16957713663578,-0.498976862430572,5.4));
#46786=CARTESIAN_POINT('Ctrl Pts',(-0.16957713663578,-0.498976862430572,
5.37));
#46787=CARTESIAN_POINT('Ctrl Pts',(-0.16957713663578,-0.601398384571075,
5.37));
#46788=CARTESIAN_POINT('Ctrl Pts',(-0.220225110650063,-0.657298839092255,
5.37));
#46789=CARTESIAN_POINT('Ctrl Pts',(-0.18158246576786,-0.417940056324005,
5.4));
#46790=CARTESIAN_POINT('Ctrl Pts',(-0.18158246576786,-0.417940056324005,
5.37));
#46791=CARTESIAN_POINT('Ctrl Pts',(-0.16957713663578,-0.455832278728485,
5.4));
#46792=CARTESIAN_POINT('Ctrl Pts',(-0.16957713663578,-0.455832278728485,
5.37));
#46793=CARTESIAN_POINT('Ctrl Pts',(-0.16957713663578,-0.498976862430572,
5.4));
#46794=CARTESIAN_POINT('Ctrl Pts',(-0.16957713663578,-0.498976862430572,
5.37));
#46795=CARTESIAN_POINT('',(-0.18158246576786,-0.417940056324005,5.4));
#46796=CARTESIAN_POINT('Ctrl Pts',(-0.18158246576786,-0.417940056324005,
5.4));
#46797=CARTESIAN_POINT('Ctrl Pts',(-0.16957713663578,-0.455832278728485,
5.4));
#46798=CARTESIAN_POINT('Ctrl Pts',(-0.16957713663578,-0.498976862430572,
5.4));
#46799=CARTESIAN_POINT('',(-0.18158246576786,-0.417940056324005,5.37));
#46800=CARTESIAN_POINT('',(-0.18158246576786,-0.417940056324005,5.4));
#46801=CARTESIAN_POINT('Ctrl Pts',(-0.18158246576786,-0.417940056324005,
5.37));
#46802=CARTESIAN_POINT('Ctrl Pts',(-0.16957713663578,-0.455832278728485,
5.37));
#46803=CARTESIAN_POINT('Ctrl Pts',(-0.16957713663578,-0.498976862430572,
5.37));
#46804=CARTESIAN_POINT('Ctrl Pts',(-0.214785113930702,-0.353223121166229,
5.4));
#46805=CARTESIAN_POINT('Ctrl Pts',(-0.214785113930702,-0.353223121166229,
5.37));
#46806=CARTESIAN_POINT('Ctrl Pts',(-0.19358803331852,-0.380047833919525,
5.4));
#46807=CARTESIAN_POINT('Ctrl Pts',(-0.19358803331852,-0.380047833919525,
5.37));
#46808=CARTESIAN_POINT('Ctrl Pts',(-0.18158246576786,-0.417940056324005,
5.4));
#46809=CARTESIAN_POINT('Ctrl Pts',(-0.18158246576786,-0.417940056324005,
5.37));
#46810=CARTESIAN_POINT('',(-0.214785113930702,-0.353223121166229,5.4));
#46811=CARTESIAN_POINT('Ctrl Pts',(-0.214785113930702,-0.353223121166229,
5.4));
#46812=CARTESIAN_POINT('Ctrl Pts',(-0.19358803331852,-0.380047833919525,
5.4));
#46813=CARTESIAN_POINT('Ctrl Pts',(-0.18158246576786,-0.417940056324005,
5.4));
#46814=CARTESIAN_POINT('',(-0.214785113930702,-0.353223121166229,5.37));
#46815=CARTESIAN_POINT('',(-0.214785113930702,-0.353223121166229,5.4));
#46816=CARTESIAN_POINT('Ctrl Pts',(-0.214785113930702,-0.353223121166229,
5.37));
#46817=CARTESIAN_POINT('Ctrl Pts',(-0.19358803331852,-0.380047833919525,
5.37));
#46818=CARTESIAN_POINT('Ctrl Pts',(-0.18158246576786,-0.417940056324005,
5.37));
#46819=CARTESIAN_POINT('Ctrl Pts',(-0.2688098102808,-0.311579144001007,
5.4));
#46820=CARTESIAN_POINT('Ctrl Pts',(-0.2688098102808,-0.311579144001007,
5.37));
#46821=CARTESIAN_POINT('Ctrl Pts',(-0.235982194542885,-0.326398408412933,
5.4));
#46822=CARTESIAN_POINT('Ctrl Pts',(-0.235982194542885,-0.326398408412933,
5.37));
#46823=CARTESIAN_POINT('Ctrl Pts',(-0.214785113930702,-0.353223121166229,
5.4));
#46824=CARTESIAN_POINT('Ctrl Pts',(-0.214785113930702,-0.353223121166229,
5.37));
#46825=CARTESIAN_POINT('',(-0.2688098102808,-0.311579144001007,5.4));
#46826=CARTESIAN_POINT('Ctrl Pts',(-0.2688098102808,-0.311579144001007,
5.4));
#46827=CARTESIAN_POINT('Ctrl Pts',(-0.235982194542885,-0.326398408412933,
5.4));
#46828=CARTESIAN_POINT('Ctrl Pts',(-0.214785113930702,-0.353223121166229,
5.4));
#46829=CARTESIAN_POINT('',(-0.2688098102808,-0.311579144001007,5.37));
#46830=CARTESIAN_POINT('',(-0.2688098102808,-0.311579144001007,5.4));
#46831=CARTESIAN_POINT('Ctrl Pts',(-0.2688098102808,-0.311579144001007,
5.37));
#46832=CARTESIAN_POINT('Ctrl Pts',(-0.235982194542885,-0.326398408412933,
5.37));
#46833=CARTESIAN_POINT('Ctrl Pts',(-0.214785113930702,-0.353223121166229,
5.37));
#46834=CARTESIAN_POINT('Ctrl Pts',(-0.338403716683388,-0.296759939193726,
5.4));
#46835=CARTESIAN_POINT('Ctrl Pts',(-0.338403716683388,-0.296759939193726,
5.37));
#46836=CARTESIAN_POINT('Ctrl Pts',(-0.301637187600136,-0.296759939193726,
5.4));
#46837=CARTESIAN_POINT('Ctrl Pts',(-0.301637187600136,-0.296759939193726,
5.37));
#46838=CARTESIAN_POINT('Ctrl Pts',(-0.2688098102808,-0.311579144001007,
5.4));
#46839=CARTESIAN_POINT('Ctrl Pts',(-0.2688098102808,-0.311579144001007,
5.37));
#46840=CARTESIAN_POINT('',(-0.338403716683388,-0.296759939193726,5.4));
#46841=CARTESIAN_POINT('Ctrl Pts',(-0.338403716683388,-0.296759939193726,
5.4));
#46842=CARTESIAN_POINT('Ctrl Pts',(-0.301637187600136,-0.296759939193726,
5.4));
#46843=CARTESIAN_POINT('Ctrl Pts',(-0.2688098102808,-0.311579144001007,
5.4));
#46844=CARTESIAN_POINT('',(-0.338403716683388,-0.296759939193726,5.37));
#46845=CARTESIAN_POINT('',(-0.338403716683388,-0.296759939193726,5.4));
#46846=CARTESIAN_POINT('Ctrl Pts',(-0.338403716683388,-0.296759939193726,
5.37));
#46847=CARTESIAN_POINT('Ctrl Pts',(-0.301637187600136,-0.296759939193726,
5.37));
#46848=CARTESIAN_POINT('Ctrl Pts',(-0.2688098102808,-0.311579144001007,
5.37));
#46849=CARTESIAN_POINT('Ctrl Pts',(-0.447578445076942,-0.350409305095673,
5.4));
#46850=CARTESIAN_POINT('Ctrl Pts',(-0.447578445076942,-0.350409305095673,
5.37));
#46851=CARTESIAN_POINT('Ctrl Pts',(-0.404809013009071,-0.296759939193726,
5.4));
#46852=CARTESIAN_POINT('Ctrl Pts',(-0.404809013009071,-0.296759939193726,
5.37));
#46853=CARTESIAN_POINT('Ctrl Pts',(-0.338403716683388,-0.296759939193726,
5.4));
#46854=CARTESIAN_POINT('Ctrl Pts',(-0.338403716683388,-0.296759939193726,
5.37));
#46855=CARTESIAN_POINT('',(-0.447578445076942,-0.350409305095673,5.4));
#46856=CARTESIAN_POINT('Ctrl Pts',(-0.447578445076942,-0.350409305095673,
5.4));
#46857=CARTESIAN_POINT('Ctrl Pts',(-0.404809013009071,-0.296759939193726,
5.4));
#46858=CARTESIAN_POINT('Ctrl Pts',(-0.338403716683388,-0.296759939193726,
5.4));
#46859=CARTESIAN_POINT('',(-0.447578445076942,-0.350409305095673,5.37));
#46860=CARTESIAN_POINT('',(-0.447578445076942,-0.350409305095673,5.4));
#46861=CARTESIAN_POINT('Ctrl Pts',(-0.447578445076942,-0.350409305095673,
5.37));
#46862=CARTESIAN_POINT('Ctrl Pts',(-0.404809013009071,-0.296759939193726,
5.37));
#46863=CARTESIAN_POINT('Ctrl Pts',(-0.338403716683388,-0.296759939193726,
5.37));
#46864=CARTESIAN_POINT('Origin',(-0.447578445076942,-0.154195165634155,
5.4));
#46865=CARTESIAN_POINT('',(-0.447578445076942,-0.154195165634155,5.4));
#46866=CARTESIAN_POINT('',(-0.447578445076942,-0.0770975828170776,5.4));
#46867=CARTESIAN_POINT('',(-0.447578445076942,-0.154195165634155,5.37));
#46868=CARTESIAN_POINT('',(-0.447578445076942,-0.154195165634155,5.4));
#46869=CARTESIAN_POINT('',(-0.447578445076942,-0.154195165634155,5.37));
#46870=CARTESIAN_POINT('Origin',(-0.515109077095985,-0.154195165634155,
5.4));
#46871=CARTESIAN_POINT('',(-0.515109077095985,-0.154195165634155,5.4));
#46872=CARTESIAN_POINT('',(-0.257554538547993,-0.154195165634155,5.4));
#46873=CARTESIAN_POINT('',(-0.515109077095985,-0.154195165634155,5.37));
#46874=CARTESIAN_POINT('',(-0.515109077095985,-0.154195165634155,5.4));
#46875=CARTESIAN_POINT('',(-0.515109077095985,-0.154195165634155,5.37));
#46876=CARTESIAN_POINT('Origin',(-0.515109077095985,-0.704195177555084,
5.4));
#46877=CARTESIAN_POINT('',(-0.515109077095985,-0.704195177555084,5.4));
#46878=CARTESIAN_POINT('',(-0.515109077095985,-0.352097588777542,5.4));
#46879=CARTESIAN_POINT('',(-0.515109077095985,-0.704195177555084,5.37));
#46880=CARTESIAN_POINT('',(-0.515109077095985,-0.704195177555084,5.4));
#46881=CARTESIAN_POINT('',(-0.515109077095985,-0.704195177555084,5.37));
#46882=CARTESIAN_POINT('Origin',(-0.452455773949623,-0.704195177555084,
5.4));
#46883=CARTESIAN_POINT('',(-0.452455773949623,-0.704195177555084,5.4));
#46884=CARTESIAN_POINT('',(-0.226227886974812,-0.704195177555084,5.4));
#46885=CARTESIAN_POINT('',(-0.452455773949623,-0.704195177555084,5.37));
#46886=CARTESIAN_POINT('',(-0.452455773949623,-0.704195177555084,5.4));
#46887=CARTESIAN_POINT('',(-0.452455773949623,-0.704195177555084,5.37));
#46888=CARTESIAN_POINT('Origin',(-0.452455773949623,-0.654297506809235,
5.4));
#46889=CARTESIAN_POINT('',(-0.452455773949623,-0.654297506809235,5.4));
#46890=CARTESIAN_POINT('',(-0.452455773949623,-0.327148753404617,5.4));
#46891=CARTESIAN_POINT('',(-0.452455773949623,-0.654297506809235,5.37));
#46892=CARTESIAN_POINT('',(-0.452455773949623,-0.654297506809235,5.4));
#46893=CARTESIAN_POINT('',(-0.452455773949623,-0.654297506809235,5.37));
#46894=CARTESIAN_POINT('Ctrl Pts',(-0.341780439019203,-0.713199293613434,
5.4));
#46895=CARTESIAN_POINT('Ctrl Pts',(-0.341780439019203,-0.713199293613434,
5.37));
#46896=CARTESIAN_POINT('Ctrl Pts',(-0.412312522530556,-0.713199293613434,
5.4));
#46897=CARTESIAN_POINT('Ctrl Pts',(-0.412312522530556,-0.713199293613434,
5.37));
#46898=CARTESIAN_POINT('Ctrl Pts',(-0.452455773949623,-0.654297506809235,
5.4));
#46899=CARTESIAN_POINT('Ctrl Pts',(-0.452455773949623,-0.654297506809235,
5.37));
#46900=CARTESIAN_POINT('Ctrl Pts',(-0.341780439019203,-0.713199293613434,
5.4));
#46901=CARTESIAN_POINT('Ctrl Pts',(-0.412312522530556,-0.713199293613434,
5.4));
#46902=CARTESIAN_POINT('Ctrl Pts',(-0.452455773949623,-0.654297506809235,
5.4));
#46903=CARTESIAN_POINT('Ctrl Pts',(-0.341780439019203,-0.713199293613434,
5.37));
#46904=CARTESIAN_POINT('Ctrl Pts',(-0.412312522530556,-0.713199293613434,
5.37));
#46905=CARTESIAN_POINT('Ctrl Pts',(-0.452455773949623,-0.654297506809235,
5.37));
#46906=CARTESIAN_POINT('Origin',(-0.342343106865883,-0.433697229623795,
5.37));
#46907=CARTESIAN_POINT('Ctrl Pts',(0.417940124869347,-0.416814541816711,
5.4));
#46908=CARTESIAN_POINT('Ctrl Pts',(0.417940124869347,-0.416814541816711,
5.37));
#46909=CARTESIAN_POINT('Ctrl Pts',(0.40668486058712,-0.452830946445465,
5.4));
#46910=CARTESIAN_POINT('Ctrl Pts',(0.40668486058712,-0.452830946445465,
5.37));
#46911=CARTESIAN_POINT('Ctrl Pts',(0.40668486058712,-0.495600378513336,
5.4));
#46912=CARTESIAN_POINT('Ctrl Pts',(0.40668486058712,-0.495600378513336,
5.37));
#46913=CARTESIAN_POINT('',(0.417940124869347,-0.416814541816711,5.4));
#46914=CARTESIAN_POINT('',(0.40668486058712,-0.495600378513336,5.4));
#46915=CARTESIAN_POINT('Ctrl Pts',(0.417940124869347,-0.416814541816711,
5.4));
#46916=CARTESIAN_POINT('Ctrl Pts',(0.40668486058712,-0.452830946445465,
5.4));
#46917=CARTESIAN_POINT('Ctrl Pts',(0.40668486058712,-0.495600378513336,
5.4));
#46918=CARTESIAN_POINT('',(0.417940124869347,-0.416814541816711,5.37));
#46919=CARTESIAN_POINT('',(0.417940124869347,-0.416814541816711,5.4));
#46920=CARTESIAN_POINT('',(0.40668486058712,-0.495600378513336,5.37));
#46921=CARTESIAN_POINT('Ctrl Pts',(0.417940124869347,-0.416814541816711,
5.37));
#46922=CARTESIAN_POINT('Ctrl Pts',(0.40668486058712,-0.452830946445465,
5.37));
#46923=CARTESIAN_POINT('Ctrl Pts',(0.40668486058712,-0.495600378513336,
5.37));
#46924=CARTESIAN_POINT('',(0.40668486058712,-0.495600378513336,5.4));
#46925=CARTESIAN_POINT('Ctrl Pts',(0.443076357245445,-0.379860198497772,
5.4));
#46926=CARTESIAN_POINT('Ctrl Pts',(0.443076357245445,-0.379860198497772,
5.37));
#46927=CARTESIAN_POINT('Ctrl Pts',(0.425443395972252,-0.393178796768188,
5.4));
#46928=CARTESIAN_POINT('Ctrl Pts',(0.425443395972252,-0.393178796768188,
5.37));
#46929=CARTESIAN_POINT('Ctrl Pts',(0.417940124869347,-0.416814541816711,
5.4));
#46930=CARTESIAN_POINT('Ctrl Pts',(0.417940124869347,-0.416814541816711,
5.37));
#46931=CARTESIAN_POINT('',(0.443076357245445,-0.379860198497772,5.4));
#46932=CARTESIAN_POINT('Ctrl Pts',(0.443076357245445,-0.379860198497772,
5.4));
#46933=CARTESIAN_POINT('Ctrl Pts',(0.425443395972252,-0.393178796768188,
5.4));
#46934=CARTESIAN_POINT('Ctrl Pts',(0.417940124869347,-0.416814541816711,
5.4));
#46935=CARTESIAN_POINT('',(0.443076357245445,-0.379860198497772,5.37));
#46936=CARTESIAN_POINT('',(0.443076357245445,-0.379860198497772,5.4));
#46937=CARTESIAN_POINT('Ctrl Pts',(0.443076357245445,-0.379860198497772,
5.37));
#46938=CARTESIAN_POINT('Ctrl Pts',(0.425443395972252,-0.393178796768188,
5.37));
#46939=CARTESIAN_POINT('Ctrl Pts',(0.417940124869347,-0.416814541816711,
5.37));
#46940=CARTESIAN_POINT('Ctrl Pts',(0.482844337821007,-0.366541659832001,
5.4));
#46941=CARTESIAN_POINT('Ctrl Pts',(0.482844337821007,-0.366541659832001,
5.37));
#46942=CARTESIAN_POINT('Ctrl Pts',(0.460709556937218,-0.366541659832001,
5.4));
#46943=CARTESIAN_POINT('Ctrl Pts',(0.460709556937218,-0.366541659832001,
5.37));
#46944=CARTESIAN_POINT('Ctrl Pts',(0.443076357245445,-0.379860198497772,
5.4));
#46945=CARTESIAN_POINT('Ctrl Pts',(0.443076357245445,-0.379860198497772,
5.37));
#46946=CARTESIAN_POINT('',(0.482844337821007,-0.366541659832001,5.4));
#46947=CARTESIAN_POINT('Ctrl Pts',(0.482844337821007,-0.366541659832001,
5.4));
#46948=CARTESIAN_POINT('Ctrl Pts',(0.460709556937218,-0.366541659832001,
5.4));
#46949=CARTESIAN_POINT('Ctrl Pts',(0.443076357245445,-0.379860198497772,
5.4));
#46950=CARTESIAN_POINT('',(0.482844337821007,-0.366541659832001,5.37));
#46951=CARTESIAN_POINT('',(0.482844337821007,-0.366541659832001,5.4));
#46952=CARTESIAN_POINT('Ctrl Pts',(0.482844337821007,-0.366541659832001,
5.37));
#46953=CARTESIAN_POINT('Ctrl Pts',(0.460709556937218,-0.366541659832001,
5.37));
#46954=CARTESIAN_POINT('Ctrl Pts',(0.443076357245445,-0.379860198497772,
5.37));
#46955=CARTESIAN_POINT('Ctrl Pts',(0.53236697614193,-0.381173288822174,
5.4));
#46956=CARTESIAN_POINT('Ctrl Pts',(0.53236697614193,-0.381173288822174,
5.37));
#46957=CARTESIAN_POINT('Ctrl Pts',(0.507605776190758,-0.366541659832001,
5.4));
#46958=CARTESIAN_POINT('Ctrl Pts',(0.507605776190758,-0.366541659832001,
5.37));
#46959=CARTESIAN_POINT('Ctrl Pts',(0.482844337821007,-0.366541659832001,
5.4));
#46960=CARTESIAN_POINT('Ctrl Pts',(0.482844337821007,-0.366541659832001,
5.37));
#46961=CARTESIAN_POINT('',(0.53236697614193,-0.381173288822174,5.4));
#46962=CARTESIAN_POINT('Ctrl Pts',(0.53236697614193,-0.381173288822174,
5.4));
#46963=CARTESIAN_POINT('Ctrl Pts',(0.507605776190758,-0.366541659832001,
5.4));
#46964=CARTESIAN_POINT('Ctrl Pts',(0.482844337821007,-0.366541659832001,
5.4));
#46965=CARTESIAN_POINT('',(0.53236697614193,-0.381173288822174,5.37));
#46966=CARTESIAN_POINT('',(0.53236697614193,-0.381173288822174,5.4));
#46967=CARTESIAN_POINT('Ctrl Pts',(0.53236697614193,-0.381173288822174,
5.37));
#46968=CARTESIAN_POINT('Ctrl Pts',(0.507605776190758,-0.366541659832001,
5.37));
#46969=CARTESIAN_POINT('Ctrl Pts',(0.482844337821007,-0.366541659832001,
5.37));
#46970=CARTESIAN_POINT('Origin',(0.555627569556236,-0.318519866466522,5.4));
#46971=CARTESIAN_POINT('',(0.555627569556236,-0.318519866466522,5.4));
#46972=CARTESIAN_POINT('',(0.573938477534482,-0.269198637603509,5.4));
#46973=CARTESIAN_POINT('',(0.555627569556236,-0.318519866466522,5.37));
#46974=CARTESIAN_POINT('',(0.555627569556236,-0.318519866466522,5.4));
#46975=CARTESIAN_POINT('',(0.555627569556236,-0.318519866466522,5.37));
#46976=CARTESIAN_POINT('Ctrl Pts',(0.486221060156822,-0.29675999879837,
5.4));
#46977=CARTESIAN_POINT('Ctrl Pts',(0.486221060156822,-0.29675999879837,
5.37));
#46978=CARTESIAN_POINT('Ctrl Pts',(0.52036140859127,-0.29675999879837,5.4));
#46979=CARTESIAN_POINT('Ctrl Pts',(0.52036140859127,-0.29675999879837,5.37));
#46980=CARTESIAN_POINT('Ctrl Pts',(0.555627569556236,-0.318519866466522,
5.4));
#46981=CARTESIAN_POINT('Ctrl Pts',(0.555627569556236,-0.318519866466522,
5.37));
#46982=CARTESIAN_POINT('',(0.486221060156822,-0.29675999879837,5.4));
#46983=CARTESIAN_POINT('Ctrl Pts',(0.486221060156822,-0.29675999879837,
5.4));
#46984=CARTESIAN_POINT('Ctrl Pts',(0.52036140859127,-0.29675999879837,5.4));
#46985=CARTESIAN_POINT('Ctrl Pts',(0.555627569556236,-0.318519866466522,
5.4));
#46986=CARTESIAN_POINT('',(0.486221060156822,-0.29675999879837,5.37));
#46987=CARTESIAN_POINT('',(0.486221060156822,-0.29675999879837,5.4));
#46988=CARTESIAN_POINT('Ctrl Pts',(0.486221060156822,-0.29675999879837,
5.37));
#46989=CARTESIAN_POINT('Ctrl Pts',(0.52036140859127,-0.29675999879837,5.37));
#46990=CARTESIAN_POINT('Ctrl Pts',(0.555627569556236,-0.318519866466522,
5.37));
#46991=CARTESIAN_POINT('Ctrl Pts',(0.442888721823692,-0.310266053676605,
5.4));
#46992=CARTESIAN_POINT('Ctrl Pts',(0.442888721823692,-0.310266053676605,
5.37));
#46993=CARTESIAN_POINT('Ctrl Pts',(0.462585434317589,-0.29675999879837,
5.4));
#46994=CARTESIAN_POINT('Ctrl Pts',(0.462585434317589,-0.29675999879837,
5.37));
#46995=CARTESIAN_POINT('Ctrl Pts',(0.486221060156822,-0.29675999879837,
5.4));
#46996=CARTESIAN_POINT('Ctrl Pts',(0.486221060156822,-0.29675999879837,
5.37));
#46997=CARTESIAN_POINT('',(0.442888721823692,-0.310266053676605,5.4));
#46998=CARTESIAN_POINT('Ctrl Pts',(0.442888721823692,-0.310266053676605,
5.4));
#46999=CARTESIAN_POINT('Ctrl Pts',(0.462585434317589,-0.29675999879837,
5.4));
#47000=CARTESIAN_POINT('Ctrl Pts',(0.486221060156822,-0.29675999879837,
5.4));
#47001=CARTESIAN_POINT('',(0.442888721823692,-0.310266053676605,5.37));
#47002=CARTESIAN_POINT('',(0.442888721823692,-0.310266053676605,5.4));
#47003=CARTESIAN_POINT('Ctrl Pts',(0.442888721823692,-0.310266053676605,
5.37));
#47004=CARTESIAN_POINT('Ctrl Pts',(0.462585434317589,-0.29675999879837,
5.37));
#47005=CARTESIAN_POINT('Ctrl Pts',(0.486221060156822,-0.29675999879837,
5.37));
#47006=CARTESIAN_POINT('Ctrl Pts',(0.399931892752647,-0.366166508197784,
5.4));
#47007=CARTESIAN_POINT('Ctrl Pts',(0.399931892752647,-0.366166508197784,
5.37));
#47008=CARTESIAN_POINT('Ctrl Pts',(0.423192486166954,-0.32377222776413,
5.4));
#47009=CARTESIAN_POINT('Ctrl Pts',(0.423192486166954,-0.32377222776413,
5.37));
#47010=CARTESIAN_POINT('Ctrl Pts',(0.442888721823692,-0.310266053676605,
5.4));
#47011=CARTESIAN_POINT('Ctrl Pts',(0.442888721823692,-0.310266053676605,
5.37));
#47012=CARTESIAN_POINT('',(0.399931892752647,-0.366166508197784,5.4));
#47013=CARTESIAN_POINT('Ctrl Pts',(0.399931892752647,-0.366166508197784,
5.4));
#47014=CARTESIAN_POINT('Ctrl Pts',(0.423192486166954,-0.32377222776413,
5.4));
#47015=CARTESIAN_POINT('Ctrl Pts',(0.442888721823692,-0.310266053676605,
5.4));
#47016=CARTESIAN_POINT('',(0.399931892752647,-0.366166508197784,5.37));
#47017=CARTESIAN_POINT('',(0.399931892752647,-0.366166508197784,5.4));
#47018=CARTESIAN_POINT('Ctrl Pts',(0.399931892752647,-0.366166508197784,
5.37));
#47019=CARTESIAN_POINT('Ctrl Pts',(0.423192486166954,-0.32377222776413,
5.37));
#47020=CARTESIAN_POINT('Ctrl Pts',(0.442888721823692,-0.310266053676605,
5.37));
#47021=CARTESIAN_POINT('Origin',(0.399931892752647,-0.305764055252075,5.4));
#47022=CARTESIAN_POINT('',(0.399931892752647,-0.305764055252075,5.4));
#47023=CARTESIAN_POINT('',(0.399931892752647,-0.152882027626038,5.4));
#47024=CARTESIAN_POINT('',(0.399931892752647,-0.305764055252075,5.37));
#47025=CARTESIAN_POINT('',(0.399931892752647,-0.305764055252075,5.4));
#47026=CARTESIAN_POINT('',(0.399931892752647,-0.305764055252075,5.37));
#47027=CARTESIAN_POINT('Origin',(0.339154228568077,-0.305764055252075,5.4));
#47028=CARTESIAN_POINT('',(0.339154228568077,-0.305764055252075,5.4));
#47029=CARTESIAN_POINT('',(0.169577114284039,-0.305764055252075,5.4));
#47030=CARTESIAN_POINT('',(0.339154228568077,-0.305764055252075,5.37));
#47031=CARTESIAN_POINT('',(0.339154228568077,-0.305764055252075,5.4));
#47032=CARTESIAN_POINT('',(0.339154228568077,-0.305764055252075,5.37));
#47033=CARTESIAN_POINT('Origin',(0.339154228568077,-0.704195177555084,5.4));
#47034=CARTESIAN_POINT('',(0.339154228568077,-0.704195177555084,5.4));
#47035=CARTESIAN_POINT('',(0.339154228568077,-0.352097588777542,5.4));
#47036=CARTESIAN_POINT('',(0.339154228568077,-0.704195177555084,5.37));
#47037=CARTESIAN_POINT('',(0.339154228568077,-0.704195177555084,5.4));
#47038=CARTESIAN_POINT('',(0.339154228568077,-0.704195177555084,5.37));
#47039=CARTESIAN_POINT('Origin',(0.40668486058712,-0.704195177555084,5.4));
#47040=CARTESIAN_POINT('',(0.40668486058712,-0.704195177555084,5.4));
#47041=CARTESIAN_POINT('',(0.20334243029356,-0.704195177555084,5.4));
#47042=CARTESIAN_POINT('',(0.40668486058712,-0.704195177555084,5.37));
#47043=CARTESIAN_POINT('',(0.40668486058712,-0.704195177555084,5.4));
#47044=CARTESIAN_POINT('',(0.40668486058712,-0.704195177555084,5.37));
#47045=CARTESIAN_POINT('Origin',(0.40668486058712,-0.495600378513336,5.4));
#47046=CARTESIAN_POINT('',(0.40668486058712,-0.247800189256668,5.4));
#47047=CARTESIAN_POINT('',(0.40668486058712,-0.495600378513336,5.37));
#47048=CARTESIAN_POINT('Origin',(0.447390899062157,-0.500477588176727,5.37));
#47049=CARTESIAN_POINT('Origin',(0.,0.,5.4));
#47050=CARTESIAN_POINT('Origin',(0.,0.,5.4));
#47051=CARTESIAN_POINT('Origin',(0.,0.,5.4));
#47052=CARTESIAN_POINT('Origin',(0.,0.,5.4));
#47053=CARTESIAN_POINT('Origin',(0.,0.,5.4));
#47054=CARTESIAN_POINT('Origin',(0.,0.,5.4));
#47055=CARTESIAN_POINT('Origin',(0.,4.8,3.135));
#47056=CARTESIAN_POINT('',(-0.3,4.8,2.4));
#47057=CARTESIAN_POINT('Origin',(0.,4.8,2.4));
#47058=CARTESIAN_POINT('',(-0.3,4.8,3.5));
#47059=CARTESIAN_POINT('',(-0.3,4.8,3.135));
#47060=CARTESIAN_POINT('',(-1.32689352189158E-17,4.5,3.4));
#47061=CARTESIAN_POINT('Ctrl Pts',(3.46944695195361E-17,4.5,3.4));
#47062=CARTESIAN_POINT('Ctrl Pts',(-0.0387350904599242,4.5,3.4));
#47063=CARTESIAN_POINT('Ctrl Pts',(-0.079391136615057,4.50794962800524,
3.40489262537173));
#47064=CARTESIAN_POINT('Ctrl Pts',(-0.153059740759081,4.53890790426334,
3.42249923688317));
#47065=CARTESIAN_POINT('Ctrl Pts',(-0.186131887156364,4.56186781844444,
3.43504912069967));
#47066=CARTESIAN_POINT('Ctrl Pts',(-0.238301026739628,4.6140369580277,3.4594914730493));
#47067=CARTESIAN_POINT('Ctrl Pts',(-0.261143371678758,4.64706258429155,
3.47321311494003));
#47068=CARTESIAN_POINT('Ctrl Pts',(-0.291998110979302,4.7204841942567,3.49369955460524));
#47069=CARTESIAN_POINT('Ctrl Pts',(-0.3,4.76101336352273,3.5));
#47070=CARTESIAN_POINT('Ctrl Pts',(-0.3,4.8,3.5));
#47071=CARTESIAN_POINT('',(0.3,4.8,3.5));
#47072=CARTESIAN_POINT('Ctrl Pts',(0.3,4.8,3.5));
#47073=CARTESIAN_POINT('Ctrl Pts',(0.3,4.76101336352273,3.5));
#47074=CARTESIAN_POINT('Ctrl Pts',(0.291998110979302,4.7204841942567,3.49369955460524));
#47075=CARTESIAN_POINT('Ctrl Pts',(0.261143371678758,4.64706258429155,3.47321311494003));
#47076=CARTESIAN_POINT('Ctrl Pts',(0.238301026739628,4.6140369580277,3.4594914730493));
#47077=CARTESIAN_POINT('Ctrl Pts',(0.186131887156364,4.56186781844444,3.43504912069967));
#47078=CARTESIAN_POINT('Ctrl Pts',(0.153059740759081,4.53890790426334,3.42249923688317));
#47079=CARTESIAN_POINT('Ctrl Pts',(0.0793911366150571,4.50794962800524,
3.40489262537173));
#47080=CARTESIAN_POINT('Ctrl Pts',(0.0387350904599242,4.5,3.4));
#47081=CARTESIAN_POINT('Ctrl Pts',(-6.24500451351651E-17,4.5,3.4));
#47082=CARTESIAN_POINT('',(-3.75550638825911E-17,5.1,3.4));
#47083=CARTESIAN_POINT('Ctrl Pts',(-4.16333634234434E-17,5.1,3.4));
#47084=CARTESIAN_POINT('Ctrl Pts',(0.0387350904599243,5.1,3.4));
#47085=CARTESIAN_POINT('Ctrl Pts',(0.079391136615057,5.09205037199476,3.40489262537173));
#47086=CARTESIAN_POINT('Ctrl Pts',(0.15305974075908,5.06109209573666,3.42249923688317));
#47087=CARTESIAN_POINT('Ctrl Pts',(0.186131887156364,5.03813218155556,3.43504912069967));
#47088=CARTESIAN_POINT('Ctrl Pts',(0.238301026739628,4.9859630419723,3.4594914730493));
#47089=CARTESIAN_POINT('Ctrl Pts',(0.261143371678758,4.95293741570845,3.47321311494003));
#47090=CARTESIAN_POINT('Ctrl Pts',(0.291998110979302,4.8795158057433,3.49369955460524));
#47091=CARTESIAN_POINT('Ctrl Pts',(0.3,4.83898663647727,3.5));
#47092=CARTESIAN_POINT('Ctrl Pts',(0.3,4.8,3.5));
#47093=CARTESIAN_POINT('Ctrl Pts',(-0.3,4.8,3.5));
#47094=CARTESIAN_POINT('Ctrl Pts',(-0.3,4.83898663647727,3.5));
#47095=CARTESIAN_POINT('Ctrl Pts',(-0.291998110979302,4.8795158057433,3.49369955460524));
#47096=CARTESIAN_POINT('Ctrl Pts',(-0.261143371678758,4.95293741570845,
3.47321311494003));
#47097=CARTESIAN_POINT('Ctrl Pts',(-0.238301026739628,4.9859630419723,3.4594914730493));
#47098=CARTESIAN_POINT('Ctrl Pts',(-0.186131887156364,5.03813218155556,
3.43504912069967));
#47099=CARTESIAN_POINT('Ctrl Pts',(-0.153059740759081,5.06109209573666,
3.42249923688317));
#47100=CARTESIAN_POINT('Ctrl Pts',(-0.0793911366150575,5.09205037199476,
3.40489262537173));
#47101=CARTESIAN_POINT('Ctrl Pts',(-0.0387350904599243,5.1,3.4));
#47102=CARTESIAN_POINT('Ctrl Pts',(-1.38777878078145E-17,5.1,3.4));
#47103=CARTESIAN_POINT('Origin',(0.,6.76,3.9));
#47104=CARTESIAN_POINT('',(-1.12434822629719E-16,6.8,2.9819));
#47105=CARTESIAN_POINT('Origin',(0.,6.8,3.9));
#47106=CARTESIAN_POINT('',(1.0263764823654E-16,6.72,3.0619));
#47107=CARTESIAN_POINT('',(-1.07536235433129E-16,6.76,3.0219));
#47108=CARTESIAN_POINT('Origin',(0.,6.72,3.9));
#47109=CARTESIAN_POINT('Origin',(0.,6.115,3.9));
#47110=CARTESIAN_POINT('',(-1.0263764823654E-16,5.4,3.0619));
#47111=CARTESIAN_POINT('Origin',(0.,5.4,3.9));
#47112=CARTESIAN_POINT('',(-1.0263764823654E-16,6.115,3.0619));
#47113=CARTESIAN_POINT('Origin',(0.,6.8,3.9));
#47114=CARTESIAN_POINT('',(-1.66132477258362,6.8,4.7));
#47115=CARTESIAN_POINT('',(-1.66132477258362,6.8,2.6));
#47116=CARTESIAN_POINT('',(-1.66132477258362,6.8,3.925));
#47117=CARTESIAN_POINT('',(1.66132477258362,6.8,4.7));
#47118=CARTESIAN_POINT('Ctrl Pts',(1.66132477258362,6.8,4.7));
#47119=CARTESIAN_POINT('Ctrl Pts',(1.66132477258362,6.8,4.72938558803469));
#47120=CARTESIAN_POINT('Ctrl Pts',(1.65134477996489,6.8,4.76320656017475));
#47121=CARTESIAN_POINT('Ctrl Pts',(1.61541194091876,6.8,4.82883847656767));
#47122=CARTESIAN_POINT('Ctrl Pts',(1.57674832389957,6.8,4.86728708168208));
#47123=CARTESIAN_POINT('Ctrl Pts',(1.47030882164508,6.8,4.94844516253902));
#47124=CARTESIAN_POINT('Ctrl Pts',(1.37375034243015,6.8,4.99240423873322));
#47125=CARTESIAN_POINT('Ctrl Pts',(1.19382805886623,6.8,5.05708112048866));
#47126=CARTESIAN_POINT('Ctrl Pts',(1.09032757512215,6.8,5.08373727101866));
#47127=CARTESIAN_POINT('Ctrl Pts',(0.876179229724424,6.8,5.12689010427577));
#47128=CARTESIAN_POINT('Ctrl Pts',(0.765498572136393,6.8,5.14322387535846));
#47129=CARTESIAN_POINT('Ctrl Pts',(0.431232289541573,6.8,5.18054651477358));
#47130=CARTESIAN_POINT('Ctrl Pts',(0.20556454289784,6.8,5.18989794855664));
#47131=CARTESIAN_POINT('Ctrl Pts',(-0.20556454289784,6.8,5.18989794855664));
#47132=CARTESIAN_POINT('Ctrl Pts',(-0.431232289541573,6.8,5.18054651477358));
#47133=CARTESIAN_POINT('Ctrl Pts',(-0.765498572136393,6.8,5.14322387535846));
#47134=CARTESIAN_POINT('Ctrl Pts',(-0.876179229724424,6.8,5.12689010427577));
#47135=CARTESIAN_POINT('Ctrl Pts',(-1.09032757512215,6.8,5.08373727101866));
#47136=CARTESIAN_POINT('Ctrl Pts',(-1.19382805886623,6.8,5.05708112048866));
#47137=CARTESIAN_POINT('Ctrl Pts',(-1.37375034243015,6.8,4.99240423873322));
#47138=CARTESIAN_POINT('Ctrl Pts',(-1.47030882164508,6.8,4.94844516253902));
#47139=CARTESIAN_POINT('Ctrl Pts',(-1.57674832389957,6.8,4.86728708168208));
#47140=CARTESIAN_POINT('Ctrl Pts',(-1.61541194091876,6.8,4.82883847656767));
#47141=CARTESIAN_POINT('Ctrl Pts',(-1.65134477996489,6.8,4.76320656017475));
#47142=CARTESIAN_POINT('Ctrl Pts',(-1.66132477258362,6.8,4.7293855880347));
#47143=CARTESIAN_POINT('Ctrl Pts',(-1.66132477258362,6.8,4.7));
#47144=CARTESIAN_POINT('',(1.66132477258362,6.8,2.6));
#47145=CARTESIAN_POINT('',(1.66132477258362,6.8,3.925));
#47146=CARTESIAN_POINT('',(-1.7,6.8,2.6));
#47147=CARTESIAN_POINT('Origin',(0.,4.24978484524311,3.9));
#47148=CARTESIAN_POINT('',(0.,4.09956969048622,3.9));
#47149=CARTESIAN_POINT('',(-6.12323399573677E-17,4.4,3.4));
#47150=CARTESIAN_POINT('',(-3.06161699786839E-17,4.24978484524311,3.65));
#47151=CARTESIAN_POINT('Origin',(0.,4.4,3.9));
#47152=CARTESIAN_POINT('Origin',(0.,4.9,3.9));
#47153=CARTESIAN_POINT('',(-6.12323399573677E-17,4.9,3.4));
#47154=CARTESIAN_POINT('',(-6.12323399573677E-17,5.4,3.4));
#47155=CARTESIAN_POINT('',(-6.12323399573677E-17,4.9,3.4));
#47156=CARTESIAN_POINT('Origin',(0.,5.4,3.9));
#47157=CARTESIAN_POINT('Origin',(0.,5.4,4.7381));
#47158=CARTESIAN_POINT('Origin',(1.7,6.8,2.6));
#47159=CARTESIAN_POINT('Origin',(0.,0.,2.6));
#47160=CARTESIAN_POINT('Origin',(0.,0.,3.925));
#47161=CARTESIAN_POINT('',(-7.,-8.57252759403147E-16,4.7));
#47162=CARTESIAN_POINT('Origin',(0.,0.,4.7));
#47163=CARTESIAN_POINT('',(-7.,-8.57252759403147E-16,2.45));
#47164=CARTESIAN_POINT('',(-7.,-8.57252759403147E-16,3.925));
#47165=CARTESIAN_POINT('Origin',(0.,0.,2.45));
#47166=CARTESIAN_POINT('Origin',(0.,0.,4.7));
#47167=CARTESIAN_POINT('Origin',(0.,0.,4.7));
#47168=CARTESIAN_POINT('',(-6.3,-7.71527483462833E-16,5.4));
#47169=CARTESIAN_POINT('Origin',(0.,0.,5.4));
#47170=CARTESIAN_POINT('Origin',(-6.3,-7.71527483462833E-16,4.7));
#47171=CARTESIAN_POINT('Origin',(6.,0.,2.425));
#47172=CARTESIAN_POINT('',(5.545,5.57214293612045E-17,2.4));
#47173=CARTESIAN_POINT('Origin',(6.,0.,2.4));
#47174=CARTESIAN_POINT('',(5.595,-4.95981953654677E-17,2.45));
#47175=CARTESIAN_POINT('',(5.57,5.26598123633361E-17,2.425));
#47176=CARTESIAN_POINT('Origin',(6.,0.,2.45));
#47177=CARTESIAN_POINT('Origin',(6.95,0.,2.4));
#47178=CARTESIAN_POINT('',(-6.95,-8.5112952540741E-16,2.4));
#47179=CARTESIAN_POINT('Origin',(0.,0.,2.4));
#47180=CARTESIAN_POINT('',(-3.455,5.19615242270663,2.4));
#47181=CARTESIAN_POINT('Origin',(-3.,5.19615242270663,2.4));
#47182=CARTESIAN_POINT('',(-3.455,-5.19615242270663,2.4));
#47183=CARTESIAN_POINT('Origin',(-3.,-5.19615242270663,2.4));
#47184=CARTESIAN_POINT('',(2.66,-3.25756048573196E-16,2.4));
#47185=CARTESIAN_POINT('Origin',(0.,0.,2.4));
#47186=CARTESIAN_POINT('',(2.545,-5.19615242270663,2.4));
#47187=CARTESIAN_POINT('Origin',(3.,-5.19615242270663,2.4));
#47188=CARTESIAN_POINT('',(-6.455,7.90509508849616E-16,2.4));
#47189=CARTESIAN_POINT('Origin',(-6.,7.34788079488412E-16,2.4));
#47190=CARTESIAN_POINT('',(2.545,5.19615242270663,2.4));
#47191=CARTESIAN_POINT('Origin',(3.,5.19615242270663,2.4));
#47192=CARTESIAN_POINT('Origin',(6.,0.,3.385));
#47193=CARTESIAN_POINT('',(5.595,-4.95981953654677E-17,4.4));
#47194=CARTESIAN_POINT('',(5.595,-4.95981953654677E-17,3.385));
#47195=CARTESIAN_POINT('Origin',(6.,0.,4.4));
#47196=CARTESIAN_POINT('Origin',(3.,5.19615242270663,2.425));
#47197=CARTESIAN_POINT('',(2.595,5.19615242270663,2.45));
#47198=CARTESIAN_POINT('',(2.57,5.19615242270663,2.425));
#47199=CARTESIAN_POINT('Origin',(3.,5.19615242270663,2.45));
#47200=CARTESIAN_POINT('Origin',(3.,5.19615242270663,3.385));
#47201=CARTESIAN_POINT('',(2.595,5.19615242270663,4.4));
#47202=CARTESIAN_POINT('',(2.595,5.19615242270663,3.385));
#47203=CARTESIAN_POINT('Origin',(3.,5.19615242270663,4.4));
#47204=CARTESIAN_POINT('Origin',(-3.,5.19615242270663,2.425));
#47205=CARTESIAN_POINT('',(-3.405,5.19615242270663,2.45));
#47206=CARTESIAN_POINT('',(-3.43,5.19615242270663,2.425));
#47207=CARTESIAN_POINT('Origin',(-3.,5.19615242270663,2.45));
#47208=CARTESIAN_POINT('Origin',(-3.,5.19615242270663,3.385));
#47209=CARTESIAN_POINT('',(-3.405,5.19615242270663,4.4));
#47210=CARTESIAN_POINT('',(-3.405,5.19615242270663,3.385));
#47211=CARTESIAN_POINT('Origin',(-3.,5.19615242270663,4.4));
#47212=CARTESIAN_POINT('Origin',(-6.,7.34788079488412E-16,2.425));
#47213=CARTESIAN_POINT('',(-6.405,6.85189884122944E-16,2.45));
#47214=CARTESIAN_POINT('',(-6.43,7.87447891851748E-16,2.425));
#47215=CARTESIAN_POINT('Origin',(-6.,7.34788079488412E-16,2.45));
#47216=CARTESIAN_POINT('Origin',(-6.,7.34788079488412E-16,3.385));
#47217=CARTESIAN_POINT('',(-6.405,6.85189884122944E-16,4.4));
#47218=CARTESIAN_POINT('',(-6.405,6.85189884122944E-16,3.385));
#47219=CARTESIAN_POINT('Origin',(-6.,7.34788079488412E-16,4.4));
#47220=CARTESIAN_POINT('Origin',(-3.,-5.19615242270663,2.425));
#47221=CARTESIAN_POINT('',(-3.405,-5.19615242270663,2.45));
#47222=CARTESIAN_POINT('',(-3.43,-5.19615242270663,2.425));
#47223=CARTESIAN_POINT('Origin',(-3.,-5.19615242270663,2.45));
#47224=CARTESIAN_POINT('Origin',(-3.,-5.19615242270663,3.385));
#47225=CARTESIAN_POINT('',(-3.405,-5.19615242270663,4.4));
#47226=CARTESIAN_POINT('',(-3.405,-5.19615242270663,3.385));
#47227=CARTESIAN_POINT('Origin',(-3.,-5.19615242270663,4.4));
#47228=CARTESIAN_POINT('Origin',(3.,-5.19615242270663,2.425));
#47229=CARTESIAN_POINT('',(2.595,-5.19615242270663,2.45));
#47230=CARTESIAN_POINT('',(2.57,-5.19615242270663,2.425));
#47231=CARTESIAN_POINT('Origin',(3.,-5.19615242270663,2.45));
#47232=CARTESIAN_POINT('Origin',(3.,-5.19615242270663,3.385));
#47233=CARTESIAN_POINT('',(2.595,-5.19615242270663,4.4));
#47234=CARTESIAN_POINT('',(2.595,-5.19615242270663,3.385));
#47235=CARTESIAN_POINT('Origin',(3.,-5.19615242270663,4.4));
#47236=CARTESIAN_POINT('Origin',(3.,-5.19615242270663,4.4));
#47237=CARTESIAN_POINT('',(3.,-5.19615242270663,4.64334855070616));
#47238=CARTESIAN_POINT('',(2.595,-5.19615242270663,4.4));
#47239=CARTESIAN_POINT('Origin',(-3.,-5.19615242270663,4.4));
#47240=CARTESIAN_POINT('',(-3.,-5.19615242270663,4.64334855070616));
#47241=CARTESIAN_POINT('',(-3.405,-5.19615242270663,4.4));
#47242=CARTESIAN_POINT('Origin',(-6.,7.34788079488412E-16,4.4));
#47243=CARTESIAN_POINT('',(-6.,7.34788079488412E-16,4.64334855070616));
#47244=CARTESIAN_POINT('',(-6.405,6.85189884122944E-16,4.4));
#47245=CARTESIAN_POINT('Origin',(-3.,5.19615242270663,4.4));
#47246=CARTESIAN_POINT('',(-3.,5.19615242270663,4.64334855070616));
#47247=CARTESIAN_POINT('',(-3.405,5.19615242270663,4.4));
#47248=CARTESIAN_POINT('Origin',(3.,5.19615242270663,4.4));
#47249=CARTESIAN_POINT('',(3.,5.19615242270663,4.64334855070616));
#47250=CARTESIAN_POINT('',(2.595,5.19615242270663,4.4));
#47251=CARTESIAN_POINT('Origin',(6.,0.,4.4));
#47252=CARTESIAN_POINT('',(6.,0.,4.64334855070616));
#47253=CARTESIAN_POINT('',(5.595,-4.95981953654677E-17,4.4));
#47254=CARTESIAN_POINT('Origin',(0.,0.,2.43));
#47255=CARTESIAN_POINT('',(2.6,3.18408167778312E-16,2.46));
#47256=CARTESIAN_POINT('',(2.63,-3.22082108175754E-16,2.43));
#47257=CARTESIAN_POINT('',(-2.6,-3.18408167778312E-16,2.46));
#47258=CARTESIAN_POINT('Origin',(0.,0.,2.46));
#47259=CARTESIAN_POINT('Origin',(0.,0.,2.46));
#47260=CARTESIAN_POINT('Origin',(0.,0.,3.1));
#47261=CARTESIAN_POINT('',(-2.6,-3.18408167778312E-16,3.8));
#47262=CARTESIAN_POINT('Origin',(0.,0.,3.8));
#47263=CARTESIAN_POINT('',(-2.6,-3.18408167778312E-16,3.1));
#47264=CARTESIAN_POINT('Origin',(0.,0.,5.4));
#47265=CARTESIAN_POINT('Origin',(0.,0.,2.425));
#47266=CARTESIAN_POINT('',(-6.975,-8.54191142405279E-16,2.425));
#47267=CARTESIAN_POINT('Origin',(2.4,0.,4.6));
#47268=CARTESIAN_POINT('',(-2.4,-2.93915231795365E-16,4.6));
#47269=CARTESIAN_POINT('Origin',(0.,0.,4.6));
#47270=CARTESIAN_POINT('Origin',(0.,0.,4.2));
#47271=CARTESIAN_POINT('',(-2.4,-2.93915231795365E-16,3.8));
#47272=CARTESIAN_POINT('',(-2.4,-2.93915231795365E-16,4.2));
#47273=CARTESIAN_POINT('Origin',(0.,0.,3.8));
#47274=CARTESIAN_POINT('Origin',(2.6,0.,3.8));
#47275=CARTESIAN_POINT('',(0.,0.,0.));
#47276=CARTESIAN_POINT('Origin',(0.575,0.,3.7));
#47277=CARTESIAN_POINT('',(-0.6,-7.34788079488412E-17,3.7));
#47278=CARTESIAN_POINT('Origin',(0.,0.,3.7));
#47279=CARTESIAN_POINT('',(-0.575,-7.04171909509728E-17,3.7));
#47280=CARTESIAN_POINT('Origin',(0.,0.,3.7));
#47281=CARTESIAN_POINT('Origin',(0.,0.,3.65));
#47282=CARTESIAN_POINT('',(-0.575,-7.04171909509728E-17,3.6));
#47283=CARTESIAN_POINT('Origin',(0.,0.,3.6));
#47284=CARTESIAN_POINT('',(-0.575,-7.04171909509728E-17,3.65));
#47285=CARTESIAN_POINT('Origin',(0.61,0.,3.6));
#47286=CARTESIAN_POINT('',(-0.6,7.34788079488412E-17,3.6));
#47287=CARTESIAN_POINT('Origin',(0.,0.,3.6));
#47288=CARTESIAN_POINT('Origin',(0.,0.,2.6));
#47289=CARTESIAN_POINT('',(-0.6,-7.34788079488412E-17,3.1));
#47290=CARTESIAN_POINT('',(-0.6,-7.34788079488412E-17,2.6));
#47291=CARTESIAN_POINT('Origin',(0.,0.,3.1));
#47292=CARTESIAN_POINT('Origin',(0.575,0.,3.1));
#47293=CARTESIAN_POINT('',(-0.575,-7.04171909509728E-17,3.1));
#47294=CARTESIAN_POINT('Origin',(0.,0.,3.1));
#47295=CARTESIAN_POINT('Origin',(0.,0.,3.05));
#47296=CARTESIAN_POINT('',(-0.575,-7.04171909509728E-17,3.));
#47297=CARTESIAN_POINT('Origin',(0.,0.,3.));
#47298=CARTESIAN_POINT('',(-0.575,-7.04171909509728E-17,3.05));
#47299=CARTESIAN_POINT('Origin',(0.61,0.,3.));
#47300=CARTESIAN_POINT('',(-0.6,7.34788079488412E-17,3.));
#47301=CARTESIAN_POINT('Origin',(0.,0.,3.));
#47302=CARTESIAN_POINT('Origin',(0.,0.,2.6));
#47303=CARTESIAN_POINT('',(-0.6,-7.34788079488412E-17,0.66));
#47304=CARTESIAN_POINT('',(-0.6,-7.34788079488412E-17,2.6));
#47305=CARTESIAN_POINT('Origin',(0.,0.,0.66));
#47306=CARTESIAN_POINT('Origin',(0.,0.,0.442705098312484));
#47307=CARTESIAN_POINT('',(-0.3,-3.67394039744206E-17,0.55));
#47308=CARTESIAN_POINT('Origin',(0.,0.,0.55));
#47309=CARTESIAN_POINT('',(-0.3,-3.67394039744206E-17,0.335410196624968));
#47310=CARTESIAN_POINT('',(-0.3,-3.67394039744206E-17,0.442705098312484));
#47311=CARTESIAN_POINT('Origin',(0.,0.,0.335410196624968));
#47312=CARTESIAN_POINT('Origin',(0.,0.,0.575));
#47313=CARTESIAN_POINT('',(-0.54,-6.61309271539571E-17,0.6));
#47314=CARTESIAN_POINT('Origin',(0.,0.,0.6));
#47315=CARTESIAN_POINT('',(-0.42,-5.14351655641888E-17,0.575));
#47316=CARTESIAN_POINT('Origin',(0.,0.,0.63));
#47317=CARTESIAN_POINT('',(-0.57,-6.98048675513991E-17,0.63));
#47318=CARTESIAN_POINT('Origin',(0.,0.,2.6));
#47319=CARTESIAN_POINT('',(-0.6,-7.34788079488412E-17,4.54));
#47320=CARTESIAN_POINT('Origin',(0.,0.,4.54));
#47321=CARTESIAN_POINT('',(-0.6,-7.34788079488412E-17,2.6));
#47322=CARTESIAN_POINT('Origin',(0.,0.,4.57));
#47323=CARTESIAN_POINT('',(-0.54,-6.61309271539571E-17,4.6));
#47324=CARTESIAN_POINT('Origin',(0.,0.,4.6));
#47325=CARTESIAN_POINT('',(-0.57,-6.98048675513991E-17,4.57));
#47326=CARTESIAN_POINT('Origin',(0.25,0.,4.6));
#47327=CARTESIAN_POINT('',(-0.25,-3.06161699786838E-17,4.6));
#47328=CARTESIAN_POINT('Origin',(0.,0.,4.6));
#47329=CARTESIAN_POINT('Origin',(0.,0.,2.725));
#47330=CARTESIAN_POINT('',(-0.25,-3.06161699786838E-17,0.85));
#47331=CARTESIAN_POINT('',(-0.25,-3.06161699786838E-17,2.725));
#47332=CARTESIAN_POINT('Origin',(0.,0.,0.85));
#47333=CARTESIAN_POINT('Origin',(0.,0.,0.825));
#47334=CARTESIAN_POINT('',(-0.075,-9.18485099360515E-18,0.8));
#47335=CARTESIAN_POINT('',(-0.1625,-1.99005104861445E-17,0.825));
#47336=CARTESIAN_POINT('Origin',(0.,0.,0.8));
#47337=CARTESIAN_POINT('Origin',(0.,0.,0.178147008133764));
#47338=CARTESIAN_POINT('',(-0.075,-9.18485099360515E-18,-0.443705983732471));
#47339=CARTESIAN_POINT('',(-0.075,-9.18485099360515E-18,0.178147008133764));
#47340=CARTESIAN_POINT('Origin',(0.,0.,-0.443705983732471));
#47341=CARTESIAN_POINT('Origin',(0.,0.,0.));
#47342=CARTESIAN_POINT('Origin',(0.,0.,0.));
#47343=CARTESIAN_POINT('',(0.,0.,0.));
#47344=CARTESIAN_POINT('Origin',(0.,0.,-0.6));
#47345=CARTESIAN_POINT('',(-0.59,-7.22541611496939E-17,-0.6));
#47346=CARTESIAN_POINT('Origin',(0.,0.,-0.6));
#47347=CARTESIAN_POINT('',(-0.59,-7.22541611496939E-17,-0.56));
#47348=CARTESIAN_POINT('',(-0.59,-7.22541611496939E-17,-0.6));
#47349=CARTESIAN_POINT('Origin',(0.,0.,-0.56));
#47350=CARTESIAN_POINT('Origin',(0.,0.,-0.6));
#47351=CARTESIAN_POINT('',(-0.65,-7.9602041944578E-17,-0.6));
#47352=CARTESIAN_POINT('Origin',(0.,0.,-0.6));
#47353=CARTESIAN_POINT('',(-0.65,-7.9602041944578E-17,-0.56));
#47354=CARTESIAN_POINT('',(-0.65,-7.9602041944578E-17,-0.6));
#47355=CARTESIAN_POINT('Origin',(0.,0.,-0.56));
#47356=CARTESIAN_POINT('Origin',(0.,0.,-0.56));
#47357=CARTESIAN_POINT('Origin',(0.76,0.,-0.6));
#47358=CARTESIAN_POINT('',(-0.76,-9.30731567351988E-17,-0.6));
#47359=CARTESIAN_POINT('Origin',(0.,0.,-0.6));
#47360=CARTESIAN_POINT('Origin',(0.,0.,0.));
#47361=CARTESIAN_POINT('',(-0.405344298097309,-4.964035972175E-17,0.2));
#47362=CARTESIAN_POINT('Origin',(0.,0.,0.2));
#47363=CARTESIAN_POINT('',(-0.075,-9.18485099360515E-18,-0.445734225744445));
#47364=CARTESIAN_POINT('Origin',(0.,0.,0.));
#47365=CARTESIAN_POINT('Origin',(0.,0.,-0.445734225744445));
#47366=CARTESIAN_POINT('Origin',(0.,0.,-0.497867112872223));
#47367=CARTESIAN_POINT('',(-0.075,-9.18485099360515E-18,-0.55));
#47368=CARTESIAN_POINT('',(-0.075,-9.18485099360515E-18,-0.497867112872223));
#47369=CARTESIAN_POINT('Origin',(0.,0.,-0.55));
#47370=CARTESIAN_POINT('Origin',(0.4,0.,-0.55));
#47371=CARTESIAN_POINT('',(-0.4,-4.89858719658941E-17,-0.55));
#47372=CARTESIAN_POINT('Origin',(0.,0.,-0.55));
#47373=CARTESIAN_POINT('Origin',(0.,0.,-0.575));
#47374=CARTESIAN_POINT('',(-0.4,-4.89858719658941E-17,-0.6));
#47375=CARTESIAN_POINT('',(-0.4,-4.89858719658941E-17,-0.575));
#47376=CARTESIAN_POINT('Origin',(0.,0.,-0.6));
#47377=CARTESIAN_POINT('Origin',(0.76,0.,-0.6));
#47378=CARTESIAN_POINT('Origin',(0.,0.,-0.58));
#47379=CARTESIAN_POINT('',(-0.8,-9.79717439317883E-17,-0.56));
#47380=CARTESIAN_POINT('Origin',(0.,0.,-0.56));
#47381=CARTESIAN_POINT('',(-0.78,-9.55224503334935E-17,-0.58));
#47382=CARTESIAN_POINT('Origin',(0.,0.,-0.45));
#47383=CARTESIAN_POINT('',(-0.8,-9.79717439317883E-17,-0.34));
#47384=CARTESIAN_POINT('Origin',(0.,0.,-0.34));
#47385=CARTESIAN_POINT('',(-0.8,-9.79717439317883E-17,-0.45));
#47386=CARTESIAN_POINT('Origin',(0.,0.,-0.32));
#47387=CARTESIAN_POINT('',(-0.76,-9.30731567351988E-17,-0.3));
#47388=CARTESIAN_POINT('Origin',(0.,0.,-0.3));
#47389=CARTESIAN_POINT('',(-0.78,-9.55224503334935E-17,-0.32));
#47390=CARTESIAN_POINT('Origin',(0.55,0.,-0.3));
#47391=CARTESIAN_POINT('',(-0.55,-6.73555739531044E-17,-0.3));
#47392=CARTESIAN_POINT('Origin',(0.,0.,-0.3));
#47393=CARTESIAN_POINT('Origin',(0.,0.,-0.07));
#47394=CARTESIAN_POINT('',(-0.55,-6.73555739531044E-17,0.16));
#47395=CARTESIAN_POINT('Origin',(0.,0.,0.16));
#47396=CARTESIAN_POINT('',(-0.55,-6.73555739531044E-17,-0.07));
#47397=CARTESIAN_POINT('Origin',(0.,0.,0.18));
#47398=CARTESIAN_POINT('',(-0.51,-6.2456986756515E-17,0.2));
#47399=CARTESIAN_POINT('Origin',(0.,0.,0.2));
#47400=CARTESIAN_POINT('',(-0.53,-6.49062803548097E-17,0.18));
#47401=CARTESIAN_POINT('Origin',(0.405344298097309,0.,0.2));
#47402=CARTESIAN_POINT('',(0.,0.,0.));
#47403=CARTESIAN_POINT('Origin',(0.,0.,0.817011318356283));
#47404=CARTESIAN_POINT('',(-1.75488973075546,-2.14912009162623E-16,1.44791652082959));
#47405=CARTESIAN_POINT('Origin',(0.,0.,1.44791652082959));
#47406=CARTESIAN_POINT('',(-2.02309581191037,-2.47757781042445E-16,0.186106115882978));
#47407=CARTESIAN_POINT('',(-1.88899277133291,-2.31334895102534E-16,0.817011318356283));
#47408=CARTESIAN_POINT('Origin',(0.,0.,0.186106115882978));
#47409=CARTESIAN_POINT('',(1.96553101732603,-0.404034822633264,0.263580625276104));
#47410=CARTESIAN_POINT('',(1.72474144876727,-1.02558434703109,0.263580625276103));
#47411=CARTESIAN_POINT('Origin',(-0.0884849938604435,0.0342792692444314,
-0.177187331777248));
#47412=CARTESIAN_POINT('',(1.73109633135173,-0.356297004039415,1.38914111564877));
#47413=CARTESIAN_POINT('Ctrl Pts',(1.96553101732603,-0.404034822633264,
0.263580625276103));
#47414=CARTESIAN_POINT('Ctrl Pts',(1.88793646815053,-0.388221893764485,
0.636136973435854));
#47415=CARTESIAN_POINT('Ctrl Pts',(1.80874957916707,-0.37209543523409,1.0163282025572));
#47416=CARTESIAN_POINT('Ctrl Pts',(1.73109633135173,-0.356297004039416,
1.38914111564877));
#47417=CARTESIAN_POINT('',(1.51933136490257,-0.902925394000066,1.38914111564877));
#47418=CARTESIAN_POINT('Origin',(-0.0779352888697595,0.0301922917576571,
1.00090915210539));
#47419=CARTESIAN_POINT('Ctrl Pts',(1.51933136490257,-0.902925394000065,
1.38914111564877));
#47420=CARTESIAN_POINT('Ctrl Pts',(1.58736114175433,-0.94356486723299,1.01632820259676));
#47421=CARTESIAN_POINT('Ctrl Pts',(1.65674528369834,-0.984995132717264,
0.636136973481484));
#47422=CARTESIAN_POINT('Ctrl Pts',(1.72474144876727,-1.02558434703109,0.263580625276103));
#47423=CARTESIAN_POINT('',(1.68684887716375,-1.08678295145922,0.263580625276104));
#47424=CARTESIAN_POINT('',(1.23778970554114,-1.57937739721302,0.263580625276103));
#47425=CARTESIAN_POINT('Origin',(-0.0701266991563423,0.063928933229414,
-0.177187331777248));
#47426=CARTESIAN_POINT('',(1.48548993201256,-0.957581184754694,1.38914111564877));
#47427=CARTESIAN_POINT('Ctrl Pts',(1.68684887716375,-1.08678295145922,0.263580625276104));
#47428=CARTESIAN_POINT('Ctrl Pts',(1.62014150671713,-1.04396579507641,0.636499771706221));
#47429=CARTESIAN_POINT('Ctrl Pts',(1.55215789194248,-1.00034225256772,1.0165209491176));
#47430=CARTESIAN_POINT('Ctrl Pts',(1.48548993201256,-0.957581184754693,
1.38914111564877));
#47431=CARTESIAN_POINT('',(1.09056003126339,-1.39079864887685,1.38914111564877));
#47432=CARTESIAN_POINT('Origin',(-0.0617657787811128,0.0563069472121782,
1.00090915210539));
#47433=CARTESIAN_POINT('Ctrl Pts',(1.09056003126339,-1.39079864887685,1.38914111564877));
#47434=CARTESIAN_POINT('Ctrl Pts',(1.13929003118602,-1.45323672146031,1.01652094915712));
#47435=CARTESIAN_POINT('Ctrl Pts',(1.18900021995803,-1.51690525741751,0.636499771750218));
#47436=CARTESIAN_POINT('Ctrl Pts',(1.23778970554114,-1.57937739721302,0.263580625276103));
#47437=CARTESIAN_POINT('',(1.18034844898819,-1.62275502061838,0.263580625276103));
#47438=CARTESIAN_POINT('',(0.583667603752152,-1.91986677826906,0.263580625276103));
#47439=CARTESIAN_POINT('Origin',(-0.0422974051457228,0.0849446405393159,
-0.177187331777248));
#47440=CARTESIAN_POINT('',(1.03925988597122,-1.42953872032833,1.38914111564877));
#47441=CARTESIAN_POINT('Ctrl Pts',(1.18034844898819,-1.62275502061838,0.263580625276103));
#47442=CARTESIAN_POINT('Ctrl Pts',(1.1336409924622,-1.55877005016848,0.636276564880181));
#47443=CARTESIAN_POINT('Ctrl Pts',(1.08599375050078,-1.49351590217855,1.01640192898384));
#47444=CARTESIAN_POINT('Ctrl Pts',(1.03925988597122,-1.42953872032833,1.38914111564877));
#47445=CARTESIAN_POINT('',(0.514502522400341,-1.69083683954147,1.38914111564877));
#47446=CARTESIAN_POINT('Origin',(-0.0372544580120808,0.0748170374381298,
1.00090915210539));
#47447=CARTESIAN_POINT('Ctrl Pts',(0.514502522400341,-1.69083683954147,
1.38914111564877));
#47448=CARTESIAN_POINT('Ctrl Pts',(0.537393970209863,-1.76668613424626,
1.0164019290234));
#47449=CARTESIAN_POINT('Ctrl Pts',(0.560754026123086,-1.8440338639089,0.636276564925202));
#47450=CARTESIAN_POINT('Ctrl Pts',(0.583667603752152,-1.91986677826906,
0.263580625276104));
#47451=CARTESIAN_POINT('',(0.514435422240241,-1.93956503224705,0.263580625276104));
#47452=CARTESIAN_POINT('',(-0.149282042137411,-2.0010675125708,0.263580625276104));
#47453=CARTESIAN_POINT('Origin',(-0.00875561219215992,0.0944881034498817,
-0.177187331777248));
#47454=CARTESIAN_POINT('',(0.452672033591646,-1.70842913037413,1.38914111564877));
#47455=CARTESIAN_POINT('Ctrl Pts',(0.514435422240241,-1.93956503224705,
0.263580625276104));
#47456=CARTESIAN_POINT('Ctrl Pts',(0.4940205153564,-1.86311974435583,0.6358305212866));
#47457=CARTESIAN_POINT('Ctrl Pts',(0.473150118322512,-1.78501046959186,
1.01619654162157));
#47458=CARTESIAN_POINT('Ctrl Pts',(0.452672033591646,-1.70842913037413,
1.38914111564877));
#47459=CARTESIAN_POINT('',(-0.131041403069769,-1.76251814577564,1.38914111564877));
#47460=CARTESIAN_POINT('Origin',(-0.00771171625443978,0.0832226721825453,
1.00090915210539));
#47461=CARTESIAN_POINT('Ctrl Pts',(-0.131041403069769,-1.76251814577564,
1.38914111564877));
#47462=CARTESIAN_POINT('Ctrl Pts',(-0.137099025337607,-1.84155838035113,
1.01619654166127));
#47463=CARTESIAN_POINT('Ctrl Pts',(-0.143261522626645,-1.92217262167001,
0.63583052133358));
#47464=CARTESIAN_POINT('Ctrl Pts',(-0.149282042137411,-2.0010675125708,
0.263580625276104));
#47465=CARTESIAN_POINT('',(-0.220954958866336,-1.9944260387699,0.263580625276103));
#47466=CARTESIAN_POINT('',(-0.862070321035964,-1.81201299100198,0.263580625276103));
#47467=CARTESIAN_POINT('Origin',(0.0259686747044756,0.0912704244128846,
-0.177187331777247));
#47468=CARTESIAN_POINT('',(-0.195051685266811,-1.75658671963028,1.38914111564877));
#47469=CARTESIAN_POINT('Ctrl Pts',(-0.220954958866336,-1.9944260387699,
0.263580625276103));
#47470=CARTESIAN_POINT('Ctrl Pts',(-0.212371888991068,-1.91572988628875,
0.636011916383804));
#47471=CARTESIAN_POINT('Ctrl Pts',(-0.203619189092551,-1.83537931742317,
1.0162671092937));
#47472=CARTESIAN_POINT('Ctrl Pts',(-0.195051685266812,-1.75658671963028,
1.38914111564877));
#47473=CARTESIAN_POINT('',(-0.758887460929825,-1.59616160997261,1.38914111564877));
#47474=CARTESIAN_POINT('Origin',(0.0228725355154589,0.0803886238959624,
1.00090915210539));
#47475=CARTESIAN_POINT('Ctrl Pts',(-0.758887460929825,-1.59616160997261,
1.38914111564877));
#47476=CARTESIAN_POINT('Ctrl Pts',(-0.79308218003796,-1.66766263634664,
1.01626710933327));
#47477=CARTESIAN_POINT('Ctrl Pts',(-0.827939608356074,-1.7405857695991,
0.636011916429978));
#47478=CARTESIAN_POINT('Ctrl Pts',(-0.862070321035964,-1.81201299100198,
0.263580625276103));
#47479=CARTESIAN_POINT('',(-0.92650414842432,-1.77992875726067,0.263580625276104));
#47480=CARTESIAN_POINT('',(-1.45843122618206,-1.37823607428775,0.263580625276103));
#47481=CARTESIAN_POINT('Origin',(0.0571857481848785,0.0757261688120474,
-0.177187331777248));
#47482=CARTESIAN_POINT('',(-0.816432593211287,-1.56750753881733,1.38914111564877));
#47483=CARTESIAN_POINT('Ctrl Pts',(-0.926504148424321,-1.77992875726068,
0.263580625276104));
#47484=CARTESIAN_POINT('Ctrl Pts',(-0.890024902524132,-1.70955582085882,
0.636496905193193));
#47485=CARTESIAN_POINT('Ctrl Pts',(-0.852859726540045,-1.63783625100815,
1.01652279052734));
#47486=CARTESIAN_POINT('Ctrl Pts',(-0.816432593211287,-1.56750753881733,
1.38914111564877));
#47487=CARTESIAN_POINT('',(-1.28424156205072,-1.21423460410598,1.38914111564877));
#47488=CARTESIAN_POINT('Origin',(0.0503677246228997,0.0666976465034872,
1.00090915210539));
#47489=CARTESIAN_POINT('Ctrl Pts',(-1.28424156205072,-1.21423460410598,
1.38914111564877));
#47490=CARTESIAN_POINT('Ctrl Pts',(-1.34191676265454,-1.26851752070915,
1.01652279056689));
#47491=CARTESIAN_POINT('Ctrl Pts',(-1.4007277508672,-1.32389093193504,0.63649690523722));
#47492=CARTESIAN_POINT('Ctrl Pts',(-1.45843122618206,-1.37823607428775,
0.263580625276104));
#47493=CARTESIAN_POINT('',(-1.50692381880089,-1.32504223415768,0.263580625276104));
#47494=CARTESIAN_POINT('',(-1.85782291278586,-0.758320738671227,0.263580625276103));
#47495=CARTESIAN_POINT('Origin',(0.080679569495743,0.0499546744999564,-0.177187331777248));
#47496=CARTESIAN_POINT('',(-1.32754975543341,-1.16672777902799,1.38914111564877));
#47497=CARTESIAN_POINT('Ctrl Pts',(-1.50692381880088,-1.32504223415768,
0.263580625276104));
#47498=CARTESIAN_POINT('Ctrl Pts',(-1.44749808261794,-1.27260964643021,
0.636422969016795));
#47499=CARTESIAN_POINT('Ctrl Pts',(-1.38692897637993,-1.21915388714204,
1.01648344351096));
#47500=CARTESIAN_POINT('Ctrl Pts',(-1.32754975543341,-1.16672777902799,
1.38914111564877));
#47501=CARTESIAN_POINT('',(-1.63615172398851,-0.668318486648626,1.38914111564877));
#47502=CARTESIAN_POINT('Origin',(0.0710604734228215,0.0439987823662984,
1.00090915210539));
#47503=CARTESIAN_POINT('Ctrl Pts',(-1.63615172398851,-0.668318486648626,
1.38914111564877));
#47504=CARTESIAN_POINT('Ctrl Pts',(-1.70954924778502,-0.698104258275537,
1.01648344355053));
#47505=CARTESIAN_POINT('Ctrl Pts',(-1.78439885503574,-0.728496216517704,
0.636422969061169));
#47506=CARTESIAN_POINT('Ctrl Pts',(-1.85782291278586,-0.758320738671227,
0.263580625276103));
#47507=CARTESIAN_POINT('',(-1.88382507729525,-0.691201415019197,0.263580625276104));
#47508=CARTESIAN_POINT('',(-2.00630532046579,-0.0359899852968828,0.263580625276104));
#47509=CARTESIAN_POINT('Origin',(0.0932771678852804,0.0174365245882386,
-0.177187331777248));
#47510=CARTESIAN_POINT('',(-1.6593739669771,-0.608374967619113,1.38914111564877));
#47511=CARTESIAN_POINT('Ctrl Pts',(-1.88382507729525,-0.691201415019197,
0.263580625276104));
#47512=CARTESIAN_POINT('Ctrl Pts',(-1.80957400607897,-0.663814383089077,
0.635908422736754));
#47513=CARTESIAN_POINT('Ctrl Pts',(-1.73373386455056,-0.635829781577252,
1.01622302039257));
#47514=CARTESIAN_POINT('Ctrl Pts',(-1.6593739669771,-0.608374967619113,
1.38914111564877));
#47515=CARTESIAN_POINT('',(-1.76709052937197,-0.0321422542887969,1.38914111564877));
#47516=CARTESIAN_POINT('Origin',(0.0821561115273148,0.0153576388648713,
1.00090915210539));
#47517=CARTESIAN_POINT('Ctrl Pts',(-1.76709052937197,-0.032142254288797,
1.38914111564877));
#47518=CARTESIAN_POINT('Ctrl Pts',(-1.84634689157125,-0.0334032960061751,
1.01622302043219));
#47519=CARTESIAN_POINT('Ctrl Pts',(-1.92717492149681,-0.0347050513350173,
0.635908422783382));
#47520=CARTESIAN_POINT('Ctrl Pts',(-2.00630532046579,-0.0359899852968828,
0.263580625276103));
#47521=CARTESIAN_POINT('',(-2.00630532046579,0.0359899852968833,0.263580625276103));
#47522=CARTESIAN_POINT('',(-1.88382507729525,0.691201415019197,0.263580625276103));
#47523=CARTESIAN_POINT('Origin',(0.0932771678852804,-0.0174365245882386,
-0.177187331777248));
#47524=CARTESIAN_POINT('',(-1.76709052937197,0.0321422542887974,1.38914111564877));
#47525=CARTESIAN_POINT('Ctrl Pts',(-2.00630532046579,0.0359899852968834,
0.263580625276103));
#47526=CARTESIAN_POINT('Ctrl Pts',(-1.92717492150672,0.0347050513351788,
0.635908422736753));
#47527=CARTESIAN_POINT('Ctrl Pts',(-1.84634689157967,0.0334032960063096,
1.01622302039257));
#47528=CARTESIAN_POINT('Ctrl Pts',(-1.76709052937197,0.0321422542887974,
1.38914111564877));
#47529=CARTESIAN_POINT('',(-1.6593739669771,0.608374967619113,1.38914111564877));
#47530=CARTESIAN_POINT('Origin',(0.0821561115273148,-0.0153576388648713,
1.00090915210539));
#47531=CARTESIAN_POINT('Ctrl Pts',(-1.6593739669771,0.608374967619113,1.38914111564877));
#47532=CARTESIAN_POINT('Ctrl Pts',(-1.73373386454266,0.635829781574335,
1.01622302043219));
#47533=CARTESIAN_POINT('Ctrl Pts',(-1.80957400606967,0.663814383085648,
0.635908422783382));
#47534=CARTESIAN_POINT('Ctrl Pts',(-1.88382507729525,0.691201415019197,
0.263580625276103));
#47535=CARTESIAN_POINT('',(-1.85782291278586,0.758320738671226,0.263580625276104));
#47536=CARTESIAN_POINT('',(-1.50692381880089,1.32504223415768,0.263580625276103));
#47537=CARTESIAN_POINT('Origin',(0.0806795694957425,-0.0499546744999564,
-0.177187331777248));
#47538=CARTESIAN_POINT('',(-1.63615172398851,0.668318486648626,1.38914111564877));
#47539=CARTESIAN_POINT('Ctrl Pts',(-1.85782291278586,0.758320738671226,
0.263580625276104));
#47540=CARTESIAN_POINT('Ctrl Pts',(-1.78439885504448,0.728496216521253,
0.636422969016796));
#47541=CARTESIAN_POINT('Ctrl Pts',(-1.70954924779282,0.698104258278699,
1.01648344351096));
#47542=CARTESIAN_POINT('Ctrl Pts',(-1.63615172398851,0.668318486648626,
1.38914111564877));
#47543=CARTESIAN_POINT('',(-1.32754975543341,1.16672777902799,1.38914111564877));
#47544=CARTESIAN_POINT('Origin',(0.0710604734228211,-0.0439987823662986,
1.00090915210539));
#47545=CARTESIAN_POINT('Ctrl Pts',(-1.32754975543341,1.16672777902799,1.38914111564877));
#47546=CARTESIAN_POINT('Ctrl Pts',(-1.38692897637363,1.21915388713648,1.01648344355052));
#47547=CARTESIAN_POINT('Ctrl Pts',(-1.44749808261087,1.27260964642397,0.636422969061169));
#47548=CARTESIAN_POINT('Ctrl Pts',(-1.50692381880089,1.32504223415768,0.263580625276103));
#47549=CARTESIAN_POINT('',(-1.45843122618206,1.37823607428775,0.263580625276103));
#47550=CARTESIAN_POINT('',(-0.92650414842432,1.77992875726068,0.263580625276103));
#47551=CARTESIAN_POINT('Origin',(0.0571857481848781,-0.0757261688120474,
-0.177187331777248));
#47552=CARTESIAN_POINT('',(-1.28424156205072,1.21423460410598,1.38914111564877));
#47553=CARTESIAN_POINT('Ctrl Pts',(-1.45843122618206,1.37823607428775,0.263580625276103));
#47554=CARTESIAN_POINT('Ctrl Pts',(-1.40072775087401,1.32389093194146,0.636496905193193));
#47555=CARTESIAN_POINT('Ctrl Pts',(-1.34191676266067,1.26851752071491,1.01652279052734));
#47556=CARTESIAN_POINT('Ctrl Pts',(-1.28424156205072,1.21423460410598,1.38914111564877));
#47557=CARTESIAN_POINT('',(-0.816432593211287,1.56750753881733,1.38914111564877));
#47558=CARTESIAN_POINT('Origin',(0.0503677246229,-0.066697646503487,1.00090915210539));
#47559=CARTESIAN_POINT('Ctrl Pts',(-0.816432593211287,1.56750753881734,
1.38914111564877));
#47560=CARTESIAN_POINT('Ctrl Pts',(-0.852859726536179,1.63783625100069,
1.01652279056688));
#47561=CARTESIAN_POINT('Ctrl Pts',(-0.890024902519824,1.70955582085052,
0.63649690523722));
#47562=CARTESIAN_POINT('Ctrl Pts',(-0.92650414842432,1.77992875726068,0.263580625276103));
#47563=CARTESIAN_POINT('',(-0.862070321035964,1.81201299100198,0.263580625276104));
#47564=CARTESIAN_POINT('',(-0.220954958866335,1.9944260387699,0.263580625276103));
#47565=CARTESIAN_POINT('Origin',(0.0259686747044761,-0.091270424412885,
-0.177187331777248));
#47566=CARTESIAN_POINT('',(-0.758887460929825,1.59616160997261,1.38914111564877));
#47567=CARTESIAN_POINT('Ctrl Pts',(-0.862070321035964,1.81201299100198,
0.263580625276104));
#47568=CARTESIAN_POINT('Ctrl Pts',(-0.827939608360305,1.74058576960796,
0.636011916383804));
#47569=CARTESIAN_POINT('Ctrl Pts',(-0.793082180041589,1.66766263635423,
1.0162671092937));
#47570=CARTESIAN_POINT('Ctrl Pts',(-0.758887460929825,1.59616160997261,
1.38914111564877));
#47571=CARTESIAN_POINT('',(-0.195051685266811,1.75658671963028,1.38914111564877));
#47572=CARTESIAN_POINT('Origin',(0.0228725355154586,-0.0803886238959621,
1.00090915210539));
#47573=CARTESIAN_POINT('Ctrl Pts',(-0.195051685266811,1.75658671963028,
1.38914111564877));
#47574=CARTESIAN_POINT('Ctrl Pts',(-0.203619189091641,1.83537931741481,
1.01626710933327));
#47575=CARTESIAN_POINT('Ctrl Pts',(-0.212371888990004,1.91572988627899,
0.636011916429979));
#47576=CARTESIAN_POINT('Ctrl Pts',(-0.220954958866335,1.9944260387699,0.263580625276103));
#47577=CARTESIAN_POINT('',(-0.14928204213741,2.0010675125708,0.263580625276104));
#47578=CARTESIAN_POINT('',(0.514435422240242,1.93956503224705,0.263580625276103));
#47579=CARTESIAN_POINT('Origin',(-0.00875561219215948,-0.0944881034498812,
-0.177187331777248));
#47580=CARTESIAN_POINT('',(-0.131041403069769,1.76251814577564,1.38914111564877));
#47581=CARTESIAN_POINT('Ctrl Pts',(-0.14928204213741,2.0010675125708,0.263580625276104));
#47582=CARTESIAN_POINT('Ctrl Pts',(-0.143261522627404,1.92217262167996,
0.635830521286599));
#47583=CARTESIAN_POINT('Ctrl Pts',(-0.137099025338251,1.84155838035954,
1.01619654162157));
#47584=CARTESIAN_POINT('Ctrl Pts',(-0.131041403069769,1.76251814577564,
1.38914111564877));
#47585=CARTESIAN_POINT('',(0.452672033591647,1.70842913037412,1.38914111564877));
#47586=CARTESIAN_POINT('Origin',(-0.00771171625443956,-0.0832226721825451,
1.00090915210539));
#47587=CARTESIAN_POINT('Ctrl Pts',(0.452672033591647,1.70842913037413,1.38914111564877));
#47588=CARTESIAN_POINT('Ctrl Pts',(0.473150118320333,1.78501046958371,1.01619654166127));
#47589=CARTESIAN_POINT('Ctrl Pts',(0.494020515353825,1.86311974434618,0.63583052133358));
#47590=CARTESIAN_POINT('Ctrl Pts',(0.514435422240242,1.93956503224705,0.263580625276104));
#47591=CARTESIAN_POINT('',(0.583667603752152,1.91986677826906,0.263580625276103));
#47592=CARTESIAN_POINT('',(1.18034844898819,1.62275502061838,0.263580625276103));
#47593=CARTESIAN_POINT('Origin',(-0.0422974051457223,-0.0849446405393151,
-0.177187331777248));
#47594=CARTESIAN_POINT('',(0.514502522400341,1.69083683954147,1.38914111564877));
#47595=CARTESIAN_POINT('Ctrl Pts',(0.583667603752152,1.91986677826906,0.263580625276104));
#47596=CARTESIAN_POINT('Ctrl Pts',(0.560754026125854,1.84403386391806,0.636276564880181));
#47597=CARTESIAN_POINT('Ctrl Pts',(0.537393970212291,1.76668613425431,1.01640192898384));
#47598=CARTESIAN_POINT('Ctrl Pts',(0.514502522400341,1.69083683954147,1.38914111564877));
#47599=CARTESIAN_POINT('',(1.03925988597122,1.42953872032833,1.38914111564877));
#47600=CARTESIAN_POINT('Origin',(-0.0372544580120806,-0.074817037438129,
1.00090915210539));
#47601=CARTESIAN_POINT('Ctrl Pts',(1.03925988597122,1.42953872032833,1.38914111564877));
#47602=CARTESIAN_POINT('Ctrl Pts',(1.08599375049582,1.49351590217177,1.0164019290234));
#47603=CARTESIAN_POINT('Ctrl Pts',(1.13364099245656,1.55877005016075,0.636276564925202));
#47604=CARTESIAN_POINT('Ctrl Pts',(1.18034844898819,1.62275502061838,0.263580625276103));
#47605=CARTESIAN_POINT('',(1.23778970554114,1.57937739721302,0.263580625276104));
#47606=CARTESIAN_POINT('',(1.68684887716375,1.08678295145922,0.263580625276104));
#47607=CARTESIAN_POINT('Origin',(-0.0701266991563427,-0.0639289332294135,
-0.177187331777248));
#47608=CARTESIAN_POINT('',(1.09056003126339,1.39079864887685,1.38914111564877));
#47609=CARTESIAN_POINT('Ctrl Pts',(1.23778970554114,1.57937739721302,0.263580625276103));
#47610=CARTESIAN_POINT('Ctrl Pts',(1.1890002199638,1.51690525742489,0.636499771706133));
#47611=CARTESIAN_POINT('Ctrl Pts',(1.1392900311912,1.45323672146694,1.01652094911755));
#47612=CARTESIAN_POINT('Ctrl Pts',(1.09056003126339,1.39079864887685,1.38914111564877));
#47613=CARTESIAN_POINT('',(1.48548993201256,0.957581184754693,1.38914111564877));
#47614=CARTESIAN_POINT('Origin',(-0.061765778781113,-0.0563069472121784,
1.00090915210539));
#47615=CARTESIAN_POINT('Ctrl Pts',(1.48548993201256,0.957581184754694,1.38914111564877));
#47616=CARTESIAN_POINT('Ctrl Pts',(1.55215789193542,1.00034225256319,1.01652094915707));
#47617=CARTESIAN_POINT('Ctrl Pts',(1.62014150670928,1.04396579507136,0.636499771750131));
#47618=CARTESIAN_POINT('Ctrl Pts',(1.68684887716375,1.08678295145922,0.263580625276104));
#47619=CARTESIAN_POINT('',(1.72474144876727,1.02558434703109,0.263580625276104));
#47620=CARTESIAN_POINT('',(1.96553101732603,0.404034822633264,0.263580625276104));
#47621=CARTESIAN_POINT('Origin',(-0.0884849938604444,-0.0342792692444314,
-0.177187331777248));
#47622=CARTESIAN_POINT('',(1.51933136490257,0.902925394000065,1.38914111564877));
#47623=CARTESIAN_POINT('Ctrl Pts',(1.72474144876727,1.02558434703109,0.263580625276104));
#47624=CARTESIAN_POINT('Ctrl Pts',(1.6567452837067,0.984995132722253,0.636136973435691));
#47625=CARTESIAN_POINT('Ctrl Pts',(1.58736114176157,0.943564867237314,1.0163282025571));
#47626=CARTESIAN_POINT('Ctrl Pts',(1.51933136490257,0.902925394000065,1.38914111564877));
#47627=CARTESIAN_POINT('',(1.73109633135173,0.356297004039415,1.38914111564877));
#47628=CARTESIAN_POINT('Origin',(-0.07793528886976,-0.0301922917576571,
1.00090915210539));
#47629=CARTESIAN_POINT('Ctrl Pts',(1.73109633135173,0.356297004039415,1.38914111564877));
#47630=CARTESIAN_POINT('Ctrl Pts',(1.80874957915885,0.372095435232418,1.01632820259666));
#47631=CARTESIAN_POINT('Ctrl Pts',(1.88793646814106,0.388221893762555,0.636136973481322));
#47632=CARTESIAN_POINT('Ctrl Pts',(1.96553101732603,0.404034822633264,0.263580625276104));
#47633=CARTESIAN_POINT('',(1.97875730221509,0.333280447823553,0.263580625276104));
#47634=CARTESIAN_POINT('',(1.74290857880594,0.293107061381241,1.38914111564877));
#47635=CARTESIAN_POINT('Ctrl Pts',(1.97875730221509,0.333280447823553,0.263580625276103));
#47636=CARTESIAN_POINT('Ctrl Pts',(1.90076305042376,0.320007569431509,0.635789556457961));
#47637=CARTESIAN_POINT('Ctrl Pts',(1.82105162804574,0.306431570368061,1.01620172824913));
#47638=CARTESIAN_POINT('Ctrl Pts',(1.74290857880594,0.293107061381241,1.38914111564877));
#47639=CARTESIAN_POINT('',(1.74290857880594,-0.293107061381241,1.38914111564877));
#47640=CARTESIAN_POINT('Origin',(-0.0835792063422023,-4.44089209850063E-16,
1.00090915210539));
#47641=CARTESIAN_POINT('',(1.97875730221509,-0.333280447823553,0.263580625276104));
#47642=CARTESIAN_POINT('Ctrl Pts',(1.74290857880594,-0.293107061381241,
1.38914111564877));
#47643=CARTESIAN_POINT('Ctrl Pts',(1.82105162803739,-0.306431570366637,
1.01620172828898));
#47644=CARTESIAN_POINT('Ctrl Pts',(1.90076305041387,-0.320007569429825,
0.635789556505179));
#47645=CARTESIAN_POINT('Ctrl Pts',(1.97875730221509,-0.333280447823553,
0.263580625276104));
#47646=CARTESIAN_POINT('Origin',(-0.0948928998314158,-4.44089209850063E-16,
-0.177187331777248));
#47647=CARTESIAN_POINT('Origin',(0.,0.,0.833644253621703));
#47648=CARTESIAN_POINT('',(-1.83314153881416,-2.24495091789282E-16,1.46454945609501));
#47649=CARTESIAN_POINT('Origin',(0.,0.,1.46454945609501));
#47650=CARTESIAN_POINT('',(-2.10134761996907,-2.57340863669103E-16,0.202739051148399));
#47651=CARTESIAN_POINT('',(-1.96724457939162,-2.40917977729193E-16,0.833644253621703));
#47652=CARTESIAN_POINT('Origin',(0.,0.,0.202739051148399));
#47653=CARTESIAN_POINT('',(1.79536793495708,-1.0598953697797,0.280213560541524));
#47654=CARTESIAN_POINT('',(2.04083980696707,-0.426259426935219,0.280213560541524));
#47655=CARTESIAN_POINT('Origin',(-0.0919376867122903,0.0356168495811988,
-0.177974371324324));
#47656=CARTESIAN_POINT('',(1.58996439658141,-0.937219520893876,1.4057740509142));
#47657=CARTESIAN_POINT('Ctrl Pts',(1.79536793495708,-1.0598953697797,0.280213560541524));
#47658=CARTESIAN_POINT('Ctrl Pts',(1.72736598254189,-1.01929689490354,0.652811627092658));
#47659=CARTESIAN_POINT('Ctrl Pts',(1.65800091965806,-0.977871183631695,
1.03291010040004));
#47660=CARTESIAN_POINT('Ctrl Pts',(1.58996439658141,-0.937219520893876,
1.4057740509142));
#47661=CARTESIAN_POINT('',(1.80639857550374,-0.378538504196173,1.4057740509142));
#47662=CARTESIAN_POINT('Origin',(-0.0813879817216061,0.0315298720944248,
1.00012211255832));
#47663=CARTESIAN_POINT('Ctrl Pts',(1.80639857550374,-0.378538504196173,
1.4057740509142));
#47664=CARTESIAN_POINT('Ctrl Pts',(1.88406502083852,-0.394332472136845,
1.03291010044331));
#47665=CARTESIAN_POINT('Ctrl Pts',(1.96323474207058,-0.410449442790543,
0.652811627142982));
#47666=CARTESIAN_POINT('Ctrl Pts',(2.04083980696707,-0.426259426935219,
0.280213560541524));
#47667=CARTESIAN_POINT('',(1.29125237154726,-1.63688470263671,0.280213560541524));
#47668=CARTESIAN_POINT('',(1.74904377904568,-1.13471145042876,0.280213560541524));
#47669=CARTESIAN_POINT('Origin',(-0.0728630496078391,0.0664234462666804,
-0.177974371324323));
#47670=CARTESIAN_POINT('',(1.14403490424299,-1.44829256388851,1.4057740509142));
#47671=CARTESIAN_POINT('Ctrl Pts',(1.29125237154726,-1.63688470263671,0.280213560541524));
#47672=CARTESIAN_POINT('Ctrl Pts',(1.24247685283117,-1.57442234203435,0.653052008848893));
#47673=CARTESIAN_POINT('Ctrl Pts',(1.19277667894508,-1.51075710516702,1.03302725266647));
#47674=CARTESIAN_POINT('Ctrl Pts',(1.14403490424299,-1.44829256388851,1.4057740509142));
#47675=CARTESIAN_POINT('',(1.54767262692101,-1.00552307413627,1.4057740509142));
#47676=CARTESIAN_POINT('Origin',(-0.0645021292326089,0.0588014602494451,
1.00012211255832));
#47677=CARTESIAN_POINT('Ctrl Pts',(1.54767262692101,-1.00552307413627,1.4057740509142));
#47678=CARTESIAN_POINT('Ctrl Pts',(1.61436802906001,-1.04829342426708,1.03302725270948));
#47679=CARTESIAN_POINT('Ctrl Pts',(1.68234743475918,-1.09190729901199,0.653052008897806));
#47680=CARTESIAN_POINT('Ctrl Pts',(1.74904377904568,-1.13471145042876,0.280213560541524));
#47681=CARTESIAN_POINT('',(0.612746020283587,-1.99280368611139,0.280213560541524));
#47682=CARTESIAN_POINT('',(1.22102969697802,-1.68991440488869,0.280213560541524));
#47683=CARTESIAN_POINT('Origin',(-0.043947853905753,0.0882591884688249,
-0.177974371324323));
#47684=CARTESIAN_POINT('',(0.543597158770307,-1.76376567086387,1.4057740509142));
#47685=CARTESIAN_POINT('Ctrl Pts',(0.612746020283587,-1.99280368611139,
0.280213560541524));
#47686=CARTESIAN_POINT('Ctrl Pts',(0.589834870344302,-1.91696156463519,
0.652943668424222));
#47687=CARTESIAN_POINT('Ctrl Pts',(0.566485626831716,-1.83962933167279,
1.03297982842434));
#47688=CARTESIAN_POINT('Ctrl Pts',(0.543597158770307,-1.76376567086387,
1.4057740509142));
#47689=CARTESIAN_POINT('',(1.07992491412252,-1.49670618111856,1.4057740509142));
#47690=CARTESIAN_POINT('Origin',(-0.0389049067721117,0.0781315853676385,
1.00012211255832));
#47691=CARTESIAN_POINT('Ctrl Pts',(1.07992491412252,-1.49670618111856,1.4057740509142));
#47692=CARTESIAN_POINT('Ctrl Pts',(1.1266720387397,-1.56068964257619,1.03297982846752));
#47693=CARTESIAN_POINT('Ctrl Pts',(1.174313429993,-1.62592582323378,0.652943668473819));
#47694=CARTESIAN_POINT('Ctrl Pts',(1.22102969697802,-1.68991440488869,0.280213560541524));
#47695=CARTESIAN_POINT('',(-0.148515076362296,-2.07958348927029,0.280213560541524));
#47696=CARTESIAN_POINT('',(0.528108788374353,-2.01688505482942,0.280213560541524));
#47697=CARTESIAN_POINT('Origin',(-0.00909725701023012,0.0981750382072089,
-0.177974371324323));
#47698=CARTESIAN_POINT('',(-0.130256395170145,-1.84103245062609,1.4057740509142));
#47699=CARTESIAN_POINT('Ctrl Pts',(-0.148515076362296,-2.07958348927029,
0.280213560541524));
#47700=CARTESIAN_POINT('Ctrl Pts',(-0.14248860712088,-2.00067609817279,
0.652520236489613));
#47701=CARTESIAN_POINT('Ctrl Pts',(-0.136321810501501,-1.92008267222723,
1.03278544865149));
#47702=CARTESIAN_POINT('Ctrl Pts',(-0.130256395170145,-1.84103245062609,
1.4057740509142));
#47703=CARTESIAN_POINT('',(0.46632735760125,-1.78575082480554,1.4057740509142));
#47704=CARTESIAN_POINT('Origin',(-0.00805336107250954,0.0869096069398723,
1.00012211255832));
#47705=CARTESIAN_POINT('Ctrl Pts',(0.46632735760125,-1.78575082480554,1.4057740509142));
#47706=CARTESIAN_POINT('Ctrl Pts',(0.486814937810489,-1.86234054901206,
1.03278544869513));
#47707=CARTESIAN_POINT('Ctrl Pts',(0.507685736154786,-1.94042857282091,
0.652520236541599));
#47708=CARTESIAN_POINT('Ctrl Pts',(0.528108788374353,-2.01688505482942,
0.280213560541524));
#47709=CARTESIAN_POINT('',(-0.889718388995002,-1.88550401883333,0.280213560541524));
#47710=CARTESIAN_POINT('',(-0.236136138451081,-2.07146420216955,0.280213560541524));
#47711=CARTESIAN_POINT('Origin',(0.0269819748541655,0.0948318050290418,
-0.177974371324323));
#47712=CARTESIAN_POINT('',(-0.786518101167265,-1.66965759641828,1.4057740509142));
#47713=CARTESIAN_POINT('Ctrl Pts',(-0.889718388995002,-1.88550401883333,
0.280213560541524));
#47714=CARTESIAN_POINT('Ctrl Pts',(-0.855578399296262,-1.81406894201494,
0.65269302441041));
#47715=CARTESIAN_POINT('Ctrl Pts',(-0.820724037780499,-1.7411658402745,
1.03285226318453));
#47716=CARTESIAN_POINT('Ctrl Pts',(-0.786518101167265,-1.66965759641828,
1.4057740509142));
#47717=CARTESIAN_POINT('',(-0.210250292573155,-1.83361992441561,1.4057740509142));
#47718=CARTESIAN_POINT('Origin',(0.0238858356651481,0.0839500045121191,
1.00012211255832));
#47719=CARTESIAN_POINT('Ctrl Pts',(-0.210250292573155,-1.83361992441561,
1.4057740509142));
#47720=CARTESIAN_POINT('Ctrl Pts',(-0.218812058596698,-1.91242456387349,
1.0328522632279));
#47721=CARTESIAN_POINT('Ctrl Pts',(-0.227556820710594,-1.9927564871379,
0.652693024461391));
#47722=CARTESIAN_POINT('Ctrl Pts',(-0.236136138451081,-2.07146420216955,
0.280213560541524));
#47723=CARTESIAN_POINT('',(-1.51076030309415,-1.43677678271449,0.280213560541524));
#47724=CARTESIAN_POINT('',(-0.968489571303184,-1.84628063062728,0.280213560541524));
#47725=CARTESIAN_POINT('Origin',(0.0594171415022222,0.0786810111005316,
-0.177974371324324));
#47726=CARTESIAN_POINT('',(-1.3365561793545,-1.27278623192205,1.4057740509142));
#47727=CARTESIAN_POINT('Ctrl Pts',(-1.51076030309415,-1.43677678271449,
0.280213560541524));
#47728=CARTESIAN_POINT('Ctrl Pts',(-1.45306528620204,-1.38244645898933,
0.653049080203456));
#47729=CARTESIAN_POINT('Ctrl Pts',(-1.39425666924037,-1.3270833341075,1.03302896509998));
#47730=CARTESIAN_POINT('Ctrl Pts',(-1.3365561793545,-1.27278623192205,1.4057740509142));
#47731=CARTESIAN_POINT('',(-0.858432475698466,-1.63384849279461,1.4057740509142));
#47732=CARTESIAN_POINT('Origin',(0.0525991179402441,0.0696524887919709,
1.00012211255832));
#47733=CARTESIAN_POINT('Ctrl Pts',(-0.858432475698466,-1.63384849279461,
1.4057740509142));
#47734=CARTESIAN_POINT('Ctrl Pts',(-0.89486633233541,-1.70420541091867,
1.03302896514302));
#47735=CARTESIAN_POINT('Ctrl Pts',(-0.932022263572612,-1.77591988504572,
0.653049080252408));
#47736=CARTESIAN_POINT('Ctrl Pts',(-0.968489571303184,-1.84628063062728,
0.280213560541524));
#47737=CARTESIAN_POINT('',(-1.9277656668486,-0.794004880635056,0.280213560541524));
#47738=CARTESIAN_POINT('',(-1.57004312096482,-1.37174662932466,0.280213560541524));
#47739=CARTESIAN_POINT('Origin',(0.0838276939486571,0.0519039106363612,
-0.177974371324324));
#47740=CARTESIAN_POINT('',(-1.70608493940645,-0.704018034052772,1.4057740509142));
#47741=CARTESIAN_POINT('Ctrl Pts',(-1.9277656668486,-0.794004880635057,
0.280213560541524));
#47742=CARTESIAN_POINT('Ctrl Pts',(-1.85434143822608,-0.764185673242953,
0.653043245509423));
#47743=CARTESIAN_POINT('Ctrl Pts',(-1.77950274741209,-0.733804480193559,
1.03303237733945));
#47744=CARTESIAN_POINT('Ctrl Pts',(-1.70608493940644,-0.704018034052771,
1.4057740509142));
#47745=CARTESIAN_POINT('',(-1.39067859624214,-1.21341676875466,1.4057740509142));
#47746=CARTESIAN_POINT('Origin',(0.0742085978757352,0.045948018502703,1.00012211255832));
#47747=CARTESIAN_POINT('Ctrl Pts',(-1.39067859624214,-1.21341676875466,
1.4057740509142));
#47748=CARTESIAN_POINT('Ctrl Pts',(-1.45006746242559,-1.26586073387978,
1.03303237738257));
#47749=CARTESIAN_POINT('Ctrl Pts',(-1.51062206618193,-1.31931151963234,
0.653043245558453));
#47750=CARTESIAN_POINT('Ctrl Pts',(-1.57004312096482,-1.37174662932466,
0.280213560541524));
#47751=CARTESIAN_POINT('',(-2.08441559517683,-0.0439982196929346,0.280213560541524));
#47752=CARTESIAN_POINT('',(-1.95955364723089,-0.711950644621268,0.280213560541524));
#47753=CARTESIAN_POINT('Origin',(0.0969168518220385,0.0181168994312522,
-0.177974371324323));
#47754=CARTESIAN_POINT('',(-1.84519747464855,-0.040168299586067,1.4057740509142));
#47755=CARTESIAN_POINT('Ctrl Pts',(-2.08441559517683,-0.0439982196929347,
0.280213560541524));
#47756=CARTESIAN_POINT('Ctrl Pts',(-2.00527294760461,-0.0427180698377973,
0.652594621112284));
#47757=CARTESIAN_POINT('Ctrl Pts',(-1.92446479622355,-0.0414225081496093,
1.03281053473744));
#47758=CARTESIAN_POINT('Ctrl Pts',(-1.84519747464855,-0.040168299586067,
1.4057740509142));
#47759=CARTESIAN_POINT('',(-1.7351058663472,-0.629106386319966,1.4057740509142));
#47760=CARTESIAN_POINT('Origin',(0.0857957954640725,0.0160380137078846,
1.00012211255832));
#47761=CARTESIAN_POINT('Ctrl Pts',(-1.7351058663472,-0.629106386319966,
1.4057740509142));
#47762=CARTESIAN_POINT('Ctrl Pts',(-1.80947351479772,-0.656571530981326,
1.03281053478093));
#47763=CARTESIAN_POINT('Ctrl Pts',(-1.88529288273134,-0.684554726931419,
0.652594621163826));
#47764=CARTESIAN_POINT('Ctrl Pts',(-1.95955364723089,-0.711950644621269,
0.280213560541524));
#47765=CARTESIAN_POINT('',(-1.95955364723089,0.711950644621269,0.280213560541524));
#47766=CARTESIAN_POINT('',(-2.08441559517683,0.043998219692935,0.280213560541524));
#47767=CARTESIAN_POINT('Origin',(0.096916851822038,-0.0181168994312522,
-0.177974371324323));
#47768=CARTESIAN_POINT('',(-1.7351058663472,0.629106386319967,1.4057740509142));
#47769=CARTESIAN_POINT('Ctrl Pts',(-1.95955364723089,0.711950644621269,
0.280213560541524));
#47770=CARTESIAN_POINT('Ctrl Pts',(-1.88529288274162,0.684554726935211,
0.652594621112283));
#47771=CARTESIAN_POINT('Ctrl Pts',(-1.80947351480639,0.65657153098453,1.03281053473744));
#47772=CARTESIAN_POINT('Ctrl Pts',(-1.7351058663472,0.629106386319967,1.4057740509142));
#47773=CARTESIAN_POINT('',(-1.84519747464855,0.0401682995860675,1.4057740509142));
#47774=CARTESIAN_POINT('Origin',(0.0857957954640725,-0.0160380137078846,
1.00012211255832));
#47775=CARTESIAN_POINT('Ctrl Pts',(-1.84519747464855,0.0401682995860675,
1.4057740509142));
#47776=CARTESIAN_POINT('Ctrl Pts',(-1.92446479621431,0.0414225081494635,
1.03281053478093));
#47777=CARTESIAN_POINT('Ctrl Pts',(-2.00527294759366,0.0427180698376206,
0.652594621163825));
#47778=CARTESIAN_POINT('Ctrl Pts',(-2.08441559517683,0.0439982196929352,
0.280213560541524));
#47779=CARTESIAN_POINT('',(-1.57004312096482,1.37174662932466,0.280213560541524));
#47780=CARTESIAN_POINT('',(-1.9277656668486,0.794004880635056,0.280213560541524));
#47781=CARTESIAN_POINT('Origin',(0.0838276939486566,-0.0519039106363608,
-0.177974371324323));
#47782=CARTESIAN_POINT('',(-1.39067859624214,1.21341676875466,1.4057740509142));
#47783=CARTESIAN_POINT('Ctrl Pts',(-1.57004312096482,1.37174662932466,0.280213560541524));
#47784=CARTESIAN_POINT('Ctrl Pts',(-1.51062206618974,1.31931151963924,0.653043245509422));
#47785=CARTESIAN_POINT('Ctrl Pts',(-1.45006746243246,1.26586073388585,1.03303237733946));
#47786=CARTESIAN_POINT('Ctrl Pts',(-1.39067859624214,1.21341676875466,1.4057740509142));
#47787=CARTESIAN_POINT('',(-1.70608493940645,0.704018034052771,1.4057740509142));
#47788=CARTESIAN_POINT('Origin',(0.0742085978757352,-0.0459480185027024,
1.00012211255832));
#47789=CARTESIAN_POINT('Ctrl Pts',(-1.70608493940645,0.704018034052771,
1.4057740509142));
#47790=CARTESIAN_POINT('Ctrl Pts',(-1.7795027474036,0.733804480190114,1.03303237738257));
#47791=CARTESIAN_POINT('Ctrl Pts',(-1.85434143821642,0.764185673239031,
0.653043245558453));
#47792=CARTESIAN_POINT('Ctrl Pts',(-1.9277656668486,0.794004880635056,0.280213560541524));
#47793=CARTESIAN_POINT('',(-0.968489571303183,1.84628063062728,0.280213560541524));
#47794=CARTESIAN_POINT('',(-1.51076030309415,1.43677678271449,0.280213560541524));
#47795=CARTESIAN_POINT('Origin',(0.0594171415022222,-0.0786810111005312,
-0.177974371324323));
#47796=CARTESIAN_POINT('',(-0.858432475698465,1.63384849279461,1.4057740509142));
#47797=CARTESIAN_POINT('Ctrl Pts',(-0.968489571303183,1.84628063062729,
0.280213560541524));
#47798=CARTESIAN_POINT('Ctrl Pts',(-0.932022263577399,1.77591988505496,
0.653049080203456));
#47799=CARTESIAN_POINT('Ctrl Pts',(-0.894866332339616,1.7042054109268,1.03302896509998));
#47800=CARTESIAN_POINT('Ctrl Pts',(-0.858432475698465,1.63384849279461,
1.4057740509142));
#47801=CARTESIAN_POINT('',(-1.3365561793545,1.27278623192205,1.4057740509142));
#47802=CARTESIAN_POINT('Origin',(0.0525991179402439,-0.0696524887919705,
1.00012211255832));
#47803=CARTESIAN_POINT('Ctrl Pts',(-1.3365561793545,1.27278623192205,1.4057740509142));
#47804=CARTESIAN_POINT('Ctrl Pts',(-1.3942566692337,1.32708333410123,1.03302896514302));
#47805=CARTESIAN_POINT('Ctrl Pts',(-1.45306528619447,1.3824464589822,0.653049080252408));
#47806=CARTESIAN_POINT('Ctrl Pts',(-1.51076030309415,1.43677678271449,0.280213560541524));
#47807=CARTESIAN_POINT('',(-0.23613613845108,2.07146420216955,0.280213560541524));
#47808=CARTESIAN_POINT('',(-0.889718388995002,1.88550401883333,0.280213560541524));
#47809=CARTESIAN_POINT('Origin',(0.0269819748541655,-0.0948318050290409,
-0.177974371324323));
#47810=CARTESIAN_POINT('',(-0.210250292573154,1.83361992441561,1.4057740509142));
#47811=CARTESIAN_POINT('Ctrl Pts',(-0.236136138451081,2.07146420216955,
0.280213560541524));
#47812=CARTESIAN_POINT('Ctrl Pts',(-0.227556820711768,1.99275648714867,
0.65269302441041));
#47813=CARTESIAN_POINT('Ctrl Pts',(-0.218812058597693,1.91242456388265,
1.03285226318453));
#47814=CARTESIAN_POINT('Ctrl Pts',(-0.210250292573154,1.83361992441561,
1.4057740509142));
#47815=CARTESIAN_POINT('',(-0.786518101167265,1.66965759641828,1.4057740509142));
#47816=CARTESIAN_POINT('Origin',(0.0238858356651483,-0.0839500045121184,
1.00012211255832));
#47817=CARTESIAN_POINT('Ctrl Pts',(-0.786518101167265,1.66965759641828,
1.4057740509142));
#47818=CARTESIAN_POINT('Ctrl Pts',(-0.82072403777652,1.74116584026618,1.0328522632279));
#47819=CARTESIAN_POINT('Ctrl Pts',(-0.855578399291589,1.81406894200517,
0.652693024461392));
#47820=CARTESIAN_POINT('Ctrl Pts',(-0.889718388995002,1.88550401883333,
0.280213560541524));
#47821=CARTESIAN_POINT('',(0.528108788374354,2.01688505482942,0.280213560541524));
#47822=CARTESIAN_POINT('',(-0.148515076362295,2.07958348927029,0.280213560541524));
#47823=CARTESIAN_POINT('Origin',(-0.00909725701022968,-0.0981750382072075,
-0.177974371324323));
#47824=CARTESIAN_POINT('',(0.466327357601251,1.78575082480554,1.4057740509142));
#47825=CARTESIAN_POINT('Ctrl Pts',(0.528108788374354,2.01688505482942,0.280213560541524));
#47826=CARTESIAN_POINT('Ctrl Pts',(0.507685736157639,1.94042857283158,0.652520236489614));
#47827=CARTESIAN_POINT('Ctrl Pts',(0.486814937812886,1.86234054902102,1.03278544865149));
#47828=CARTESIAN_POINT('Ctrl Pts',(0.466327357601251,1.78575082480554,1.40577405091419));
#47829=CARTESIAN_POINT('',(-0.130256395170144,1.84103245062609,1.4057740509142));
#47830=CARTESIAN_POINT('Origin',(-0.00805336107250976,-0.0869096069398716,
1.00012211255832));
#47831=CARTESIAN_POINT('Ctrl Pts',(-0.130256395170144,1.84103245062609,
1.4057740509142));
#47832=CARTESIAN_POINT('Ctrl Pts',(-0.136321810500791,1.92008267221798,
1.03278544869513));
#47833=CARTESIAN_POINT('Ctrl Pts',(-0.142488607120037,2.00067609816177,
0.652520236541599));
#47834=CARTESIAN_POINT('Ctrl Pts',(-0.148515076362295,2.07958348927029,
0.280213560541524));
#47835=CARTESIAN_POINT('',(1.22102969697802,1.68991440488869,0.280213560541524));
#47836=CARTESIAN_POINT('',(0.612746020283587,1.99280368611139,0.280213560541524));
#47837=CARTESIAN_POINT('Origin',(-0.0439478539057538,-0.0882591884688253,
-0.177974371324324));
#47838=CARTESIAN_POINT('',(1.07992491412252,1.49670618111856,1.4057740509142));
#47839=CARTESIAN_POINT('Ctrl Pts',(1.22102969697802,1.68991440488869,0.280213560541524));
#47840=CARTESIAN_POINT('Ctrl Pts',(1.17431342999922,1.6259258232423,0.652943668424222));
#47841=CARTESIAN_POINT('Ctrl Pts',(1.12667203874511,1.5606896425836,1.03297982842434));
#47842=CARTESIAN_POINT('Ctrl Pts',(1.07992491412252,1.49670618111856,1.4057740509142));
#47843=CARTESIAN_POINT('',(0.543597158770306,1.76376567086387,1.4057740509142));
#47844=CARTESIAN_POINT('Origin',(-0.0389049067721121,-0.078131585367639,
1.00012211255832));
#47845=CARTESIAN_POINT('Ctrl Pts',(0.543597158770306,1.76376567086387,1.4057740509142));
#47846=CARTESIAN_POINT('Ctrl Pts',(0.566485626829063,1.839629331664,1.03297982846752));
#47847=CARTESIAN_POINT('Ctrl Pts',(0.589834870341253,1.9169615646251,0.652943668473819));
#47848=CARTESIAN_POINT('Ctrl Pts',(0.612746020283587,1.99280368611139,0.280213560541524));
#47849=CARTESIAN_POINT('',(1.74904377904567,1.13471145042876,0.280213560541524));
#47850=CARTESIAN_POINT('',(1.29125237154726,1.63688470263671,0.280213560541524));
#47851=CARTESIAN_POINT('Origin',(-0.0728630496078391,-0.0664234462666808,
-0.177974371324324));
#47852=CARTESIAN_POINT('',(1.54767262692101,1.00552307413627,1.4057740509142));
#47853=CARTESIAN_POINT('Ctrl Pts',(1.74904377904568,1.13471145042876,0.280213560541524));
#47854=CARTESIAN_POINT('Ctrl Pts',(1.68234743476795,1.09190729901762,0.653052008848806));
#47855=CARTESIAN_POINT('Ctrl Pts',(1.61436802906772,1.04829342427202,1.03302725266642));
#47856=CARTESIAN_POINT('Ctrl Pts',(1.54767262692101,1.00552307413627,1.4057740509142));
#47857=CARTESIAN_POINT('',(1.14403490424299,1.44829256388851,1.4057740509142));
#47858=CARTESIAN_POINT('Origin',(-0.0645021292326093,-0.0588014602494451,
1.00012211255832));
#47859=CARTESIAN_POINT('Ctrl Pts',(1.14403490424299,1.44829256388851,1.4057740509142));
#47860=CARTESIAN_POINT('Ctrl Pts',(1.19277667893946,1.51075710515983,1.03302725270942));
#47861=CARTESIAN_POINT('Ctrl Pts',(1.24247685282478,1.57442234202617,0.653052008897718));
#47862=CARTESIAN_POINT('Ctrl Pts',(1.29125237154726,1.63688470263671,0.280213560541524));
#47863=CARTESIAN_POINT('',(2.04083980696707,0.426259426935219,0.280213560541524));
#47864=CARTESIAN_POINT('',(1.79536793495708,1.0598953697797,0.280213560541524));
#47865=CARTESIAN_POINT('Origin',(-0.0919376867122907,-0.0356168495811993,
-0.177974371324324));
#47866=CARTESIAN_POINT('',(1.80639857550374,0.378538504196172,1.4057740509142));
#47867=CARTESIAN_POINT('Ctrl Pts',(2.04083980696707,0.426259426935219,0.280213560541524));
#47868=CARTESIAN_POINT('Ctrl Pts',(1.96323474208109,0.410449442792685,0.652811627092499));
#47869=CARTESIAN_POINT('Ctrl Pts',(1.88406502084756,0.394332472138682,1.03291010039994));
#47870=CARTESIAN_POINT('Ctrl Pts',(1.80639857550374,0.378538504196172,1.4057740509142));
#47871=CARTESIAN_POINT('',(1.58996439658141,0.937219520893876,1.4057740509142));
#47872=CARTESIAN_POINT('Origin',(-0.0813879817216063,-0.0315298720944253,
1.00012211255832));
#47873=CARTESIAN_POINT('Ctrl Pts',(1.58996439658141,0.937219520893876,1.4057740509142));
#47874=CARTESIAN_POINT('Ctrl Pts',(1.65800091965018,0.977871183626988,1.03291010044321));
#47875=CARTESIAN_POINT('Ctrl Pts',(1.72736598253273,1.01929689489808,0.652811627142823));
#47876=CARTESIAN_POINT('Ctrl Pts',(1.79536793495708,1.0598953697797,0.280213560541524));
#47877=CARTESIAN_POINT('',(1.82116038686464,0.299569788289876,1.4057740509142));
#47878=CARTESIAN_POINT('',(2.05700911027379,0.339761294150944,0.280213560541524));
#47879=CARTESIAN_POINT('Ctrl Pts',(1.82116038686464,0.299569788289876,1.4057740509142));
#47880=CARTESIAN_POINT('Ctrl Pts',(1.89931264504173,0.312902975680572,1.03279071366283));
#47881=CARTESIAN_POINT('Ctrl Pts',(1.97900261625265,0.326481279972747,0.652480914840093));
#47882=CARTESIAN_POINT('Ctrl Pts',(2.05700911027379,0.339761294150944,0.280213560541524));
#47883=CARTESIAN_POINT('',(2.05700911027379,-0.339761294150944,0.280213560541524));
#47884=CARTESIAN_POINT('Origin',(-0.0985956297819381,-4.44089209850063E-16,
-0.177974371324324));
#47885=CARTESIAN_POINT('',(1.82116038686464,-0.299569788289876,1.4057740509142));
#47886=CARTESIAN_POINT('Ctrl Pts',(2.05700911027379,-0.339761294150944,
0.280213560541524));
#47887=CARTESIAN_POINT('Ctrl Pts',(1.97900261626361,-0.326481279974613,
0.652480914787787));
#47888=CARTESIAN_POINT('Ctrl Pts',(1.89931264505091,-0.312902975682139,
1.03279071361899));
#47889=CARTESIAN_POINT('Ctrl Pts',(1.82116038686464,-0.299569788289876,
1.4057740509142));
#47890=CARTESIAN_POINT('Origin',(-0.0872819362927251,-2.22044604925031E-16,
1.00012211255832));
#47891=CARTESIAN_POINT('Origin',(0.,0.,0.194422583515688));
#47892=CARTESIAN_POINT('',(-2.06222171593972,-2.52549322355774E-16,0.194422583515688));
#47893=CARTESIAN_POINT('Origin',(0.,0.,1.4562329884623));
#47894=CARTESIAN_POINT('',(-1.79401563478481,-2.19703550475953E-16,1.4562329884623));
#47895=CARTESIAN_POINT('Origin',(1.68353271183615,-0.652204047184062,1.40243487042194));
#47896=CARTESIAN_POINT('Origin',(1.68353271183615,-0.652204047184062,1.40243487042194));
#47897=CARTESIAN_POINT('Origin',(1.68353271183615,-0.652204047184062,1.40243487042194));
#47898=CARTESIAN_POINT('',(1.42304436641037,-0.516927480140812,1.34041816052587));
#47899=CARTESIAN_POINT('Origin',(1.68353271183615,-0.652204047184062,1.40243487042194));
#47900=CARTESIAN_POINT('',(1.39989426782994,-0.576684772985975,1.34041816052587));
#47901=CARTESIAN_POINT('Origin',(-0.0549728800446225,0.0212966071870162,
1.0061434213025));
#47902=CARTESIAN_POINT('Origin',(1.68353271183615,-0.652204047184062,1.40243487042194));
#47903=CARTESIAN_POINT('Origin',(1.79500904160339,-0.69539020741027,0.84));
#47904=CARTESIAN_POINT('Origin',(1.90648537137062,-0.738576367636477,0.277565129578061));
#47905=CARTESIAN_POINT('Origin',(1.79500904160339,-0.69539020741027,0.84));
#47906=CARTESIAN_POINT('',(1.72523663201451,-0.45673394652411,0.22));
#47907=CARTESIAN_POINT('Origin',(1.90648537137062,-0.738576367636477,0.277565129578061));
#47908=CARTESIAN_POINT('',(1.60754702144021,-0.587633297864109,0.22));
#47909=CARTESIAN_POINT('Origin',(1.92030584968083,-0.743930449457738,0.22));
#47910=CARTESIAN_POINT('Ctrl Pts',(1.42304436641037,-0.516927480140814,
1.34041816052587));
#47911=CARTESIAN_POINT('Ctrl Pts',(1.48410498320936,-0.540267046545479,
0.969742401437925));
#47912=CARTESIAN_POINT('Ctrl Pts',(1.54648225040979,-0.564172784216683,
0.59094512501486));
#47913=CARTESIAN_POINT('Ctrl Pts',(1.60754702144021,-0.587633297864117,
0.22));
#47914=CARTESIAN_POINT('Origin',(2.21659783251117,-0.858714575118933,0.3482551044561));
#47915=CARTESIAN_POINT('Origin',(1.33424422438224,-1.21632432380853,1.40243487042194));
#47916=CARTESIAN_POINT('Origin',(1.33424422438224,-1.21632432380853,1.40243487042194));
#47917=CARTESIAN_POINT('Origin',(1.33424422438224,-1.21632432380853,1.40243487042194));
#47918=CARTESIAN_POINT('',(1.14021360866399,-0.996083437827601,1.34041816052587));
#47919=CARTESIAN_POINT('Origin',(1.33424422438224,-1.21632432380853,1.40243487042194));
#47920=CARTESIAN_POINT('',(1.09703996059555,-1.04344267372651,1.34041816052587));
#47921=CARTESIAN_POINT('Origin',(-0.0435674621476161,0.0397169895648517,
1.0061434213025));
#47922=CARTESIAN_POINT('Origin',(1.33424422438224,-1.21632432380853,1.40243487042194));
#47923=CARTESIAN_POINT('Origin',(1.42259216564977,-1.29686411401962,0.84));
#47924=CARTESIAN_POINT('Origin',(1.5109401069173,-1.37740390423071,0.277565129578061));
#47925=CARTESIAN_POINT('Origin',(1.42259216564977,-1.29686411401962,0.84));
#47926=CARTESIAN_POINT('',(1.44374391665803,-1.04911907687602,0.22));
#47927=CARTESIAN_POINT('Origin',(1.5109401069173,-1.37740390423071,0.277565129578061));
#47928=CARTESIAN_POINT('',(1.2867153233272,-1.12866469583084,0.22));
#47929=CARTESIAN_POINT('Origin',(1.52189320170064,-1.38738896945528,0.22));
#47930=CARTESIAN_POINT('Ctrl Pts',(1.14021360866399,-0.996083437827602,
1.34041816052587));
#47931=CARTESIAN_POINT('Ctrl Pts',(1.18866923103111,-1.03985896697717,0.970128186228657));
#47932=CARTESIAN_POINT('Ctrl Pts',(1.23815819319504,-1.08464692910743,0.591640399915973));
#47933=CARTESIAN_POINT('Ctrl Pts',(1.2867153233272,-1.12866469583084,0.22));
#47934=CARTESIAN_POINT('Origin',(1.75671243867939,-1.60145498856633,0.3482551044561));
#47935=CARTESIAN_POINT('Origin',(0.804758661123036,-1.61617326061691,1.40243487042194));
#47936=CARTESIAN_POINT('Origin',(0.804758661123036,-1.61617326061691,1.40243487042194));
#47937=CARTESIAN_POINT('Origin',(0.804758661123036,-1.61617326061691,1.40243487042194));
#47938=CARTESIAN_POINT('',(0.703390684925828,-1.3407128077469,1.34041816052587));
#47939=CARTESIAN_POINT('Origin',(0.804758661123036,-1.61617326061691,1.40243487042194));
#47940=CARTESIAN_POINT('',(0.646024327774458,-1.36927785946482,1.34041816052587));
#47941=CARTESIAN_POINT('Origin',(-0.0262780170719328,0.0527733724225172,
1.0061434213025));
#47942=CARTESIAN_POINT('Origin',(0.804758661123036,-1.61617326061691,1.40243487042194));
#47943=CARTESIAN_POINT('Origin',(0.858046334869837,-1.72318933585849,0.84));
#47944=CARTESIAN_POINT('Origin',(0.911334008616638,-1.83020541110008,0.277565129578061));
#47945=CARTESIAN_POINT('Origin',(0.858046334869837,-1.72318933585849,0.84));
#47946=CARTESIAN_POINT('',(0.967265585295667,-1.49981486252633,0.22));
#47947=CARTESIAN_POINT('Origin',(0.911334008616638,-1.83020541110008,0.277565129578061));
#47948=CARTESIAN_POINT('',(0.792105590863112,-1.51726367247863,0.22));
#47949=CARTESIAN_POINT('Origin',(0.917940443729429,-1.84347292134022,0.22));
#47950=CARTESIAN_POINT('Ctrl Pts',(0.703390684925826,-1.34071280774691,
1.34041816052587));
#47951=CARTESIAN_POINT('Ctrl Pts',(0.732784340667834,-1.39908348436706,
0.969829651658146));
#47952=CARTESIAN_POINT('Ctrl Pts',(0.762770120360982,-1.45876053753165,
0.591113455185774));
#47953=CARTESIAN_POINT('Ctrl Pts',(0.792105590863111,-1.51726367247863,
0.22));
#47954=CARTESIAN_POINT('Origin',(1.05957329572431,-2.12791003183941,0.3482551044561));
#47955=CARTESIAN_POINT('Origin',(0.166585981357483,-1.79774904305379,1.40243487042194));
#47956=CARTESIAN_POINT('Origin',(0.166585981357483,-1.79774904305379,1.40243487042194));
#47957=CARTESIAN_POINT('Origin',(0.166585981357483,-1.79774904305379,1.40243487042194));
#47958=CARTESIAN_POINT('',(0.171570951566094,-1.50427148383386,1.34041816052587));
#47959=CARTESIAN_POINT('Origin',(0.166585981357483,-1.79774904305379,1.40243487042194));
#47960=CARTESIAN_POINT('',(0.107759529743047,-1.51018448285187,1.34041816052587));
#47961=CARTESIAN_POINT('Origin',(-0.00543958017916557,0.0587024189071708,
1.0061434213025));
#47962=CARTESIAN_POINT('Origin',(0.166585981357483,-1.79774904305379,1.40243487042194));
#47963=CARTESIAN_POINT('Origin',(0.177616591966855,-1.91678828936794,0.84));
#47964=CARTESIAN_POINT('Origin',(0.188647202576228,-2.0358275356821,0.277565129578061));
#47965=CARTESIAN_POINT('Origin',(0.177616591966855,-1.91678828936794,0.84));
#47966=CARTESIAN_POINT('',(0.36015267683549,-1.74795234023142,0.22));
#47967=CARTESIAN_POINT('Origin',(0.188647202576228,-2.0358275356821,0.277565129578061));
#47968=CARTESIAN_POINT('',(0.190517609144359,-1.70094778270994,0.22));
#47969=CARTESIAN_POINT('Origin',(0.190014742348963,-2.05058564016207,0.22));
#47970=CARTESIAN_POINT('Ctrl Pts',(0.171570951566093,-1.50427148383386,
1.34041816052587));
#47971=CARTESIAN_POINT('Ctrl Pts',(0.177897879678585,-1.56936071475471,
0.969590466476621));
#47972=CARTESIAN_POINT('Ctrl Pts',(0.184305736125241,-1.63589092068322,
0.590584376399643));
#47973=CARTESIAN_POINT('Ctrl Pts',(0.190517609144358,-1.70094778270994,
0.22));
#47974=CARTESIAN_POINT('Origin',(0.219332907883337,-2.36697903415605,0.3482551044561));
#47975=CARTESIAN_POINT('Origin',(-0.494085058275185,-1.73652885555491,1.40243487042194));
#47976=CARTESIAN_POINT('Origin',(-0.494085058275185,-1.73652885555491,1.40243487042194));
#47977=CARTESIAN_POINT('Origin',(-0.494085058275185,-1.73652885555491,1.40243487042194));
#47978=CARTESIAN_POINT('',(-0.383420389510102,-1.46466996057301,1.34041816052587));
#47979=CARTESIAN_POINT('Origin',(-0.494085058275185,-1.73652885555491,1.40243487042194));
#47980=CARTESIAN_POINT('',(-0.445058789896328,-1.44713232360867,1.34041816052587));
#47981=CARTESIAN_POINT('Origin',(0.0161335021585525,0.0567033784370783,
1.0061434213025));
#47982=CARTESIAN_POINT('Origin',(-0.494085058275185,-1.73652885555491,1.40243487042194));
#47983=CARTESIAN_POINT('Origin',(-0.52680125588876,-1.85151436310768,0.84));
#47984=CARTESIAN_POINT('Origin',(-0.559517453502335,-1.96649987066044,0.277565129578061));
#47985=CARTESIAN_POINT('Origin',(-0.52680125588876,-1.85151436310768,0.84));
#47986=CARTESIAN_POINT('',(-0.295600846306194,-1.76001916864997,0.22));
#47987=CARTESIAN_POINT('Origin',(-0.559517453502335,-1.96649987066044,0.277565129578061));
#47988=CARTESIAN_POINT('',(-0.436800831383855,-1.65490946960924,0.22));
#47989=CARTESIAN_POINT('Origin',(-0.563573502893763,-1.98075540559274,0.22));
#47990=CARTESIAN_POINT('Ctrl Pts',(-0.383420389510103,-1.46466996057301,
1.34041816052587));
#47991=CARTESIAN_POINT('Ctrl Pts',(-0.401029817090961,-1.5276357164313,
0.96967110048816));
#47992=CARTESIAN_POINT('Ctrl Pts',(-0.419081848799302,-1.59196577132107,
0.590796412809183));
#47993=CARTESIAN_POINT('Ctrl Pts',(-0.436800831383856,-1.65490946960923,
0.22));
#47994=CARTESIAN_POINT('Origin',(-0.650529604532875,-2.28637440202631,0.3482551044561));
#47995=CARTESIAN_POINT('Origin',(-1.08802717296797,-1.44078082367478,1.40243487042194));
#47996=CARTESIAN_POINT('Origin',(-1.08802717296797,-1.44078082367478,1.40243487042194));
#47997=CARTESIAN_POINT('Origin',(-1.08802717296797,-1.44078082367478,1.40243487042194));
#47998=CARTESIAN_POINT('',(-0.886628682377235,-1.22725664312035,1.34041816052587));
#47999=CARTESIAN_POINT('Origin',(-1.08802717296797,-1.44078082367478,1.40243487042194));
#48000=CARTESIAN_POINT('',(-0.937769453804317,-1.18863692522509,1.34041816052587));
#48001=CARTESIAN_POINT('Origin',(0.0355276656309362,0.0470462325047916,
1.0061434213025));
#48002=CARTESIAN_POINT('Origin',(-1.08802717296797,-1.44078082367478,1.40243487042194));
#48003=CARTESIAN_POINT('Origin',(-1.16007167503007,-1.53618316251446,0.84));
#48004=CARTESIAN_POINT('Origin',(-1.23211617709217,-1.63158550135414,0.277565129578061));
#48005=CARTESIAN_POINT('Origin',(-1.16007167503007,-1.53618316251446,0.84));
#48006=CARTESIAN_POINT('',(-0.911431837173392,-1.53438565573945,0.22));
#48007=CARTESIAN_POINT('Origin',(-1.23211617709217,-1.63158550135414,0.277565129578061));
#48008=CARTESIAN_POINT('',(-1.00512689923672,-1.38536646246786,0.22));
#48009=CARTESIAN_POINT('Origin',(-1.2410480237021,-1.64341317775352,0.22));
#48010=CARTESIAN_POINT('Ctrl Pts',(-0.886628682377236,-1.22725664312035,
1.34041816052587));
#48011=CARTESIAN_POINT('Ctrl Pts',(-0.92575705730228,-1.27955870074339,
0.970028743491965));
#48012=CARTESIAN_POINT('Ctrl Pts',(-0.965795109999248,-1.33297888801976,
0.591471165657163));
#48013=CARTESIAN_POINT('Ctrl Pts',(-1.00512689923672,-1.38536646246787,
0.22));
#48014=CARTESIAN_POINT('Origin',(-1.43253448914795,-1.896982237665,0.3482551044561));
#48015=CARTESIAN_POINT('Origin',(-1.53502518898474,-0.950447357915218,1.40243487042194));
#48016=CARTESIAN_POINT('Origin',(-1.53502518898474,-0.950447357915218,1.40243487042194));
#48017=CARTESIAN_POINT('Origin',(-1.53502518898474,-0.950447357915218,1.40243487042194));
#48018=CARTESIAN_POINT('',(-1.27009285871019,-0.824095515550463,1.34041816052587));
#48019=CARTESIAN_POINT('Origin',(-1.53502518898474,-0.950447357915218,1.40243487042194));
#48020=CARTESIAN_POINT('',(-1.3038291566161,-0.769609523625294,1.34041816052587));
#48021=CARTESIAN_POINT('Origin',(0.0501236209942708,0.0310352321805594,
1.0061434213025));
#48022=CARTESIAN_POINT('Origin',(-1.53502518898474,-0.950447357915218,1.40243487042194));
#48023=CARTESIAN_POINT('Origin',(-1.63666798627951,-1.01338191353891,0.84));
#48024=CARTESIAN_POINT('Origin',(-1.73831078357428,-1.0763164691626,0.277565129578061));
#48025=CARTESIAN_POINT('Origin',(-1.63666798627951,-1.01338191353891,0.84));
#48026=CARTESIAN_POINT('',(-1.40416890801217,-1.1015248576969,0.22));
#48027=CARTESIAN_POINT('Origin',(-1.73831078357428,-1.0763164691626,0.277565129578061));
#48028=CARTESIAN_POINT('',(-1.43770500974724,-0.928722037989642,0.22));
#48029=CARTESIAN_POINT('Origin',(-1.75091213202498,-1.0841188937919,0.22));
#48030=CARTESIAN_POINT('Ctrl Pts',(-1.27009285871019,-0.824095515550462,
1.34041816052587));
#48031=CARTESIAN_POINT('Ctrl Pts',(-1.32548789695821,-0.85874045931348,
0.969926863920483));
#48032=CARTESIAN_POINT('Ctrl Pts',(-1.38213150089445,-0.894097100162996,
0.591291664620299));
#48033=CARTESIAN_POINT('Ctrl Pts',(-1.43770500974724,-0.928722037989639,
0.22));
#48034=CARTESIAN_POINT('Origin',(-2.02106765305595,-1.25139211056558,0.3482551044561));
#48035=CARTESIAN_POINT('Origin',(-1.77470954736091,-0.331750709858588,1.40243487042194));
#48036=CARTESIAN_POINT('Origin',(-1.77470954736091,-0.331750709858588,1.40243487042194));
#48037=CARTESIAN_POINT('Origin',(-1.77470954736091,-0.331750709858588,1.40243487042194));
#48038=CARTESIAN_POINT('',(-1.48202395664685,-0.309635722134599,1.34041816052587));
#48039=CARTESIAN_POINT('Origin',(-1.77470954736091,-0.331750709858588,1.40243487042194));
#48040=CARTESIAN_POINT('',(-1.49379950706012,-0.246642091306309,1.34041816052587));
#48041=CARTESIAN_POINT('Origin',(0.0579501035977568,0.0108327517781841,
1.0061434213025));
#48042=CARTESIAN_POINT('Origin',(-1.77470954736091,-0.331750709858588,1.40243487042194));
#48043=CARTESIAN_POINT('Origin',(-1.89222321689151,-0.353717821796897,0.84));
#48044=CARTESIAN_POINT('Origin',(-2.00973688642211,-0.375684933735207,0.277565129578061));
#48045=CARTESIAN_POINT('Origin',(-1.89222321689151,-0.353717821796897,0.84));
#48046=CARTESIAN_POINT('',(-1.70726518705538,-0.519897023862431,0.22));
#48047=CARTESIAN_POINT('Origin',(-2.00973688642211,-0.375684933735207,0.277565129578061));
#48048=CARTESIAN_POINT('',(-1.67611309209292,-0.346648556054458,0.22));
#48049=CARTESIAN_POINT('Origin',(-2.02430585477882,-0.378408345913518,0.22));
#48050=CARTESIAN_POINT('Ctrl Pts',(-1.48202395664686,-0.309635722134596,
1.34041816052587));
#48051=CARTESIAN_POINT('Ctrl Pts',(-1.54624662587943,-0.32194035490071,
0.96962006919933));
#48052=CARTESIAN_POINT('Ctrl Pts',(-1.61189130995875,-0.334457530455581,
0.59067441941184));
#48053=CARTESIAN_POINT('Ctrl Pts',(-1.67611309209293,-0.346648556054445,
0.22));
#48054=CARTESIAN_POINT('Origin',(-2.33664443129628,-0.43679454473122,0.3482551044561));
#48055=CARTESIAN_POINT('Origin',(-1.77470954736091,0.331750709858588,1.40243487042194));
#48056=CARTESIAN_POINT('Origin',(-1.77470954736091,0.331750709858588,1.40243487042194));
#48057=CARTESIAN_POINT('Origin',(-1.77470954736091,0.331750709858588,1.40243487042194));
#48058=CARTESIAN_POINT('',(-1.49379950706012,0.24664209130631,1.34041816052587));
#48059=CARTESIAN_POINT('Origin',(-1.77470954736091,0.331750709858588,1.40243487042194));
#48060=CARTESIAN_POINT('',(-1.48202395664685,0.309635722134599,1.34041816052587));
#48061=CARTESIAN_POINT('Origin',(0.0579501035977565,-0.0108327517781845,
1.0061434213025));
#48062=CARTESIAN_POINT('Origin',(-1.77470954736091,0.331750709858588,1.40243487042194));
#48063=CARTESIAN_POINT('Origin',(-1.89222321689151,0.353717821796898,0.84));
#48064=CARTESIAN_POINT('Origin',(-2.00973688642211,0.375684933735208,0.277565129578061));
#48065=CARTESIAN_POINT('Origin',(-1.89222321689151,0.353717821796898,0.84));
#48066=CARTESIAN_POINT('',(-1.77978584230378,0.131945783893516,0.22));
#48067=CARTESIAN_POINT('Origin',(-2.00973688642211,0.375684933735208,0.277565129578061));
#48068=CARTESIAN_POINT('',(-1.6881528136882,0.282241734221853,0.22));
#48069=CARTESIAN_POINT('Origin',(-2.02430585477882,0.378408345913518,0.22));
#48070=CARTESIAN_POINT('Ctrl Pts',(-1.49379950706012,0.246642091306312,
1.34041816052587));
#48071=CARTESIAN_POINT('Ctrl Pts',(-1.55813030865998,0.258368266999456,
0.96962006919933));
#48072=CARTESIAN_POINT('Ctrl Pts',(-1.62386387892535,0.270409943457099,
0.59067441941184));
#48073=CARTESIAN_POINT('Ctrl Pts',(-1.6881528136882,0.282241734221861,0.22));
#48074=CARTESIAN_POINT('Origin',(-2.33664443129628,0.43679454473122,0.3482551044561));
#48075=CARTESIAN_POINT('Origin',(-1.53502518898474,0.950447357915218,1.40243487042194));
#48076=CARTESIAN_POINT('Origin',(-1.53502518898474,0.950447357915218,1.40243487042194));
#48077=CARTESIAN_POINT('Origin',(-1.53502518898474,0.950447357915218,1.40243487042194));
#48078=CARTESIAN_POINT('',(-1.3038291566161,0.769609523625295,1.34041816052587));
#48079=CARTESIAN_POINT('Origin',(-1.53502518898474,0.950447357915218,1.40243487042194));
#48080=CARTESIAN_POINT('',(-1.27009285871019,0.824095515550462,1.34041816052587));
#48081=CARTESIAN_POINT('Origin',(0.0501236209942704,-0.0310352321805596,
1.0061434213025));
#48082=CARTESIAN_POINT('Origin',(-1.53502518898474,0.950447357915218,1.40243487042194));
#48083=CARTESIAN_POINT('Origin',(-1.63666798627951,1.01338191353891,0.84));
#48084=CARTESIAN_POINT('Origin',(-1.73831078357428,1.0763164691626,0.277565129578061));
#48085=CARTESIAN_POINT('Origin',(-1.63666798627951,1.01338191353891,0.84));
#48086=CARTESIAN_POINT('',(-1.61193655741525,0.765968582397815,0.22));
#48087=CARTESIAN_POINT('Origin',(-1.73831078357428,1.0763164691626,0.277565129578061));
#48088=CARTESIAN_POINT('',(-1.47219814341721,0.873013714336073,0.22));
#48089=CARTESIAN_POINT('Origin',(-1.75091213202497,1.0841188937919,0.22));
#48090=CARTESIAN_POINT('Ctrl Pts',(-1.3038291566161,0.769609523625296,1.34041816052587));
#48091=CARTESIAN_POINT('Ctrl Pts',(-1.35953373177067,0.803754548119228,
0.969926863920484));
#48092=CARTESIAN_POINT('Ctrl Pts',(-1.41643192564858,0.838700012094964,
0.591291664620299));
#48093=CARTESIAN_POINT('Ctrl Pts',(-1.47219814341721,0.873013714336066,
0.22));
#48094=CARTESIAN_POINT('Origin',(-2.02106765305595,1.25139211056558,0.3482551044561));
#48095=CARTESIAN_POINT('Origin',(-1.08802717296797,1.44078082367478,1.40243487042194));
#48096=CARTESIAN_POINT('Origin',(-1.08802717296797,1.44078082367478,1.40243487042194));
#48097=CARTESIAN_POINT('Origin',(-1.08802717296797,1.44078082367478,1.40243487042194));
#48098=CARTESIAN_POINT('',(-0.937769453804316,1.1886369252251,1.34041816052587));
#48099=CARTESIAN_POINT('Origin',(-1.08802717296797,1.44078082367478,1.40243487042194));
#48100=CARTESIAN_POINT('',(-0.886628682377236,1.22725664312035,1.34041816052587));
#48101=CARTESIAN_POINT('Origin',(0.0355276656309362,-0.0470462325047913,
1.0061434213025));
#48102=CARTESIAN_POINT('Origin',(-1.08802717296797,1.44078082367478,1.40243487042194));
#48103=CARTESIAN_POINT('Origin',(-1.16007167503007,1.53618316251446,0.84));
#48104=CARTESIAN_POINT('Origin',(-1.23211617709217,1.63158550135414,0.277565129578061));
#48105=CARTESIAN_POINT('Origin',(-1.16007167503007,1.53618316251446,0.84));
#48106=CARTESIAN_POINT('',(-1.22638630839898,1.29654307947085,0.22));
#48107=CARTESIAN_POINT('Origin',(-1.23211617709217,1.63158550135414,0.277565129578061));
#48108=CARTESIAN_POINT('',(-1.0574149561462,1.3458803547932,0.22));
#48109=CARTESIAN_POINT('Origin',(-1.2410480237021,1.64341317775352,0.22));
#48110=CARTESIAN_POINT('Ctrl Pts',(-0.937769453804315,1.1886369252251,1.34041816052587));
#48111=CARTESIAN_POINT('Ctrl Pts',(-0.977366925938209,1.24058473707973,
0.970028743491965));
#48112=CARTESIAN_POINT('Ctrl Pts',(-1.01779089870601,1.29371349104664,0.591471165657163));
#48113=CARTESIAN_POINT('Ctrl Pts',(-1.05741495614621,1.3458803547932,0.22));
#48114=CARTESIAN_POINT('Origin',(-1.43253448914794,1.896982237665,0.3482551044561));
#48115=CARTESIAN_POINT('Origin',(-0.494085058275185,1.73652885555491,1.40243487042194));
#48116=CARTESIAN_POINT('Origin',(-0.494085058275185,1.73652885555491,1.40243487042194));
#48117=CARTESIAN_POINT('Origin',(-0.494085058275185,1.73652885555491,1.40243487042194));
#48118=CARTESIAN_POINT('',(-0.445058789896327,1.44713232360867,1.34041816052587));
#48119=CARTESIAN_POINT('Origin',(-0.494085058275185,1.73652885555491,1.40243487042194));
#48120=CARTESIAN_POINT('',(-0.383420389510103,1.46466996057301,1.34041816052587));
#48121=CARTESIAN_POINT('Origin',(0.0161335021585525,-0.0567033784370781,
1.0061434213025));
#48122=CARTESIAN_POINT('Origin',(-0.494085058275185,1.73652885555491,1.40243487042194));
#48123=CARTESIAN_POINT('Origin',(-0.52680125588876,1.85151436310768,0.84));
#48124=CARTESIAN_POINT('Origin',(-0.559517453502335,1.96649987066044,0.277565129578062));
#48125=CARTESIAN_POINT('Origin',(-0.52680125588876,1.85151436310768,0.84));
#48126=CARTESIAN_POINT('',(-0.675205792792306,1.65201224926814,0.22));
#48127=CARTESIAN_POINT('Origin',(-0.559517453502335,1.96649987066044,0.277565129578062));
#48128=CARTESIAN_POINT('',(-0.499822019709113,1.63697839555501,0.22));
#48129=CARTESIAN_POINT('Origin',(-0.563573502893763,1.98075540559275,0.22));
#48130=CARTESIAN_POINT('Ctrl Pts',(-0.445058789896326,1.44713232360867,
1.34041816052587));
#48131=CARTESIAN_POINT('Ctrl Pts',(-0.463234151860379,1.50993705725198,
0.969671100488159));
#48132=CARTESIAN_POINT('Ctrl Pts',(-0.481751415100855,1.57413474235824,
0.590796412809184));
#48133=CARTESIAN_POINT('Ctrl Pts',(-0.499822019709111,1.63697839555501,
0.22));
#48134=CARTESIAN_POINT('Origin',(-0.650529604532875,2.28637440202631,0.3482551044561));
#48135=CARTESIAN_POINT('Origin',(0.166585981357484,1.79774904305379,1.40243487042194));
#48136=CARTESIAN_POINT('Origin',(0.166585981357484,1.79774904305379,1.40243487042194));
#48137=CARTESIAN_POINT('Origin',(0.166585981357484,1.79774904305379,1.40243487042194));
#48138=CARTESIAN_POINT('',(0.107759529743047,1.51018448285187,1.34041816052587));
#48139=CARTESIAN_POINT('Origin',(0.166585981357484,1.79774904305379,1.40243487042194));
#48140=CARTESIAN_POINT('',(0.171570951566095,1.50427148383386,1.34041816052587));
#48141=CARTESIAN_POINT('Origin',(-0.00543958017916535,-0.0587024189071703,
1.0061434213025));
#48142=CARTESIAN_POINT('Origin',(0.166585981357484,1.79774904305379,1.40243487042194));
#48143=CARTESIAN_POINT('Origin',(0.177616591966856,1.91678828936794,0.84));
#48144=CARTESIAN_POINT('Origin',(0.188647202576229,2.0358275356821,0.277565129578061));
#48145=CARTESIAN_POINT('Origin',(0.177616591966856,1.91678828936794,0.84));
#48146=CARTESIAN_POINT('',(-0.0328349934245687,1.78436801068587,0.22));
#48147=CARTESIAN_POINT('Origin',(0.188647202576229,2.0358275356821,0.277565129578061));
#48148=CARTESIAN_POINT('',(0.12527465009912,1.70699343318669,0.22));
#48149=CARTESIAN_POINT('Origin',(0.190014742348964,2.05058564016207,0.22));
#48150=CARTESIAN_POINT('Ctrl Pts',(0.107759529743049,1.51018448285187,1.34041816052587));
#48151=CARTESIAN_POINT('Ctrl Pts',(0.113500444401593,1.57532801591611,0.96959046647662));
#48152=CARTESIAN_POINT('Ctrl Pts',(0.119426587147494,1.64190285919258,0.590584376399643));
#48153=CARTESIAN_POINT('Ctrl Pts',(0.12527465009912,1.70699343318669,0.22));
#48154=CARTESIAN_POINT('Origin',(0.219332907883338,2.36697903415605,0.3482551044561));
#48155=CARTESIAN_POINT('Origin',(0.804758661123035,1.61617326061691,1.40243487042194));
#48156=CARTESIAN_POINT('Origin',(0.804758661123035,1.61617326061691,1.40243487042194));
#48157=CARTESIAN_POINT('Origin',(0.804758661123035,1.61617326061691,1.40243487042194));
#48158=CARTESIAN_POINT('',(0.646024327774458,1.36927785946482,1.34041816052587));
#48159=CARTESIAN_POINT('Origin',(0.804758661123035,1.61617326061691,1.40243487042194));
#48160=CARTESIAN_POINT('',(0.703390684925827,1.3407128077469,1.34041816052587));
#48161=CARTESIAN_POINT('Origin',(-0.0262780170719323,-0.052773372422517,
1.0061434213025));
#48162=CARTESIAN_POINT('Origin',(0.804758661123035,1.61617326061691,1.40243487042194));
#48163=CARTESIAN_POINT('Origin',(0.858046334869836,1.7231893358585,0.84));
#48164=CARTESIAN_POINT('Origin',(0.911334008616637,1.83020541110008,0.277565129578061));
#48165=CARTESIAN_POINT('Origin',(0.858046334869836,1.7231893358585,0.84));
#48166=CARTESIAN_POINT('',(0.613970353750136,1.67573498473601,0.22));
#48167=CARTESIAN_POINT('Origin',(0.911334008616637,1.83020541110008,0.277565129578061));
#48168=CARTESIAN_POINT('',(0.733452284240665,1.54646954888937,0.22));
#48169=CARTESIAN_POINT('Origin',(0.917940443729428,1.84347292134022,0.22));
#48170=CARTESIAN_POINT('Ctrl Pts',(0.64602432777446,1.36927785946482,1.34041816052587));
#48171=CARTESIAN_POINT('Ctrl Pts',(0.674891498245406,1.42791069459989,0.969829651658146));
#48172=CARTESIAN_POINT('Ctrl Pts',(0.704444345302139,1.48780332260248,0.591113455185774));
#48173=CARTESIAN_POINT('Ctrl Pts',(0.733452284240667,1.54646954888937,0.22));
#48174=CARTESIAN_POINT('Origin',(1.05957329572431,2.12791003183941,0.3482551044561));
#48175=CARTESIAN_POINT('Origin',(1.33424422438224,1.21632432380853,1.40243487042194));
#48176=CARTESIAN_POINT('Origin',(1.33424422438224,1.21632432380853,1.40243487042194));
#48177=CARTESIAN_POINT('Origin',(1.33424422438224,1.21632432380853,1.40243487042194));
#48178=CARTESIAN_POINT('',(1.09703996059555,1.04344267372651,1.34041816052587));
#48179=CARTESIAN_POINT('Origin',(1.33424422438224,1.21632432380853,1.40243487042194));
#48180=CARTESIAN_POINT('',(1.14021360866399,0.996083437827603,1.34041816052587));
#48181=CARTESIAN_POINT('Origin',(-0.0435674621476159,-0.0397169895648515,
1.0061434213025));
#48182=CARTESIAN_POINT('Origin',(1.33424422438224,1.21632432380853,1.40243487042194));
#48183=CARTESIAN_POINT('Origin',(1.42259216564977,1.29686411401962,0.84));
#48184=CARTESIAN_POINT('Origin',(1.5109401069173,1.37740390423071,0.277565129578062));
#48185=CARTESIAN_POINT('Origin',(1.42259216564977,1.29686411401962,0.84));
#48186=CARTESIAN_POINT('',(1.17785560252371,1.34078466352944,0.22));
#48187=CARTESIAN_POINT('Origin',(1.5109401069173,1.37740390423071,0.277565129578062));
#48188=CARTESIAN_POINT('',(1.2425731231961,1.17708638273095,0.22));
#48189=CARTESIAN_POINT('Origin',(1.52189320170064,1.38738896945528,0.22));
#48190=CARTESIAN_POINT('Ctrl Pts',(1.09703996059555,1.04344267372651,1.34041816052587));
#48191=CARTESIAN_POINT('Ctrl Pts',(1.14509967248684,1.08765249728891,0.970128181227685));
#48192=CARTESIAN_POINT('Ctrl Pts',(1.194262842832,1.1327978368539,0.591640391729911));
#48193=CARTESIAN_POINT('Ctrl Pts',(1.2425731231961,1.17708638273095,0.22));
#48194=CARTESIAN_POINT('Origin',(1.75671243867939,1.60145498856633,0.3482551044561));
#48195=CARTESIAN_POINT('Origin',(1.68353271183615,0.652204047184062,1.40243487042194));
#48196=CARTESIAN_POINT('Origin',(1.68353271183615,0.652204047184062,1.40243487042194));
#48197=CARTESIAN_POINT('Origin',(1.68353271183615,0.652204047184062,1.40243487042194));
#48198=CARTESIAN_POINT('',(1.39989426782994,0.576684772985975,1.34041816052587));
#48199=CARTESIAN_POINT('Origin',(1.68353271183615,0.652204047184062,1.40243487042194));
#48200=CARTESIAN_POINT('',(1.42304436641037,0.516927480140812,1.34041816052587));
#48201=CARTESIAN_POINT('Origin',(-0.0549728800446225,-0.0212966071870164,
1.0061434213025));
#48202=CARTESIAN_POINT('Origin',(1.68353271183615,0.652204047184062,1.40243487042194));
#48203=CARTESIAN_POINT('Origin',(1.79500904160339,0.695390207410269,0.84));
#48204=CARTESIAN_POINT('Origin',(1.90648537137062,0.738576367636477,0.277565129578061));
#48205=CARTESIAN_POINT('Origin',(1.79500904160339,0.695390207410269,0.84));
#48206=CARTESIAN_POINT('',(1.58266492545325,0.824753943968932,0.22));
#48207=CARTESIAN_POINT('Origin',(1.90648537137062,0.738576367636477,0.277565129578061));
#48208=CARTESIAN_POINT('',(1.58387757652854,0.648731178123911,0.22));
#48209=CARTESIAN_POINT('Origin',(1.92030584968083,0.743930449457738,0.22));
#48210=CARTESIAN_POINT('Ctrl Pts',(1.39989426782994,0.576684772985972,1.34041816052587));
#48211=CARTESIAN_POINT('Ctrl Pts',(1.46074237398106,0.6005728974663,0.969742391482374));
#48212=CARTESIAN_POINT('Ctrl Pts',(1.52294492302307,0.624929637725966,0.590945108845491));
#48213=CARTESIAN_POINT('Ctrl Pts',(1.58387757652854,0.648731178123902,0.22));
#48214=CARTESIAN_POINT('Origin',(2.21659783251117,0.858714575118932,0.3482551044561));
#48215=CARTESIAN_POINT('Origin',(2.37711940646971,0.,0.3482551044561));
#48216=CARTESIAN_POINT('Origin',(2.04454922222021,0.,0.277565129578061));
#48217=CARTESIAN_POINT('Origin',(1.80545077777979,0.,1.40243487042194));
#48218=CARTESIAN_POINT('Origin',(1.80545077777979,0.,1.40243487042194));
#48219=CARTESIAN_POINT('Origin',(1.80545077777979,0.,1.40243487042194));
#48220=CARTESIAN_POINT('',(1.51368509711198,0.0320423981330441,1.34041816052587));
#48221=CARTESIAN_POINT('Origin',(1.80545077777979,0.,1.40243487042194));
#48222=CARTESIAN_POINT('',(1.51368509711198,-0.0320423981330441,1.34041816052587));
#48223=CARTESIAN_POINT('Origin',(-0.058953905876358,2.22044604925031E-16,
1.0061434213025));
#48224=CARTESIAN_POINT('Origin',(1.80545077777979,0.,1.40243487042194));
#48225=CARTESIAN_POINT('Origin',(1.925,0.,0.84));
#48226=CARTESIAN_POINT('Origin',(1.925,0.,0.84));
#48227=CARTESIAN_POINT('',(1.77372658035123,0.197335634156047,0.22));
#48228=CARTESIAN_POINT('Origin',(2.04454922222021,0.,0.277565129578061));
#48229=CARTESIAN_POINT('',(1.71127058658217,0.0327612331676529,0.22));
#48230=CARTESIAN_POINT('Origin',(2.05937055187959,5.55111512312578E-17,
0.22));
#48231=CARTESIAN_POINT('Ctrl Pts',(1.51368509711198,0.0320423981330421,
1.34041816052587));
#48232=CARTESIAN_POINT('Ctrl Pts',(1.57907985889494,0.032336657496431,0.969593785059623));
#48233=CARTESIAN_POINT('Ctrl Pts',(1.64592664765089,0.0325785727668236,
0.590535829016318));
#48234=CARTESIAN_POINT('Ctrl Pts',(1.71127058658217,0.0327612331676708,
0.22));
#48235=CARTESIAN_POINT('Origin',(2.21659783251117,-0.858714575118933,0.3482551044561));
#48236=CARTESIAN_POINT('',(1.58266492545325,-0.824753943968933,0.22));
#48237=CARTESIAN_POINT('Origin',(1.90648537137062,-0.738576367636477,0.277565129578061));
#48238=CARTESIAN_POINT('',(1.76562782918999,-0.352472248043786,0.22));
#48239=CARTESIAN_POINT('Origin',(1.79500904160339,-0.69539020741027,0.84));
#48240=CARTESIAN_POINT('',(1.58387757652854,-0.648731178123907,0.22));
#48241=CARTESIAN_POINT('Ctrl Pts',(1.58387757652854,-0.648731178123902,
0.22));
#48242=CARTESIAN_POINT('Ctrl Pts',(1.52294492060034,-0.624929636779598,
0.590945123594562));
#48243=CARTESIAN_POINT('Ctrl Pts',(1.46074237258046,-0.600572896916442,
0.969742400014606));
#48244=CARTESIAN_POINT('Ctrl Pts',(1.39989426782994,-0.576684772985972,
1.34041816052587));
#48245=CARTESIAN_POINT('Origin',(1.92030584968083,-0.743930449457738,0.22));
#48246=CARTESIAN_POINT('Origin',(0.,0.,0.79));
#48247=CARTESIAN_POINT('',(-1.5105713967741,-1.84991642594294E-16,1.36));
#48248=CARTESIAN_POINT('Origin',(0.,0.,1.36));
#48249=CARTESIAN_POINT('',(-1.71158415478175,-2.09608605662479E-16,0.22));
#48250=CARTESIAN_POINT('',(-1.61107777577792,-1.97300124128387E-16,0.79));
#48251=CARTESIAN_POINT('',(-1.6881528136882,-0.282241734221848,0.22));
#48252=CARTESIAN_POINT('Origin',(0.,0.,0.22));
#48253=CARTESIAN_POINT('Ctrl Pts',(-1.6881528136882,-0.282241734221859,
0.22));
#48254=CARTESIAN_POINT('Ctrl Pts',(-1.62386387917194,-0.27040994350248,
0.590674417990065));
#48255=CARTESIAN_POINT('Ctrl Pts',(-1.55813030890113,-0.258368267043411,
0.969620067809347));
#48256=CARTESIAN_POINT('Ctrl Pts',(-1.49379950706012,-0.246642091306311,
1.34041816052587));
#48257=CARTESIAN_POINT('',(-1.47219814341721,-0.873013714336066,0.22));
#48258=CARTESIAN_POINT('Origin',(0.,0.,0.22));
#48259=CARTESIAN_POINT('Ctrl Pts',(-1.47219814341721,-0.873013714336065,
0.22));
#48260=CARTESIAN_POINT('Ctrl Pts',(-1.41643192586061,-0.838700012225428,
0.591291663208605));
#48261=CARTESIAN_POINT('Ctrl Pts',(-1.35953373199102,-0.803754548254296,
0.96992686245492));
#48262=CARTESIAN_POINT('Ctrl Pts',(-1.3038291566161,-0.769609523625295,
1.34041816052587));
#48263=CARTESIAN_POINT('',(-1.0574149561462,-1.3458803547932,0.22));
#48264=CARTESIAN_POINT('Origin',(0.,0.,0.22));
#48265=CARTESIAN_POINT('Ctrl Pts',(-1.05741495614621,-1.3458803547932,0.22));
#48266=CARTESIAN_POINT('Ctrl Pts',(-1.01779089885589,-1.29371349124397,
0.591471164251991));
#48267=CARTESIAN_POINT('Ctrl Pts',(-0.977366926097244,-1.24058473728836,
0.97002874200439));
#48268=CARTESIAN_POINT('Ctrl Pts',(-0.937769453804316,-1.18863692522509,
1.34041816052587));
#48269=CARTESIAN_POINT('',(-0.499822019709113,-1.63697839555501,0.22));
#48270=CARTESIAN_POINT('Origin',(0.,0.,0.22));
#48271=CARTESIAN_POINT('Ctrl Pts',(-0.499822019709112,-1.63697839555501,
0.22));
#48272=CARTESIAN_POINT('Ctrl Pts',(-0.481751415170154,-1.57413474259924,
0.590796411387241));
#48273=CARTESIAN_POINT('Ctrl Pts',(-0.463234151929265,-1.50993705749001,
0.969671099083018));
#48274=CARTESIAN_POINT('Ctrl Pts',(-0.445058789896327,-1.44713232360867,
1.34041816052587));
#48275=CARTESIAN_POINT('',(0.125274650099118,-1.70699343318669,0.22));
#48276=CARTESIAN_POINT('Origin',(0.,0.,0.22));
#48277=CARTESIAN_POINT('Ctrl Pts',(0.125274650099119,-1.70699343318669,
0.22));
#48278=CARTESIAN_POINT('Ctrl Pts',(0.119426587169905,-1.64190285944202,
0.59058437497945));
#48279=CARTESIAN_POINT('Ctrl Pts',(0.113500444422932,-1.57532801615826,
0.969590465098185));
#48280=CARTESIAN_POINT('Ctrl Pts',(0.107759529743048,-1.51018448285187,
1.34041816052587));
#48281=CARTESIAN_POINT('',(0.733452284240667,-1.54646954888937,0.22));
#48282=CARTESIAN_POINT('Origin',(0.,0.,0.22));
#48283=CARTESIAN_POINT('Ctrl Pts',(0.733452284240667,-1.54646954888937,
0.22));
#48284=CARTESIAN_POINT('Ctrl Pts',(0.704444345412884,-1.48780332282645,
0.591113453768949));
#48285=CARTESIAN_POINT('Ctrl Pts',(0.674891498357873,-1.42791069482832,
0.969829650214334));
#48286=CARTESIAN_POINT('Ctrl Pts',(0.64602432777446,-1.36927785946482,1.34041816052587));
#48287=CARTESIAN_POINT('',(1.2425731231961,-1.17708638273095,0.22));
#48288=CARTESIAN_POINT('Origin',(0.,0.,0.22));
#48289=CARTESIAN_POINT('Ctrl Pts',(1.2425731231961,-1.17708638273095,0.22));
#48290=CARTESIAN_POINT('Ctrl Pts',(1.19426284194958,-1.13279783604494,0.591640398518164));
#48291=CARTESIAN_POINT('Ctrl Pts',(1.14509967203354,-1.08765249687192,0.97012818472025));
#48292=CARTESIAN_POINT('Ctrl Pts',(1.09703996059555,-1.04344267372651,1.34041816052587));
#48293=CARTESIAN_POINT('Origin',(0.,0.,0.22));
#48294=CARTESIAN_POINT('',(1.71127058658217,-0.0327612331676529,0.22));
#48295=CARTESIAN_POINT('Origin',(0.,0.,0.22));
#48296=CARTESIAN_POINT('Ctrl Pts',(1.71127058658217,-0.0327612331676703,
0.22));
#48297=CARTESIAN_POINT('Ctrl Pts',(1.64592664790065,-0.0325785727675214,
0.590535827600031));
#48298=CARTESIAN_POINT('Ctrl Pts',(1.57907985913672,-0.0323366574975186,
0.96959378368857));
#48299=CARTESIAN_POINT('Ctrl Pts',(1.51368509711198,-0.0320423981330418,
1.34041816052587));
#48300=CARTESIAN_POINT('',(1.60754702144021,0.587633297864109,0.22));
#48301=CARTESIAN_POINT('Origin',(0.,0.,0.22));
#48302=CARTESIAN_POINT('Ctrl Pts',(1.60754702144021,0.587633297864116,0.22));
#48303=CARTESIAN_POINT('Ctrl Pts',(1.54648225330539,0.564172785329145,0.590945107425194));
#48304=CARTESIAN_POINT('Ctrl Pts',(1.48410498508378,0.540267047261947,0.969742390059058));
#48305=CARTESIAN_POINT('Ctrl Pts',(1.42304436641037,0.516927480140813,1.34041816052587));
#48306=CARTESIAN_POINT('',(1.2867153233272,1.12866469583084,0.22));
#48307=CARTESIAN_POINT('Origin',(0.,0.,0.22));
#48308=CARTESIAN_POINT('Ctrl Pts',(1.2867153233272,1.12866469583084,0.22));
#48309=CARTESIAN_POINT('Ctrl Pts',(1.23815819444723,1.08464693024256,0.591640390332101));
#48310=CARTESIAN_POINT('Ctrl Pts',(1.18866923188292,1.03985896774671,0.970128179719278));
#48311=CARTESIAN_POINT('Ctrl Pts',(1.14021360866399,0.996083437827605,1.34041816052587));
#48312=CARTESIAN_POINT('',(0.792105590863113,1.51726367247863,0.22));
#48313=CARTESIAN_POINT('Origin',(0.,0.,0.22));
#48314=CARTESIAN_POINT('Ctrl Pts',(0.79210559086311,1.51726367247863,0.22));
#48315=CARTESIAN_POINT('Ctrl Pts',(0.762770120472978,1.458760537755,0.591113453768949));
#48316=CARTESIAN_POINT('Ctrl Pts',(0.732784340782351,1.39908348459447,0.969829650214334));
#48317=CARTESIAN_POINT('Ctrl Pts',(0.703390684925826,1.34071280774691,1.34041816052587));
#48318=CARTESIAN_POINT('',(0.190517609144359,1.70094778270994,0.22));
#48319=CARTESIAN_POINT('Origin',(0.,0.,0.22));
#48320=CARTESIAN_POINT('Ctrl Pts',(0.190517609144358,1.70094778270994,0.22));
#48321=CARTESIAN_POINT('Ctrl Pts',(0.184305736149047,1.63589092093253,0.590584374979451));
#48322=CARTESIAN_POINT('Ctrl Pts',(0.177897879702104,1.56936071499665,0.969590465098185));
#48323=CARTESIAN_POINT('Ctrl Pts',(0.171570951566093,1.50427148383386,1.34041816052587));
#48324=CARTESIAN_POINT('',(-0.436800831383854,1.65490946960924,0.22));
#48325=CARTESIAN_POINT('Origin',(0.,0.,0.22));
#48326=CARTESIAN_POINT('Ctrl Pts',(-0.436800831383856,1.65490946960923,
0.22));
#48327=CARTESIAN_POINT('Ctrl Pts',(-0.419081848867252,1.59196577156245,
0.59079641138724));
#48328=CARTESIAN_POINT('Ctrl Pts',(-0.401029817157702,1.52763571666994,
0.969671099083018));
#48329=CARTESIAN_POINT('Ctrl Pts',(-0.383420389510104,1.46466996057301,
1.34041816052587));
#48330=CARTESIAN_POINT('',(-1.00512689923672,1.38536646246786,0.22));
#48331=CARTESIAN_POINT('Origin',(0.,0.,0.22));
#48332=CARTESIAN_POINT('Ctrl Pts',(-1.00512689923672,1.38536646246787,0.22));
#48333=CARTESIAN_POINT('Ctrl Pts',(-0.965795110148029,1.33297888821793,
0.591471164251991));
#48334=CARTESIAN_POINT('Ctrl Pts',(-0.925757057459429,1.27955870095344,
0.970028742004391));
#48335=CARTESIAN_POINT('Ctrl Pts',(-0.886628682377236,1.22725664312035,
1.34041816052587));
#48336=CARTESIAN_POINT('',(-1.43770500974724,0.928722037989635,0.22));
#48337=CARTESIAN_POINT('Origin',(0.,0.,0.22));
#48338=CARTESIAN_POINT('Ctrl Pts',(-1.43770500974724,0.928722037989638,
0.22));
#48339=CARTESIAN_POINT('Ctrl Pts',(-1.38213150110575,0.894097100294643,
0.591291663208604));
#48340=CARTESIAN_POINT('Ctrl Pts',(-1.32548789717734,0.858740459450525,
0.96992686245492));
#48341=CARTESIAN_POINT('Ctrl Pts',(-1.27009285871019,0.824095515550461,
1.34041816052587));
#48342=CARTESIAN_POINT('',(-1.67611309209293,0.346648556054452,0.22));
#48343=CARTESIAN_POINT('Origin',(0.,0.,0.22));
#48344=CARTESIAN_POINT('Ctrl Pts',(-1.67611309209293,0.346648556054445,
0.22));
#48345=CARTESIAN_POINT('Ctrl Pts',(-1.61189131020508,0.334457530502342,
0.590674417990065));
#48346=CARTESIAN_POINT('Ctrl Pts',(-1.54624662612018,0.321940354946836,
0.969620067809347));
#48347=CARTESIAN_POINT('Ctrl Pts',(-1.48202395664686,0.309635722134596,
1.34041816052587));
#48348=CARTESIAN_POINT('Origin',(0.,0.,0.22));
#48349=CARTESIAN_POINT('Origin',(1.75671243867939,-1.60145498856633,0.3482551044561));
#48350=CARTESIAN_POINT('',(1.17785560252371,-1.34078466352944,0.22));
#48351=CARTESIAN_POINT('Origin',(1.5109401069173,-1.37740390423071,0.277565129578061));
#48352=CARTESIAN_POINT('',(1.69921453277503,-0.768881160572422,0.22));
#48353=CARTESIAN_POINT('Origin',(1.42259216564977,-1.29686411401962,0.84));
#48354=CARTESIAN_POINT('Origin',(1.52189320170064,-1.38738896945528,0.22));
#48355=CARTESIAN_POINT('Origin',(1.05957329572431,-2.12791003183941,0.3482551044561));
#48356=CARTESIAN_POINT('',(0.613970353750137,-1.67573498473601,0.22));
#48357=CARTESIAN_POINT('Origin',(0.911334008616638,-1.83020541110008,0.277565129578061));
#48358=CARTESIAN_POINT('',(1.47637898190569,-1.24630651326724,0.22));
#48359=CARTESIAN_POINT('Origin',(0.858046334869837,-1.72318933585849,0.84));
#48360=CARTESIAN_POINT('Origin',(0.917940443729429,-1.84347292134022,0.22));
#48361=CARTESIAN_POINT('Origin',(0.219332907883337,-2.36697903415605,0.3482551044561));
#48362=CARTESIAN_POINT('',(-0.0328349934245695,-1.78436801068587,0.22));
#48363=CARTESIAN_POINT('Origin',(0.188647202576228,-2.0358275356821,0.277565129578061));
#48364=CARTESIAN_POINT('',(1.01216517589981,-1.68753448467274,0.22));
#48365=CARTESIAN_POINT('Origin',(0.177616591966855,-1.91678828936794,0.84));
#48366=CARTESIAN_POINT('Origin',(0.190014742348963,-2.05058564016207,0.22));
#48367=CARTESIAN_POINT('Origin',(-0.650529604532875,-2.28637440202631,0.3482551044561));
#48368=CARTESIAN_POINT('',(-0.675205792792306,-1.65201224926814,0.22));
#48369=CARTESIAN_POINT('Origin',(-0.559517453502335,-1.96649987066044,0.277565129578061));
#48370=CARTESIAN_POINT('',(0.306297263555869,-1.93127394609614,0.22));
#48371=CARTESIAN_POINT('Origin',(-0.52680125588876,-1.85151436310768,0.84));
#48372=CARTESIAN_POINT('Origin',(-0.563573502893763,-1.98075540559274,0.22));
#48373=CARTESIAN_POINT('Origin',(-1.43253448914795,-1.896982237665,0.3482551044561));
#48374=CARTESIAN_POINT('',(-1.22638630839899,-1.29654307947085,0.22));
#48375=CARTESIAN_POINT('Origin',(-1.23211617709217,-1.63158550135414,0.277565129578061));
#48376=CARTESIAN_POINT('',(-0.523913724701359,-1.82702575023449,0.22));
#48377=CARTESIAN_POINT('Origin',(-1.16007167503007,-1.53618316251446,0.84));
#48378=CARTESIAN_POINT('Origin',(-1.2410480237021,-1.64341317775352,0.22));
#48379=CARTESIAN_POINT('Origin',(-2.02106765305595,-1.25139211056558,0.3482551044561));
#48380=CARTESIAN_POINT('',(-1.61193655741525,-0.765968582397815,0.22));
#48381=CARTESIAN_POINT('Origin',(-1.73831078357428,-1.0763164691626,0.277565129578061));
#48382=CARTESIAN_POINT('',(-1.27088637074967,-1.31678354640376,0.22));
#48383=CARTESIAN_POINT('Origin',(-1.63666798627951,-1.01338191353891,0.84));
#48384=CARTESIAN_POINT('Origin',(-1.75091213202498,-1.0841188937919,0.22));
#48385=CARTESIAN_POINT('Origin',(-2.33664443129628,-0.43679454473122,0.3482551044561));
#48386=CARTESIAN_POINT('',(-1.77978584230378,-0.131945783893515,0.22));
#48387=CARTESIAN_POINT('Origin',(-2.00973688642211,-0.375684933735207,0.277565129578061));
#48388=CARTESIAN_POINT('',(-1.71463064913977,-0.480495281851195,0.22));
#48389=CARTESIAN_POINT('Origin',(-1.89222321689151,-0.353717821796897,0.84));
#48390=CARTESIAN_POINT('Origin',(-2.02430585477882,-0.378408345913518,0.22));
#48391=CARTESIAN_POINT('Origin',(-2.33664443129628,0.43679454473122,0.3482551044561));
#48392=CARTESIAN_POINT('',(-1.70726518705538,0.519897023862432,0.22));
#48393=CARTESIAN_POINT('Origin',(-2.00973688642211,0.375684933735208,0.277565129578061));
#48394=CARTESIAN_POINT('',(-1.71463064913977,0.480495281851196,0.22));
#48395=CARTESIAN_POINT('Origin',(-1.89222321689151,0.353717821796898,0.84));
#48396=CARTESIAN_POINT('Origin',(-2.02430585477882,0.378408345913518,0.22));
#48397=CARTESIAN_POINT('Origin',(-2.02106765305595,1.25139211056558,0.3482551044561));
#48398=CARTESIAN_POINT('',(-1.40416890801217,1.1015248576969,0.22));
#48399=CARTESIAN_POINT('Origin',(-1.73831078357428,1.0763164691626,0.277565129578061));
#48400=CARTESIAN_POINT('',(-1.27088637074967,1.31678354640376,0.22));
#48401=CARTESIAN_POINT('Origin',(-1.63666798627951,1.01338191353891,0.84));
#48402=CARTESIAN_POINT('Origin',(-1.75091213202497,1.0841188937919,0.22));
#48403=CARTESIAN_POINT('Origin',(-1.43253448914794,1.896982237665,0.3482551044561));
#48404=CARTESIAN_POINT('',(-0.911431837173392,1.53438565573945,0.22));
#48405=CARTESIAN_POINT('Origin',(-1.23211617709217,1.63158550135414,0.277565129578061));
#48406=CARTESIAN_POINT('',(-0.523913724701358,1.82702575023449,0.22));
#48407=CARTESIAN_POINT('Origin',(-1.16007167503007,1.53618316251446,0.84));
#48408=CARTESIAN_POINT('Origin',(-1.2410480237021,1.64341317775352,0.22));
#48409=CARTESIAN_POINT('Origin',(-0.650529604532875,2.28637440202631,0.3482551044561));
#48410=CARTESIAN_POINT('',(-0.295600846306193,1.76001916864997,0.22));
#48411=CARTESIAN_POINT('Origin',(-0.559517453502335,1.96649987066044,0.277565129578062));
#48412=CARTESIAN_POINT('',(0.30629726355587,1.93127394609614,0.22));
#48413=CARTESIAN_POINT('Origin',(-0.52680125588876,1.85151436310768,0.84));
#48414=CARTESIAN_POINT('Origin',(-0.563573502893763,1.98075540559275,0.22));
#48415=CARTESIAN_POINT('Origin',(0.219332907883338,2.36697903415605,0.3482551044561));
#48416=CARTESIAN_POINT('',(0.360152676835491,1.74795234023142,0.22));
#48417=CARTESIAN_POINT('Origin',(0.188647202576229,2.0358275356821,0.277565129578061));
#48418=CARTESIAN_POINT('',(1.01216517589981,1.68753448467274,0.22));
#48419=CARTESIAN_POINT('Origin',(0.177616591966856,1.91678828936794,0.84));
#48420=CARTESIAN_POINT('Origin',(0.190014742348964,2.05058564016207,0.22));
#48421=CARTESIAN_POINT('Origin',(1.05957329572431,2.12791003183941,0.3482551044561));
#48422=CARTESIAN_POINT('',(0.967265585295667,1.49981486252633,0.22));
#48423=CARTESIAN_POINT('Origin',(0.911334008616637,1.83020541110008,0.277565129578061));
#48424=CARTESIAN_POINT('',(1.47637898190569,1.24630651326724,0.22));
#48425=CARTESIAN_POINT('Origin',(0.858046334869836,1.7231893358585,0.84));
#48426=CARTESIAN_POINT('Origin',(0.917940443729428,1.84347292134022,0.22));
#48427=CARTESIAN_POINT('Origin',(1.75671243867939,1.60145498856633,0.3482551044561));
#48428=CARTESIAN_POINT('',(1.44374391665803,1.04911907687602,0.22));
#48429=CARTESIAN_POINT('Origin',(1.5109401069173,1.37740390423071,0.277565129578062));
#48430=CARTESIAN_POINT('',(1.69921453277503,0.768881160572423,0.22));
#48431=CARTESIAN_POINT('Origin',(1.42259216564977,1.29686411401962,0.84));
#48432=CARTESIAN_POINT('Origin',(1.52189320170064,1.38738896945528,0.22));
#48433=CARTESIAN_POINT('Origin',(2.21659783251117,0.858714575118932,0.3482551044561));
#48434=CARTESIAN_POINT('',(1.72523663201451,0.45673394652411,0.22));
#48435=CARTESIAN_POINT('Origin',(1.90648537137062,0.738576367636477,0.277565129578061));
#48436=CARTESIAN_POINT('',(1.76562782918999,0.352472248043786,0.22));
#48437=CARTESIAN_POINT('Origin',(1.79500904160339,0.695390207410269,0.84));
#48438=CARTESIAN_POINT('Origin',(1.92030584968083,0.743930449457738,0.22));
#48439=CARTESIAN_POINT('Origin',(1.925,0.,0.84));
#48440=CARTESIAN_POINT('',(1.77372658035123,-0.197335634156047,0.22));
#48441=CARTESIAN_POINT('Origin',(2.05937055187959,5.55111512312578E-17,
0.22));
#48442=CARTESIAN_POINT('Origin',(2.04454922222021,0.,0.277565129578061));
#48443=CARTESIAN_POINT('Origin',(2.37711940646971,0.,0.3482551044561));
#48444=CARTESIAN_POINT('',(1.77372658035123,0.,0.22));
#48445=CARTESIAN_POINT('Origin',(0.,0.,0.03));
#48446=CARTESIAN_POINT('',(-1.25,-1.53080849893419E-16,0.06));
#48447=CARTESIAN_POINT('Origin',(0.,0.,0.0599999999999999));
#48448=CARTESIAN_POINT('',(-1.31,-1.60428730688303E-16,2.08166817117217E-17));
#48449=CARTESIAN_POINT('',(-1.28,-1.56754790290861E-16,0.03));
#48450=CARTESIAN_POINT('Origin',(0.,0.,0.));
#48451=CARTESIAN_POINT('Origin',(1.84,0.,0.));
#48452=CARTESIAN_POINT('',(-1.84,-2.25335011043113E-16,1.73472347597681E-17));
#48453=CARTESIAN_POINT('Origin',(0.,0.,0.));
#48454=CARTESIAN_POINT('Origin',(0.,0.,0.03));
#48455=CARTESIAN_POINT('',(-1.9,-2.32682891837997E-16,0.06));
#48456=CARTESIAN_POINT('Origin',(0.,0.,0.0599999999999999));
#48457=CARTESIAN_POINT('',(-1.87,-2.29008951440555E-16,0.03));
#48458=CARTESIAN_POINT('Origin',(0.,0.,0.14));
#48459=CARTESIAN_POINT('',(-1.9,-2.32682891837997E-16,0.22));
#48460=CARTESIAN_POINT('Origin',(0.,0.,0.22));
#48461=CARTESIAN_POINT('',(-1.9,-2.32682891837997E-16,0.14));
#48462=CARTESIAN_POINT('Origin',(1.71158415478175,0.,0.22));
#48463=CARTESIAN_POINT('Origin',(1.6,0.,1.36));
#48464=CARTESIAN_POINT('',(-1.6,-1.95943487863577E-16,1.36));
#48465=CARTESIAN_POINT('Origin',(0.,0.,1.36));
#48466=CARTESIAN_POINT('Origin',(0.,0.,1.43));
#48467=CARTESIAN_POINT('',(-1.6,-1.95943487863577E-16,1.5));
#48468=CARTESIAN_POINT('Origin',(0.,0.,1.5));
#48469=CARTESIAN_POINT('',(-1.6,-1.95943487863577E-16,1.43));
#48470=CARTESIAN_POINT('Origin',(1.31,0.,1.5));
#48471=CARTESIAN_POINT('',(-1.31,-1.60428730688303E-16,1.5));
#48472=CARTESIAN_POINT('Origin',(0.,0.,1.5));
#48473=CARTESIAN_POINT('Origin',(0.,0.,1.47));
#48474=CARTESIAN_POINT('',(-1.25,-1.53080849893419E-16,1.44));
#48475=CARTESIAN_POINT('',(-1.28,-1.56754790290861E-16,1.47));
#48476=CARTESIAN_POINT('Origin',(0.,0.,1.44));
#48477=CARTESIAN_POINT('Origin',(0.,0.,0.75));
#48478=CARTESIAN_POINT('',(-1.25,-1.53080849893419E-16,0.75));
#48479=CARTESIAN_POINT('',(0.,0.,0.));
#48480=CARTESIAN_POINT('Origin',(0.,0.,0.35));
#48481=CARTESIAN_POINT('',(-2.37133297968149,-2.90404534327949E-16,0.375));
#48482=CARTESIAN_POINT('Origin',(0.,0.,0.375));
#48483=CARTESIAN_POINT('',(-2.43379937982364,-2.98054462026784E-16,0.325));
#48484=CARTESIAN_POINT('',(-2.40256617975257,-2.94229498177366E-16,0.35));
#48485=CARTESIAN_POINT('Origin',(0.,0.,0.325));
#48486=CARTESIAN_POINT('Origin',(2.54,0.,0.325));
#48487=CARTESIAN_POINT('',(-2.54,-3.11060286983428E-16,0.325));
#48488=CARTESIAN_POINT('Origin',(0.,0.,0.325));
#48489=CARTESIAN_POINT('Origin',(0.,0.,0.355));
#48490=CARTESIAN_POINT('',(-2.6,-3.18408167778312E-16,0.385));
#48491=CARTESIAN_POINT('Origin',(0.,0.,0.385));
#48492=CARTESIAN_POINT('',(-2.57,-3.1473422738087E-16,0.355));
#48493=CARTESIAN_POINT('Origin',(0.,0.,0.975));
#48494=CARTESIAN_POINT('',(-2.6,-3.18408167778312E-16,1.565));
#48495=CARTESIAN_POINT('Origin',(0.,0.,1.565));
#48496=CARTESIAN_POINT('',(-2.6,-3.18408167778312E-16,0.975));
#48497=CARTESIAN_POINT('Origin',(0.,0.,1.595));
#48498=CARTESIAN_POINT('',(-2.54,-3.11060286983428E-16,1.625));
#48499=CARTESIAN_POINT('Origin',(0.,0.,1.625));
#48500=CARTESIAN_POINT('',(-2.57,-3.1473422738087E-16,1.595));
#48501=CARTESIAN_POINT('Origin',(2.10967297612751,0.,1.625));
#48502=CARTESIAN_POINT('',(-2.10967297612751,-2.58360425746223E-16,1.625));
#48503=CARTESIAN_POINT('Origin',(0.,0.,1.625));
#48504=CARTESIAN_POINT('Origin',(0.,0.,1.6));
#48505=CARTESIAN_POINT('',(-2.07213937626967,-2.53763885453584E-16,1.575));
#48506=CARTESIAN_POINT('',(-2.09090617619859,-2.56062155599903E-16,1.6));
#48507=CARTESIAN_POINT('Origin',(0.,0.,1.575));
#48508=CARTESIAN_POINT('Origin',(0.,0.,0.975));
#48509=CARTESIAN_POINT('',(-2.22173617797558,-2.72084209890766E-16,0.975));
#48510=CARTESIAN_POINT('',(0.,0.,0.));
#48511=CARTESIAN_POINT('Origin',(-1.43138504711854,-0.60758690480082,0.12));
#48512=CARTESIAN_POINT('',(-1.53138504711854,-0.60758690480082,0.12));
#48513=CARTESIAN_POINT('Origin',(-1.43138504711854,-0.60758690480082,0.12));
#48514=CARTESIAN_POINT('',(-1.53138504711854,-0.60758690480082,0.));
#48515=CARTESIAN_POINT('',(-1.53138504711854,-0.60758690480082,0.12));
#48516=CARTESIAN_POINT('Origin',(-1.43138504711854,-0.60758690480082,0.));
#48517=CARTESIAN_POINT('Origin',(-1.43138504711854,0.607586904800821,0.12));
#48518=CARTESIAN_POINT('',(-1.53138504711854,0.607586904800821,0.12));
#48519=CARTESIAN_POINT('Origin',(-1.43138504711854,0.607586904800821,0.12));
#48520=CARTESIAN_POINT('',(-1.53138504711854,0.607586904800821,0.));
#48521=CARTESIAN_POINT('',(-1.53138504711854,0.607586904800821,0.12));
#48522=CARTESIAN_POINT('Origin',(-1.43138504711854,0.607586904800821,0.));
#48523=CARTESIAN_POINT('Origin',(-1.46712320635062,-0.916760327123444,0.));
#48524=CARTESIAN_POINT('',(-1.29751358711933,-0.810776474276803,0.));
#48525=CARTESIAN_POINT('',(-1.46712320635062,-0.916760327123444,0.));
#48526=CARTESIAN_POINT('',(-1.29751358711933,-0.810776474276803,0.));
#48527=CARTESIAN_POINT('',(-1.29751358711933,-0.810776474276803,0.12));
#48528=CARTESIAN_POINT('',(-1.29751358711933,-0.810776474276803,0.));
#48529=CARTESIAN_POINT('',(-1.46712320635062,-0.916760327123444,0.12));
#48530=CARTESIAN_POINT('',(-1.29751358711933,-0.810776474276803,0.12));
#48531=CARTESIAN_POINT('',(-1.46712320635062,-0.916760327123444,0.));
#48532=CARTESIAN_POINT('Origin',(-1.44710519783383,-0.588549333387818,0.));
#48533=CARTESIAN_POINT('',(-1.73682935003403,-0.433040193123405,0.));
#48534=CARTESIAN_POINT('Origin',(-1.44710519783383,-0.588549333387818,0.));
#48535=CARTESIAN_POINT('',(-1.73682935003403,-0.433040193123405,0.12));
#48536=CARTESIAN_POINT('Origin',(-1.44710519783383,-0.588549333387818,0.12));
#48537=CARTESIAN_POINT('',(-1.73682935003403,-0.433040193123405,0.));
#48538=CARTESIAN_POINT('Origin',(-1.15950339289982,-0.289096665241603,0.));
#48539=CARTESIAN_POINT('',(-1.15950339289982,-0.289096665241603,0.));
#48540=CARTESIAN_POINT('',(-1.73682935003403,-0.433040193123405,0.));
#48541=CARTESIAN_POINT('',(-1.15950339289982,-0.289096665241603,0.12));
#48542=CARTESIAN_POINT('',(-1.73682935003403,-0.433040193123405,0.12));
#48543=CARTESIAN_POINT('',(-1.15950339289982,-0.289096665241603,0.));
#48544=CARTESIAN_POINT('Origin',(-4.16333634234434E-17,1.38777878078145E-16,
0.));
#48545=CARTESIAN_POINT('',(-1.15950339289982,0.289096665241603,0.));
#48546=CARTESIAN_POINT('Origin',(-4.16333634234434E-17,1.38777878078145E-16,
0.));
#48547=CARTESIAN_POINT('',(-1.15950339289982,0.289096665241603,0.12));
#48548=CARTESIAN_POINT('Origin',(-4.16333634234434E-17,1.38777878078145E-16,
0.12));
#48549=CARTESIAN_POINT('',(-1.15950339289982,0.289096665241603,0.));
#48550=CARTESIAN_POINT('Origin',(-1.73682935003403,0.433040193123405,0.));
#48551=CARTESIAN_POINT('',(-1.73682935003403,0.433040193123405,0.));
#48552=CARTESIAN_POINT('',(-1.15950339289982,0.289096665241603,0.));
#48553=CARTESIAN_POINT('',(-1.73682935003403,0.433040193123405,0.12));
#48554=CARTESIAN_POINT('',(-1.15950339289982,0.289096665241603,0.12));
#48555=CARTESIAN_POINT('',(-1.73682935003403,0.433040193123405,0.));
#48556=CARTESIAN_POINT('Origin',(-1.44710519783383,0.588549333387818,0.));
#48557=CARTESIAN_POINT('',(-1.46712320635062,0.916760327123444,0.));
#48558=CARTESIAN_POINT('Origin',(-1.44710519783383,0.588549333387818,0.));
#48559=CARTESIAN_POINT('',(-1.46712320635062,0.916760327123444,0.12));
#48560=CARTESIAN_POINT('Origin',(-1.44710519783383,0.588549333387818,0.12));
#48561=CARTESIAN_POINT('',(-1.46712320635062,0.916760327123444,0.));
#48562=CARTESIAN_POINT('Origin',(-1.29751358711933,0.810776474276804,0.));
#48563=CARTESIAN_POINT('',(-1.29751358711933,0.810776474276804,0.));
#48564=CARTESIAN_POINT('',(-1.46712320635062,0.916760327123444,0.));
#48565=CARTESIAN_POINT('',(-1.29751358711933,0.810776474276804,0.12));
#48566=CARTESIAN_POINT('',(-1.46712320635062,0.916760327123444,0.12));
#48567=CARTESIAN_POINT('',(-1.29751358711933,0.810776474276804,0.));
#48568=CARTESIAN_POINT('Origin',(5.55111512312578E-17,-2.77555756156289E-16,
0.));
#48569=CARTESIAN_POINT('Origin',(5.55111512312578E-17,-2.77555756156289E-16,
0.));
#48570=CARTESIAN_POINT('Origin',(5.55111512312578E-17,-2.77555756156289E-16,
0.12));
#48571=CARTESIAN_POINT('Origin',(-0.122963043440601,-2.22044604925031E-16,
0.12));
#48572=CARTESIAN_POINT('Origin',(-0.122963043440601,-2.22044604925031E-16,
0.));
#48573=CARTESIAN_POINT('',(0.,0.,0.));
#48574=CARTESIAN_POINT('Origin',(0.,0.,-2.22));
#48575=CARTESIAN_POINT('',(-0.393952734404645,4.1940781306567E-5,-2.7812836477965));
#48576=CARTESIAN_POINT('',(-0.394010867405998,5.4694194531556E-5,-2.7996163522035));
#48577=CARTESIAN_POINT('',(-0.3933,-4.81653586104654E-17,-2.22));
#48578=CARTESIAN_POINT('',(0.386880458087545,0.0743511284475749,-2.84));
#48579=CARTESIAN_POINT('Ctrl Pts',(-0.393952734404645,4.1940781306567E-5,
-2.7812836477965));
#48580=CARTESIAN_POINT('Ctrl Pts',(-0.393956887618347,0.00257921210189992,
-2.78141257124883));
#48581=CARTESIAN_POINT('Ctrl Pts',(-0.39393432800773,0.00511641073810632,
-2.78154149470116));
#48582=CARTESIAN_POINT('Ctrl Pts',(-0.393884823371554,0.00765309135505756,
-2.78167041815349));
#48583=CARTESIAN_POINT('Ctrl Pts',(-0.391341925890778,0.137954397427497,
-2.78829281046787));
#48584=CARTESIAN_POINT('Ctrl Pts',(-0.317703128330192,0.266888881816179,
-2.79491520278225));
#48585=CARTESIAN_POINT('Ctrl Pts',(-0.206805076321773,0.335299228187672,
-2.80153759509663));
#48586=CARTESIAN_POINT('Ctrl Pts',(-0.0959070243133527,0.403709574559165,
-2.80815998741101));
#48587=CARTESIAN_POINT('Ctrl Pts',(0.0522502821429009,0.411595782913467,
-2.81478237972539));
#48588=CARTESIAN_POINT('Ctrl Pts',(0.169863896558048,0.355408659714183,
-2.82140477203977));
#48589=CARTESIAN_POINT('Ctrl Pts',(0.279947577673663,0.302818784096202,
-2.82760318135985));
#48590=CARTESIAN_POINT('Ctrl Pts',(0.363273346469767,0.194097233714658,
-2.83380159067992));
#48591=CARTESIAN_POINT('Ctrl Pts',(0.386886490162192,0.0743511351644956,
-2.84));
#48592=CARTESIAN_POINT('',(-0.3933,-4.81653586104654E-17,-2.84));
#48593=CARTESIAN_POINT('Origin',(0.,0.,-2.84));
#48594=CARTESIAN_POINT('',(-0.3933,-4.81653586104654E-17,-4.4467));
#48595=CARTESIAN_POINT('',(-0.3933,-4.81653586104654E-17,-2.22));
#48596=CARTESIAN_POINT('Origin',(0.,0.,-4.4467));
#48597=CARTESIAN_POINT('',(0.174290087240704,0.352573191677455,-2.84));
#48598=CARTESIAN_POINT('Origin',(0.,0.,-2.84));
#48599=CARTESIAN_POINT('Ctrl Pts',(0.174290087240704,0.352573191677456,
-2.84));
#48600=CARTESIAN_POINT('Ctrl Pts',(0.0569263183517564,0.410590482842535,
-2.83337760768562));
#48601=CARTESIAN_POINT('Ctrl Pts',(-0.090669376315471,0.404886350107643,
-2.82675521537124));
#48602=CARTESIAN_POINT('Ctrl Pts',(-0.202271457956682,0.338016611261013,
-2.82013282305686));
#48603=CARTESIAN_POINT('Ctrl Pts',(-0.313873539597893,0.271146872414382,
-2.81351043074248));
#48604=CARTESIAN_POINT('Ctrl Pts',(-0.389482008213088,0.143111527456014,
-2.8068880384281));
#48605=CARTESIAN_POINT('Ctrl Pts',(-0.393813496269577,0.0128329553269884,
-2.80026564611372));
#48606=CARTESIAN_POINT('Ctrl Pts',(-0.393955056835797,0.00857522491277192,
-2.80004921481031));
#48607=CARTESIAN_POINT('Ctrl Pts',(-0.394020486735239,0.0043150985163057,
-2.79983278350691));
#48608=CARTESIAN_POINT('Ctrl Pts',(-0.394010867405998,5.4694194531556E-5,
-2.7996163522035));
#48609=CARTESIAN_POINT('Origin',(0.,0.,-2.22));
#48610=CARTESIAN_POINT('',(-0.39300565221066,0.000328329871180644,-2.6562836477965));
#48611=CARTESIAN_POINT('',(-0.392962952735427,0.00031460754753748,-2.6746163522035));
#48612=CARTESIAN_POINT('',(-0.3933,-4.81653586104654E-17,-2.22));
#48613=CARTESIAN_POINT('Ctrl Pts',(-0.39300565221066,0.000328329871180644,
-2.6562836477965));
#48614=CARTESIAN_POINT('Ctrl Pts',(-0.39332720747469,0.0411433485463145,
-2.65834488402921));
#48615=CARTESIAN_POINT('Ctrl Pts',(-0.387477274673374,0.081868491656979,
-2.66040612026193));
#48616=CARTESIAN_POINT('Ctrl Pts',(-0.375071232908909,0.120487600583847,
-2.66246735649464));
#48617=CARTESIAN_POINT('Ctrl Pts',(-0.335212785667873,0.244564058239049,
-2.66908974880902));
#48618=CARTESIAN_POINT('Ctrl Pts',(-0.227680558122831,0.346901509500663,
-2.6757121411234));
#48619=CARTESIAN_POINT('Ctrl Pts',(-0.101784662090584,0.380572608550405,
-2.68233453343778));
#48620=CARTESIAN_POINT('Ctrl Pts',(0.0241112339416628,0.414243707600147,
-2.68895692575216));
#48621=CARTESIAN_POINT('Ctrl Pts',(0.168370798461114,0.379248454438019,
-2.69557931806654));
#48622=CARTESIAN_POINT('Ctrl Pts',(0.264846786191469,0.291635199129418,
-2.70220171038092));
#48623=CARTESIAN_POINT('Ctrl Pts',(0.361322773921825,0.204021943820817,
-2.7088241026953));
#48624=CARTESIAN_POINT('Ctrl Pts',(0.410015184863085,0.0637906863657433,
-2.71544649500968));
#48625=CARTESIAN_POINT('Ctrl Pts',(0.388591027578597,-0.0647583673116287,
-2.72206888732406));
#48626=CARTESIAN_POINT('Ctrl Pts',(0.367166870294109,-0.193307420989001,
-2.72869127963844));
#48627=CARTESIAN_POINT('Ctrl Pts',(0.275626144783873,-0.310174270888672,
-2.73531367195282));
#48628=CARTESIAN_POINT('Ctrl Pts',(0.155954592874106,-0.361764920745412,
-2.7419360642672));
#48629=CARTESIAN_POINT('Ctrl Pts',(0.036283040964339,-0.413355570602153,
-2.74855845658158));
#48630=CARTESIAN_POINT('Ctrl Pts',(-0.111519337344959,-0.399670020415965,
-2.75518084889597));
#48631=CARTESIAN_POINT('Ctrl Pts',(-0.219697027799126,-0.326993181444773,
-2.76180324121035));
#48632=CARTESIAN_POINT('Ctrl Pts',(-0.325768735904897,-0.255731201113731,
-2.7682967100724));
#48633=CARTESIAN_POINT('Ctrl Pts',(-0.393743550091291,-0.127752436559022,
-2.77479017893445));
#48634=CARTESIAN_POINT('Ctrl Pts',(-0.393952734404645,4.1940781306567E-5,
-2.7812836477965));
#48635=CARTESIAN_POINT('Ctrl Pts',(-0.394010867405998,5.4694194531556E-5,
-2.7996163522035));
#48636=CARTESIAN_POINT('Ctrl Pts',(-0.393726153286074,-0.126045290173359,
-2.79321039119253));
#48637=CARTESIAN_POINT('Ctrl Pts',(-0.327694632260249,-0.252388750748456,
-2.78680443018155));
#48638=CARTESIAN_POINT('Ctrl Pts',(-0.223957356921664,-0.32405571896141,
-2.78039846917058));
#48639=CARTESIAN_POINT('Ctrl Pts',(-0.11671522201948,-0.3981440218211,-2.7737760768562));
#48640=CARTESIAN_POINT('Ctrl Pts',(0.0308235552826724,-0.413798828240797,
-2.76715368454182));
#48641=CARTESIAN_POINT('Ctrl Pts',(0.151148649024799,-0.363796630115481,
-2.76053129222743));
#48642=CARTESIAN_POINT('Ctrl Pts',(0.271473742766925,-0.313794431990164,
-2.75390889991305));
#48643=CARTESIAN_POINT('Ctrl Pts',(0.364585152949026,-0.198135229319833,
-2.74728650759867));
#48644=CARTESIAN_POINT('Ctrl Pts',(0.387712443649385,-0.0698775765452277,
-2.74066411528429));
#48645=CARTESIAN_POINT('Ctrl Pts',(0.410839734349744,0.0583800762293768,
-2.73404172296991));
#48646=CARTESIAN_POINT('Ctrl Pts',(0.363982905568364,0.199236179108254,
-2.72741933065553));
#48647=CARTESIAN_POINT('Ctrl Pts',(0.268666865662216,0.288113545745012,
-2.72079693834115));
#48648=CARTESIAN_POINT('Ctrl Pts',(0.173350825756067,0.376990912381769,
-2.71417454602677));
#48649=CARTESIAN_POINT('Ctrl Pts',(0.0295755747251501,0.413889542776405,
-2.70755215371239));
#48650=CARTESIAN_POINT('Ctrl Pts',(-0.0967512798405108,0.381883315850353,
-2.70092976139801));
#48651=CARTESIAN_POINT('Ctrl Pts',(-0.223078134406171,0.3498770889243,-2.69430736908363));
#48652=CARTESIAN_POINT('Ctrl Pts',(-0.331956592506576,0.24896600467756,
-2.68768497676925));
#48653=CARTESIAN_POINT('Ctrl Pts',(-0.373450060077915,0.125425952738769,
-2.68106258445487));
#48654=CARTESIAN_POINT('Ctrl Pts',(-0.386913297942314,0.0853413514175464,
-2.67891384037108));
#48655=CARTESIAN_POINT('Ctrl Pts',(-0.393282346889808,0.0428744069284828,
-2.67676509628729));
#48656=CARTESIAN_POINT('Ctrl Pts',(-0.392962952735427,0.00031460754753748,
-2.6746163522035));
#48657=CARTESIAN_POINT('Origin',(0.,0.,-2.22));
#48658=CARTESIAN_POINT('',(-0.39276380274066,-0.000209749112361407,-2.5312836477965));
#48659=CARTESIAN_POINT('',(-0.392793287557452,-0.000232553243135302,-2.5496163522035));
#48660=CARTESIAN_POINT('',(-0.3933,-4.81653586104654E-17,-2.22));
#48661=CARTESIAN_POINT('Ctrl Pts',(-0.39276380274066,-0.000209749112361407,
-2.5312836477965));
#48662=CARTESIAN_POINT('Ctrl Pts',(-0.392381433345052,0.0789898077510052,
-2.5352771968096));
#48663=CARTESIAN_POINT('Ctrl Pts',(-0.369164685986063,0.158395566123688,
-2.5392707458227));
#48664=CARTESIAN_POINT('Ctrl Pts',(-0.324646816974723,0.223159140648563,
-2.54326429483579));
#48665=CARTESIAN_POINT('Ctrl Pts',(-0.250824061168682,0.330554792180273,
-2.54988668715017));
#48666=CARTESIAN_POINT('Ctrl Pts',(-0.118426042679012,0.397686377849861,
-2.55650907946455));
#48667=CARTESIAN_POINT('Ctrl Pts',(0.011836349297656,0.393770822005192,
-2.56313147177893));
#48668=CARTESIAN_POINT('Ctrl Pts',(0.142098741274323,0.389855266160524,
-2.56975386409331));
#48669=CARTESIAN_POINT('Ctrl Pts',(0.270225506737988,0.3148925688016,-2.5763762564077));
#48670=CARTESIAN_POINT('Ctrl Pts',(0.337464415042443,0.203256760030363,
-2.58299864872208));
#48671=CARTESIAN_POINT('Ctrl Pts',(0.404703323346898,0.0916209512591259,
-2.58962104103646));
#48672=CARTESIAN_POINT('Ctrl Pts',(0.411054374492143,-0.0566879689244253,
-2.59624343335084));
#48673=CARTESIAN_POINT('Ctrl Pts',(0.353605200899493,-0.173663278362041,
-2.60286582566522));
#48674=CARTESIAN_POINT('Ctrl Pts',(0.296156027306843,-0.290638587799656,
-2.6094882179796));
#48675=CARTESIAN_POINT('Ctrl Pts',(0.174906628976298,-0.376280286491338,
-2.61611061029398));
#48676=CARTESIAN_POINT('Ctrl Pts',(0.0454558890327329,-0.391317435834831,
-2.62273300260836));
#48677=CARTESIAN_POINT('Ctrl Pts',(-0.0839948509108324,-0.406354585178324,
-2.62935539492274));
#48678=CARTESIAN_POINT('Ctrl Pts',(-0.221646932467417,-0.350787185173631,
-2.63597778723712));
#48679=CARTESIAN_POINT('Ctrl Pts',(-0.304380639777195,-0.250095753146889,
-2.6426001795515));
#48680=CARTESIAN_POINT('Ctrl Pts',(-0.361363272992008,-0.18074478211436,
-2.64716133563317));
#48681=CARTESIAN_POINT('Ctrl Pts',(-0.392294106525188,-0.0899881839271938,
-2.65172249171483));
#48682=CARTESIAN_POINT('Ctrl Pts',(-0.39300565221066,0.000328329871180644,
-2.6562836477965));
#48683=CARTESIAN_POINT('Ctrl Pts',(-0.392962952735427,0.00031460754753748,
-2.6746163522035));
#48684=CARTESIAN_POINT('Ctrl Pts',(-0.392297979598613,-0.0882941628644968,
-2.67014270397291));
#48685=CARTESIAN_POINT('Ctrl Pts',(-0.362640930570418,-0.177305426955751,
-2.66566905574232));
#48686=CARTESIAN_POINT('Ctrl Pts',(-0.307653528440411,-0.246057304588508,
-2.66119540751173));
#48687=CARTESIAN_POINT('Ctrl Pts',(-0.226255052189297,-0.347831490346152,
-2.65457301519735));
#48688=CARTESIAN_POINT('Ctrl Pts',(-0.0893496226447939,-0.405210842230597,
-2.64795062288297));
#48689=CARTESIAN_POINT('Ctrl Pts',(0.0402879227865041,-0.391883265826329,
-2.64132823056859));
#48690=CARTESIAN_POINT('Ctrl Pts',(0.169925468217803,-0.378555689422062,
-2.63470583825421));
#48691=CARTESIAN_POINT('Ctrl Pts',(0.292295129535897,-0.294521184729083,
-2.62808344593983));
#48692=CARTESIAN_POINT('Ctrl Pts',(0.35128302181726,-0.178314085485268,
-2.62146105362545));
#48693=CARTESIAN_POINT('Ctrl Pts',(0.410270914098623,-0.0621069862414521,
-2.61483866131107));
#48694=CARTESIAN_POINT('Ctrl Pts',(0.405877037343254,0.0862727075531994,
-2.60821626899669));
#48695=CARTESIAN_POINT('Ctrl Pts',(0.340116983457932,0.198786014393248,
-2.60159387668231));
#48696=CARTESIAN_POINT('Ctrl Pts',(0.274356929572611,0.311299321233295,
-2.59497148436793));
#48697=CARTESIAN_POINT('Ctrl Pts',(0.147230698557337,0.38794624111874,-2.58834909205354));
#48698=CARTESIAN_POINT('Ctrl Pts',(0.0170313711229766,0.393580345679592,
-2.58172669973916));
#48699=CARTESIAN_POINT('Ctrl Pts',(-0.113167956311385,0.399214450240444,
-2.57510430742478));
#48700=CARTESIAN_POINT('Ctrl Pts',(-0.246440380164833,0.333835739476704,
-2.5684819151104));
#48701=CARTESIAN_POINT('Ctrl Pts',(-0.321673867949857,0.227423564450892,
-2.56185952279602));
#48702=CARTESIAN_POINT('Ctrl Pts',(-0.368036591141922,0.161846939463297,
-2.55777846593185));
#48703=CARTESIAN_POINT('Ctrl Pts',(-0.392358130091861,0.080687221346171,
-2.55369740906767));
#48704=CARTESIAN_POINT('Ctrl Pts',(-0.392793287557452,-0.000232553243135302,
-2.5496163522035));
#48705=CARTESIAN_POINT('Origin',(0.,0.,-2.22));
#48706=CARTESIAN_POINT('',(-0.393773264356009,-0.00023371002059569,-2.4062836477965));
#48707=CARTESIAN_POINT('',(-0.393810998789827,-0.000208891560843762,-2.4246163522035));
#48708=CARTESIAN_POINT('',(-0.3933,-4.81653586104654E-17,-2.22));
#48709=CARTESIAN_POINT('Ctrl Pts',(-0.393773264356009,-0.00023371002059569,
-2.4062836477965));
#48710=CARTESIAN_POINT('Ctrl Pts',(-0.392952500563531,0.11651851875429,
-2.41220950958998));
#48711=CARTESIAN_POINT('Ctrl Pts',(-0.337733951007006,0.23394492666379,
-2.41813537138347));
#48712=CARTESIAN_POINT('Ctrl Pts',(-0.24685270843109,0.307016768785737,
-2.42406123317695));
#48713=CARTESIAN_POINT('Ctrl Pts',(-0.145289212127785,0.388677533503259,
-2.43068362549133));
#48714=CARTESIAN_POINT('Ctrl Pts',(0.000813329977278038,0.414943994822137,
-2.43730601780571));
#48715=CARTESIAN_POINT('Ctrl Pts',(0.124459873438975,0.373771716382449,
-2.44392841012009));
#48716=CARTESIAN_POINT('Ctrl Pts',(0.248106416900672,0.332599437942762,
-2.45055080243447));
#48717=CARTESIAN_POINT('Ctrl Pts',(0.349296961719004,0.22398841974451,-2.45717319474885));
#48718=CARTESIAN_POINT('Ctrl Pts',(0.381630776406502,0.0977420389515133,
-2.46379558706323));
#48719=CARTESIAN_POINT('Ctrl Pts',(0.413964591094,-0.0285043418414835,-2.47041797937761));
#48720=CARTESIAN_POINT('Ctrl Pts',(0.377441675650666,-0.172386085229224,
-2.47704037169199));
#48721=CARTESIAN_POINT('Ctrl Pts',(0.288809541620048,-0.267926491451958,
-2.48366276400637));
#48722=CARTESIAN_POINT('Ctrl Pts',(0.200177407589429,-0.363466897674693,
-2.49028515632075));
#48723=CARTESIAN_POINT('Ctrl Pts',(0.0594360549715268,-0.41066596673242,
-2.49690754863513));
#48724=CARTESIAN_POINT('Ctrl Pts',(-0.0688778315672936,-0.387880652908061,
-2.50352994094951));
#48725=CARTESIAN_POINT('Ctrl Pts',(-0.197191718106114,-0.365095339083702,
-2.51015233326389));
#48726=CARTESIAN_POINT('Ctrl Pts',(-0.313078138565853,-0.272325642377255,
-2.51677472557827));
#48727=CARTESIAN_POINT('Ctrl Pts',(-0.363397602234515,-0.152110935327116,
-2.52339711789265));
#48728=CARTESIAN_POINT('Ctrl Pts',(-0.383372556708641,-0.104390170331315,
-2.52602596119393));
#48729=CARTESIAN_POINT('Ctrl Pts',(-0.3930155059803,-0.0523446356110889,
-2.52865480449522));
#48730=CARTESIAN_POINT('Ctrl Pts',(-0.39276380274066,-0.000209749112361407,
-2.5312836477965));
#48731=CARTESIAN_POINT('Ctrl Pts',(-0.392793287557452,-0.000232553243135302,
-2.5496163522035));
#48732=CARTESIAN_POINT('Ctrl Pts',(-0.39306426665197,-0.0506225131556464,
-2.54707501675329));
#48733=CARTESIAN_POINT('Ctrl Pts',(-0.384072727828695,-0.10091942920435,
-2.54453368130309));
#48734=CARTESIAN_POINT('Ctrl Pts',(-0.365373106319892,-0.147302469940018,
-2.54199234585288));
#48735=CARTESIAN_POINT('Ctrl Pts',(-0.316644305188305,-0.268170690017237,
-2.5353699535385));
#48736=CARTESIAN_POINT('Ctrl Pts',(-0.201992151208531,-0.362461490883791,
-2.52874756122412));
#48737=CARTESIAN_POINT('Ctrl Pts',(-0.0739901136783288,-0.386937986140273,
-2.52212516890974));
#48738=CARTESIAN_POINT('Ctrl Pts',(0.0540119238518717,-0.411414481396754,
-2.51550277659536));
#48739=CARTESIAN_POINT('Ctrl Pts',(0.1953638449325,-0.366076671043165,-2.50888038428098));
#48740=CARTESIAN_POINT('Ctrl Pts',(0.285248963317479,-0.271714131682789,
-2.5022579919666));
#48741=CARTESIAN_POINT('Ctrl Pts',(0.375134081702459,-0.177351592322412,
-2.49563559965222));
#48742=CARTESIAN_POINT('Ctrl Pts',(0.413552397391789,-0.0339643239552482,
-2.48901320733784));
#48743=CARTESIAN_POINT('Ctrl Pts',(0.38288728052918,0.0926977181808754,
-2.48239081502346));
#48744=CARTESIAN_POINT('Ctrl Pts',(0.352222163666571,0.219359760317,-2.47576842270908));
#48745=CARTESIAN_POINT('Ctrl Pts',(0.252473614252022,0.329296576222083,
-2.4691460303947));
#48746=CARTESIAN_POINT('Ctrl Pts',(0.12938113226254,0.372096844648535,-2.46252363808032));
#48747=CARTESIAN_POINT('Ctrl Pts',(0.00628865027305796,0.414897113074987,
-2.45590124576594));
#48748=CARTESIAN_POINT('Ctrl Pts',(-0.140147764291357,0.390560834022808,
-2.44927885345156));
#48749=CARTESIAN_POINT('Ctrl Pts',(-0.242779966614497,0.310247363505348,
-2.44265646113718));
#48750=CARTESIAN_POINT('Ctrl Pts',(-0.335973685848564,0.237319852912212,
-2.43664309149262));
#48751=CARTESIAN_POINT('Ctrl Pts',(-0.393049557048956,0.118237518587536,
-2.43062972184806));
#48752=CARTESIAN_POINT('Ctrl Pts',(-0.393810998789827,-0.000208891560843762,
-2.4246163522035));
#48753=CARTESIAN_POINT('Origin',(0.,0.,-2.22));
#48754=CARTESIAN_POINT('',(-0.393484494376611,0.000340583921978138,-2.2812836477965));
#48755=CARTESIAN_POINT('',(-0.393432313413097,0.00034956597777247,-2.2996163522035));
#48756=CARTESIAN_POINT('',(-0.3933,-4.81653586104654E-17,-2.22));
#48757=CARTESIAN_POINT('Ctrl Pts',(-0.393484494376611,0.000340583921978138,
-2.2812836477965));
#48758=CARTESIAN_POINT('Ctrl Pts',(-0.39370719115912,0.0247346784797741,
-2.28251943005599));
#48759=CARTESIAN_POINT('Ctrl Pts',(-0.391633797841506,0.0490910240555078,
-2.28375521231547));
#48760=CARTESIAN_POINT('Ctrl Pts',(-0.387128134168714,0.0729887915576785,
-2.28499099457496));
#48761=CARTESIAN_POINT('Ctrl Pts',(-0.362982883458997,0.201053740396819,
-2.29161338688934));
#48762=CARTESIAN_POINT('Ctrl Pts',(-0.268989026604262,0.315949495614517,
-2.29823577920372));
#48763=CARTESIAN_POINT('Ctrl Pts',(-0.148247268569818,0.364990826350649,
-2.3048581715181));
#48764=CARTESIAN_POINT('Ctrl Pts',(-0.0275055105353745,0.41403215708678,
-2.31148056383248));
#48765=CARTESIAN_POINT('Ctrl Pts',(0.119984148678778,0.397219063341345,
-2.31810295614686));
#48766=CARTESIAN_POINT('Ctrl Pts',(0.226590605275426,0.322261157389841,
-2.32472534846124));
#48767=CARTESIAN_POINT('Ctrl Pts',(0.333197061872074,0.247303251438337,
-2.33134774077562));
#48768=CARTESIAN_POINT('Ctrl Pts',(0.398920315851218,0.114200533280764,
-2.33797013309));
#48769=CARTESIAN_POINT('Ctrl Pts',(0.393623093648558,-0.0160129978489424,
-2.34459252540438));
#48770=CARTESIAN_POINT('Ctrl Pts',(0.388325871445897,-0.14622652897865,
-2.35121491771876));
#48771=CARTESIAN_POINT('Ctrl Pts',(0.312008173061429,-0.27355087308049,
-2.35783731003314));
#48772=CARTESIAN_POINT('Ctrl Pts',(0.199665334447639,-0.339601693428282,
-2.36445970234752));
#48773=CARTESIAN_POINT('Ctrl Pts',(0.0873224958338501,-0.405652513776072,
-2.3710820946619));
#48774=CARTESIAN_POINT('Ctrl Pts',(-0.0610454830092596,-0.410429810369814,
-2.37770448697628));
#48775=CARTESIAN_POINT('Ctrl Pts',(-0.177404746411668,-0.351742962866779,
-2.38432687929066));
#48776=CARTESIAN_POINT('Ctrl Pts',(-0.293764009814075,-0.293056115363745,
-2.39094927160504));
#48777=CARTESIAN_POINT('Ctrl Pts',(-0.378114557775781,-0.170905123763935,
-2.39757166391942));
#48778=CARTESIAN_POINT('Ctrl Pts',(-0.391777606505862,-0.0413020939059466,
-2.4041940562338));
#48779=CARTESIAN_POINT('Ctrl Pts',(-0.393214659763545,-0.0276706958232436,
-2.4048905867547));
#48780=CARTESIAN_POINT('Ctrl Pts',(-0.393869737586711,-0.0139568600971337,
-2.4055871172756));
#48781=CARTESIAN_POINT('Ctrl Pts',(-0.393773264356009,-0.00023371002059569,
-2.4062836477965));
#48782=CARTESIAN_POINT('Ctrl Pts',(-0.393810998789827,-0.000208891560843762,
-2.4246163522035));
#48783=CARTESIAN_POINT('Ctrl Pts',(-0.393888116164835,-0.0122049192796106,
-2.42400732953368));
#48784=CARTESIAN_POINT('Ctrl Pts',(-0.393387602125509,-0.0241944241624916,
-2.42339830686386));
#48785=CARTESIAN_POINT('Ctrl Pts',(-0.392288475751339,-0.0361287983316595,
-2.42278928419403));
#48786=CARTESIAN_POINT('Ctrl Pts',(-0.380336792483176,-0.165900827668469,
-2.41616689187965));
#48787=CARTESIAN_POINT('Ctrl Pts',(-0.297605435864983,-0.289154224359348,
-2.40954449956527));
#48788=CARTESIAN_POINT('Ctrl Pts',(-0.182030711531421,-0.349371376506604,
-2.40292210725089));
#48789=CARTESIAN_POINT('Ctrl Pts',(-0.0664559871978615,-0.409588528653859,
-2.39629971493651));
#48790=CARTESIAN_POINT('Ctrl Pts',(0.0819621048510649,-0.406769436257494,
-2.38967732262213));
#48791=CARTESIAN_POINT('Ctrl Pts',(0.195166729089834,-0.342206788988941,
-2.38305493030775));
#48792=CARTESIAN_POINT('Ctrl Pts',(0.308371353328604,-0.277644141720387,
-2.37643253799337));
#48793=CARTESIAN_POINT('Ctrl Pts',(0.386362509757215,-0.151337939579646,
-2.36981014567899));
#48794=CARTESIAN_POINT('Ctrl Pts',(0.393377501689779,-0.0212056521456562,
-2.36318775336461));
#48795=CARTESIAN_POINT('Ctrl Pts',(0.400392493622343,0.108926635288333,
-2.35656536105023));
#48796=CARTESIAN_POINT('Ctrl Pts',(0.336431321058859,0.242885008015571,
-2.34994296873585));
#48797=CARTESIAN_POINT('Ctrl Pts',(0.230823258321736,0.319243107978586,
-2.34332057642147));
#48798=CARTESIAN_POINT('Ctrl Pts',(0.125215195584611,0.395601207941602,
-2.33669818410709));
#48799=CARTESIAN_POINT('Ctrl Pts',(-0.0220397573261533,0.414359035140395,
-2.33007579179271));
#48800=CARTESIAN_POINT('Ctrl Pts',(-0.143418120667098,0.366915223480943,
-2.32345339947833));
#48801=CARTESIAN_POINT('Ctrl Pts',(-0.264796484008043,0.319471411821491,
-2.31683100716395));
#48802=CARTESIAN_POINT('Ctrl Pts',(-0.360298257779167,0.205825961303794,
-2.31020861484957));
#48803=CARTESIAN_POINT('Ctrl Pts',(-0.386131284610396,0.0780907779253198,
-2.30358622253519));
#48804=CARTESIAN_POINT('Ctrl Pts',(-0.39129325438036,0.0525666626341382,
-2.30226293242462));
#48805=CARTESIAN_POINT('Ctrl Pts',(-0.393673472700586,0.0264799689052292,
-2.30093964231406));
#48806=CARTESIAN_POINT('Ctrl Pts',(-0.393432313413097,0.00034956597777247,
-2.2996163522035));
#48807=CARTESIAN_POINT('Origin',(0.,0.,-2.22));
#48808=CARTESIAN_POINT('',(-0.392657355902925,4.67015916158497E-5,-2.1562836477965));
#48809=CARTESIAN_POINT('',(-0.392653076767141,1.81848134072799E-5,-2.1746163522035));
#48810=CARTESIAN_POINT('',(-0.3933,-4.81653586104654E-17,-2.22));
#48811=CARTESIAN_POINT('Ctrl Pts',(-0.392657355902925,4.67015916158497E-5,
-2.1562836477965));
#48812=CARTESIAN_POINT('Ctrl Pts',(-0.392723854145937,0.0629185196199584,
-2.15945174283637));
#48813=CARTESIAN_POINT('Ctrl Pts',(-0.378505393622063,0.125761940444854,
-2.16261983787624));
#48814=CARTESIAN_POINT('Ctrl Pts',(-0.349841169009376,0.181126233397604,
-2.16578793291611));
#48815=CARTESIAN_POINT('Ctrl Pts',(-0.289923225139679,0.29685636886619,
-2.17241032523049));
#48816=CARTESIAN_POINT('Ctrl Pts',(-0.166884273336077,0.379906329935288,
-2.17903271754487));
#48817=CARTESIAN_POINT('Ctrl Pts',(-0.0371435918272561,0.392193714310694,
-2.18565510985925));
#48818=CARTESIAN_POINT('Ctrl Pts',(0.0925970896815651,0.404481098686101,
-2.19227750217363));
#48819=CARTESIAN_POINT('Ctrl Pts',(0.229039500895603,0.346005906367814,
-2.19889989448801));
#48820=CARTESIAN_POINT('Ctrl Pts',(0.309618232668553,0.243581826000877,
-2.20552228680239));
#48821=CARTESIAN_POINT('Ctrl Pts',(0.390196964441505,0.141157745633939,
-2.21214467911677));
#48822=CARTESIAN_POINT('Ctrl Pts',(0.414912016773367,-0.00521522278165044,
-2.21876707143115));
#48823=CARTESIAN_POINT('Ctrl Pts',(0.372430349245197,-0.128418031910157,
-2.22538946374554));
#48824=CARTESIAN_POINT('Ctrl Pts',(0.329948681717027,-0.251620841038662,
-2.23201185605992));
#48825=CARTESIAN_POINT('Ctrl Pts',(0.220270294328826,-0.351653490880085,
-2.23863424837429));
#48826=CARTESIAN_POINT('Ctrl Pts',(0.0936880038099836,-0.382646199380983,
-2.24525664068867));
#48827=CARTESIAN_POINT('Ctrl Pts',(-0.0328942867088593,-0.413638907881881,
-2.25187903300305));
#48828=CARTESIAN_POINT('Ctrl Pts',(-0.176380480358344,-0.375591675042255,
-2.25850142531744));
#48829=CARTESIAN_POINT('Ctrl Pts',(-0.270975254900737,-0.285950987392151,
-2.26512381763182));
#48830=CARTESIAN_POINT('Ctrl Pts',(-0.347918018104932,-0.213037845660076,
-2.27051042768671));
#48831=CARTESIAN_POINT('Ctrl Pts',(-0.392513788802351,-0.105990020856159,
-2.27589703774161));
#48832=CARTESIAN_POINT('Ctrl Pts',(-0.393484494376611,0.000340583921978138,
-2.2812836477965));
#48833=CARTESIAN_POINT('Ctrl Pts',(-0.393432313413097,0.00034956597777247,
-2.2996163522035));
#48834=CARTESIAN_POINT('Ctrl Pts',(-0.392466593423499,-0.104289374972686,
-2.29431724999968));
#48835=CARTESIAN_POINT('Ctrl Pts',(-0.349464615981463,-0.209629234065492,
-2.28901814779586));
#48836=CARTESIAN_POINT('Ctrl Pts',(-0.274724910660883,-0.282350424157676,
-2.28371904559205));
#48837=CARTESIAN_POINT('Ctrl Pts',(-0.181321229988805,-0.373231526622949,
-2.27709665327767));
#48838=CARTESIAN_POINT('Ctrl Pts',(-0.0383495887533156,-0.413168815314241,
-2.27047426096328));
#48839=CARTESIAN_POINT('Ctrl Pts',(0.0886306378313994,-0.383849122174911,
-2.2638518686489));
#48840=CARTESIAN_POINT('Ctrl Pts',(0.215610864416114,-0.35452942903558,
-2.25722947633452));
#48841=CARTESIAN_POINT('Ctrl Pts',(0.326599676350054,-0.255952754065626,
-2.25060708402015));
#48842=CARTESIAN_POINT('Ctrl Pts',(0.370703364216961,-0.133321244798174,
-2.24398469170577));
#48843=CARTESIAN_POINT('Ctrl Pts',(0.414807052083867,-0.0106897355307235,
-2.23736229939138));
#48844=CARTESIAN_POINT('Ctrl Pts',(0.392025615883743,0.135996608034224,
-2.230739907077));
#48845=CARTESIAN_POINT('Ctrl Pts',(0.312805440018932,0.239475040979098,
-2.22411751476262));
#48846=CARTESIAN_POINT('Ctrl Pts',(0.233585264154121,0.342953473923971,
-2.21749512244824));
#48847=CARTESIAN_POINT('Ctrl Pts',(0.0979263486246238,0.40322399624877,
-2.21087273013386));
#48848=CARTESIAN_POINT('Ctrl Pts',(-0.0319651678833566,0.392649674136003,
-2.20425033781948));
#48849=CARTESIAN_POINT('Ctrl Pts',(-0.161856684391337,0.382075352023237,
-2.1976279455051));
#48850=CARTESIAN_POINT('Ctrl Pts',(-0.285980801877801,0.300656185472903,
-2.19100555319072));
#48851=CARTESIAN_POINT('Ctrl Pts',(-0.347420641447049,0.185726779042249,
-2.18438316087634));
#48852=CARTESIAN_POINT('Ctrl Pts',(-0.377624789710302,0.129226878391847,
-2.18112755798539));
#48853=CARTESIAN_POINT('Ctrl Pts',(-0.392679669287032,0.0646283660230939,
-2.17787195509445));
#48854=CARTESIAN_POINT('Ctrl Pts',(-0.392653076767141,1.81848134072799E-5,
-2.1746163522035));
#48855=CARTESIAN_POINT('Origin',(0.,0.,-2.22));
#48856=CARTESIAN_POINT('',(-0.393312671622578,-0.000360778048017763,-2.0312836477965));
#48857=CARTESIAN_POINT('',(-0.393365397637326,-0.000357415208850981,-2.0496163522035));
#48858=CARTESIAN_POINT('',(-0.3933,-4.81653586104654E-17,-2.22));
#48859=CARTESIAN_POINT('Ctrl Pts',(-0.393312671622578,-0.000360778048017763,
-2.0312836477965));
#48860=CARTESIAN_POINT('Ctrl Pts',(-0.392382090476659,0.100433263636076,
-2.03638405561676));
#48861=CARTESIAN_POINT('Ctrl Pts',(-0.352868355048726,0.201875395553562,
-2.04148446343701));
#48862=CARTESIAN_POINT('Ctrl Pts',(-0.283060251797859,0.273993521475951,
-2.04658487125726));
#48863=CARTESIAN_POINT('Ctrl Pts',(-0.192421098470888,0.367632018566217,
-2.05320726357164));
#48864=CARTESIAN_POINT('Ctrl Pts',(-0.050710058864453,0.411834517909533,
-2.05982965588602));
#48865=CARTESIAN_POINT('Ctrl Pts',(0.0770915383084671,0.386332047182076,
-2.0664520482004));
#48866=CARTESIAN_POINT('Ctrl Pts',(0.204893135481385,0.360829576454619,
-2.07307444051478));
#48867=CARTESIAN_POINT('Ctrl Pts',(0.31878529022079,0.265622135656392,-2.07969683282916));
#48868=CARTESIAN_POINT('Ctrl Pts',(0.366542970761298,0.14436691637679,-2.08631922514355));
#48869=CARTESIAN_POINT('Ctrl Pts',(0.414300651301807,0.0231116970971894,
-2.09294161745793));
#48870=CARTESIAN_POINT('Ctrl Pts',(0.39592385764342,-0.124191300663785,
-2.09956400977231));
#48871=CARTESIAN_POINT('Ctrl Pts',(0.319839233699866,-0.229996566376417,
-2.10618640208669));
#48872=CARTESIAN_POINT('Ctrl Pts',(0.24375460975631,-0.335801832089051,
-2.11280879440107));
#48873=CARTESIAN_POINT('Ctrl Pts',(0.109962155527584,-0.40010936575334,
-2.11943118671545));
#48874=CARTESIAN_POINT('Ctrl Pts',(-0.020187852595031,-0.393431069650401,
-2.12605357902983));
#48875=CARTESIAN_POINT('Ctrl Pts',(-0.150337860717645,-0.386752773547463,
-2.13267597134421));
#48876=CARTESIAN_POINT('Ctrl Pts',(-0.276845422734146,-0.309088647677299,
-2.13929836365859));
#48877=CARTESIAN_POINT('Ctrl Pts',(-0.341700735774504,-0.196051429808179,
-2.14592075597297));
#48878=CARTESIAN_POINT('Ctrl Pts',(-0.375529829618191,-0.137090236470876,
-2.14937505324748));
#48879=CARTESIAN_POINT('Ctrl Pts',(-0.392584850281501,-0.0685048875892015,
-2.15282935052199));
#48880=CARTESIAN_POINT('Ctrl Pts',(-0.392657355902925,4.67015916158497E-5,
-2.1562836477965));
#48881=CARTESIAN_POINT('Ctrl Pts',(-0.392653076767141,1.81848134072799E-5,
-2.1746163522035));
#48882=CARTESIAN_POINT('Ctrl Pts',(-0.39262557604985,-0.0667985867737443,
-2.17124956278007));
#48883=CARTESIAN_POINT('Ctrl Pts',(-0.376468876623097,-0.133627837849165,
-2.16788277335663));
#48884=CARTESIAN_POINT('Ctrl Pts',(-0.344257961249291,-0.191525441321806,
-2.1645159839332));
#48885=CARTESIAN_POINT('Ctrl Pts',(-0.280899879830252,-0.305408608944229,
-2.15789359161882));
#48886=CARTESIAN_POINT('Ctrl Pts',(-0.155428155340142,-0.384735297878101,
-2.15127119930444));
#48887=CARTESIAN_POINT('Ctrl Pts',(-0.0253776093140804,-0.393130405212394,
-2.14464880699006));
#48888=CARTESIAN_POINT('Ctrl Pts',(0.104672936711982,-0.401525512546686,
-2.13802641467568));
#48889=CARTESIAN_POINT('Ctrl Pts',(0.239302304273997,-0.338989038281399,
-2.1314040223613));
#48890=CARTESIAN_POINT('Ctrl Pts',(0.31677645195751,-0.234196964203578,
-2.12478163004692));
#48891=CARTESIAN_POINT('Ctrl Pts',(0.394250599641022,-0.129404890125758,
-2.11815923773254));
#48892=CARTESIAN_POINT('Ctrl Pts',(0.414569527446035,0.0176427837645943,
-2.11153684541816));
#48893=CARTESIAN_POINT('Ctrl Pts',(0.368416029525569,0.13951762521486,-2.10491445310378));
#48894=CARTESIAN_POINT('Ctrl Pts',(0.322262531605102,0.261392466665128,
-2.0982920607894));
#48895=CARTESIAN_POINT('Ctrl Pts',(0.209636607959153,0.358094475675308,
-2.09166966847501));
#48896=CARTESIAN_POINT('Ctrl Pts',(0.0821826624843472,0.385281129234163,
-2.08504727616063));
#48897=CARTESIAN_POINT('Ctrl Pts',(-0.0452712829904564,0.412467782793019,
-2.07842488384625));
#48898=CARTESIAN_POINT('Ctrl Pts',(-0.187553250294117,0.370139080900551,
-2.07180249153187));
#48899=CARTESIAN_POINT('Ctrl Pts',(-0.27942011289984,0.27770476960976,-2.06518009921749));
#48900=CARTESIAN_POINT('Ctrl Pts',(-0.351387691014076,0.205292657891022,
-2.05999218354616));
#48901=CARTESIAN_POINT('Ctrl Pts',(-0.392415527723301,0.102130741981397,
-2.05480426787483));
#48902=CARTESIAN_POINT('Ctrl Pts',(-0.393365397637326,-0.000357415208850981,
-2.0496163522035));
#48903=CARTESIAN_POINT('Origin',(0.,0.,-2.22));
#48904=CARTESIAN_POINT('',(-0.393882499483816,0.000146440842145469,-1.9062836477965));
#48905=CARTESIAN_POINT('',(-0.393853641092568,0.000174899764659127,-1.9246163522035));
#48906=CARTESIAN_POINT('',(-0.3933,-4.81653586104654E-17,-2.22));
#48907=CARTESIAN_POINT('Ctrl Pts',(-0.393882499483816,0.000146440842145469,
-1.9062836477965));
#48908=CARTESIAN_POINT('Ctrl Pts',(-0.393921042941097,0.0082248682466142,
-1.90669397608276));
#48909=CARTESIAN_POINT('Ctrl Pts',(-0.393694085357014,0.0163010888479467,
-1.90710430436902));
#48910=CARTESIAN_POINT('Ctrl Pts',(-0.393194767449,0.0243604353283438,-1.90751463265527));
#48911=CARTESIAN_POINT('Ctrl Pts',(-0.385136149051954,0.154432272874696,
-1.91413702496965));
#48912=CARTESIAN_POINT('Ctrl Pts',(-0.306134336330414,0.280108815161806,
-1.92075941728403));
#48913=CARTESIAN_POINT('Ctrl Pts',(-0.192415460823864,0.343761321842059,
-1.92738180959842));
#48914=CARTESIAN_POINT('Ctrl Pts',(-0.0786965853173158,0.407413828522312,
-1.9340042019128));
#48915=CARTESIAN_POINT('Ctrl Pts',(0.069739352974242,0.409042299595711,
-1.94062659422718));
#48916=CARTESIAN_POINT('Ctrl Pts',(0.184827335787369,0.347900002736998,
-1.94724898654156));
#48917=CARTESIAN_POINT('Ctrl Pts',(0.299915318600494,0.286757705878285,
-1.95387137885594));
#48918=CARTESIAN_POINT('Ctrl Pts',(0.381655345935191,0.162844641087458,
-1.96049377117032));
#48919=CARTESIAN_POINT('Ctrl Pts',(0.392565683129179,0.0329809094474556,
-1.9671161634847));
#48920=CARTESIAN_POINT('Ctrl Pts',(0.403476020323167,-0.0968828221925501,
-1.97373855579908));
#48921=CARTESIAN_POINT('Ctrl Pts',(0.343556667376447,-0.232697220681733,
-1.98036094811346));
#48922=CARTESIAN_POINT('Ctrl Pts',(0.240283530054112,-0.312184850919123,
-1.98698334042784));
#48923=CARTESIAN_POINT('Ctrl Pts',(0.137010392731777,-0.391672481156512,
-1.99360573274222));
#48924=CARTESIAN_POINT('Ctrl Pts',(-0.00961652896617249,-0.414833343142106,
-2.0002281250566));
#48925=CARTESIAN_POINT('Ctrl Pts',(-0.132361737907768,-0.371047067495075,
-2.00685051737098));
#48926=CARTESIAN_POINT('Ctrl Pts',(-0.255106946849363,-0.327260791848045,
-2.01347290968536));
#48927=CARTESIAN_POINT('Ctrl Pts',(-0.353970443034605,-0.216527378568391,
-2.02009530199974));
#48928=CARTESIAN_POINT('Ctrl Pts',(-0.383618557603471,-0.0896234245099577,
-2.02671769431412));
#48929=CARTESIAN_POINT('Ctrl Pts',(-0.390432405003592,-0.0604578539500652,
-2.02823967880825));
#48930=CARTESIAN_POINT('Ctrl Pts',(-0.393590361196535,-0.030438170670314,
-2.02976166330238));
#48931=CARTESIAN_POINT('Ctrl Pts',(-0.393312671622578,-0.000360778048017763,
-2.0312836477965));
#48932=CARTESIAN_POINT('Ctrl Pts',(-0.393365397637326,-0.000357415208850981,
-2.0496163522035));
#48933=CARTESIAN_POINT('Ctrl Pts',(-0.393628039956887,-0.0286957454733452,
-2.04818187556045));
#48934=CARTESIAN_POINT('Ctrl Pts',(-0.390826554813069,-0.0569825640779221,
-2.0467473989174));
#48935=CARTESIAN_POINT('Ctrl Pts',(-0.384767761572825,-0.0845535818946124,
-2.04531292227435));
#48936=CARTESIAN_POINT('Ctrl Pts',(-0.356796789732301,-0.21183770141908,
-2.03869052995997));
#48937=CARTESIAN_POINT('Ctrl Pts',(-0.259403088143465,-0.323866019778899,
-2.03206813764559));
#48938=CARTESIAN_POINT('Ctrl Pts',(-0.137246354138968,-0.369268163849161,
-2.02544574533121));
#48939=CARTESIAN_POINT('Ctrl Pts',(-0.0150896201344695,-0.414670307919424,
-2.01882335301683));
#48940=CARTESIAN_POINT('Ctrl Pts',(0.13183014628569,-0.393446277700128,
-2.01220096070245));
#48941=CARTESIAN_POINT('Ctrl Pts',(0.236143164597026,-0.315328312035364,
-2.00557856838807));
#48942=CARTESIAN_POINT('Ctrl Pts',(0.340456182908363,-0.2372103463706,-1.99895617607369));
#48943=CARTESIAN_POINT('Ctrl Pts',(0.402162453110875,-0.102198445260367,
-1.99233378375931));
#48944=CARTESIAN_POINT('Ctrl Pts',(0.392966681917479,0.0277979398469947,
-1.98571139144493));
#48945=CARTESIAN_POINT('Ctrl Pts',(0.383770910724084,0.157794324954353,
-1.97908899913055));
#48946=CARTESIAN_POINT('Ctrl Pts',(0.303673098134783,0.282775194058841,
-1.97246660681617));
#48947=CARTESIAN_POINT('Ctrl Pts',(0.189401944351842,0.345430806432652,
-1.96584421450179));
#48948=CARTESIAN_POINT('Ctrl Pts',(0.0751307905688987,0.408086418806465,
-1.95922182218741));
#48949=CARTESIAN_POINT('Ctrl Pts',(-0.0733137044076861,0.4084167744496,
-1.95259942987303));
#48950=CARTESIAN_POINT('Ctrl Pts',(-0.187862598662765,0.34627038940782,
-1.94597703755865));
#48951=CARTESIAN_POINT('Ctrl Pts',(-0.302411492917843,0.28412400436604,
-1.93935464524427));
#48952=CARTESIAN_POINT('Ctrl Pts',(-0.383064786451416,0.159500878639347,
-1.93273225292988));
#48953=CARTESIAN_POINT('Ctrl Pts',(-0.392839064326688,0.0295467104074692,
-1.9261098606155));
#48954=CARTESIAN_POINT('Ctrl Pts',(-0.393573842411656,0.0197774490783411,
-1.92561202447817));
#48955=CARTESIAN_POINT('Ctrl Pts',(-0.393908066836798,0.00997806079885537,
-1.92511418834083));
#48956=CARTESIAN_POINT('Ctrl Pts',(-0.393853641092568,0.000174899764659127,
-1.9246163522035));
#48957=CARTESIAN_POINT('Origin',(0.,0.,-2.22));
#48958=CARTESIAN_POINT('',(-0.392871469582262,0.000278750737986277,-1.7812836477965));
#48959=CARTESIAN_POINT('',(-0.392835179244401,0.000259422774165058,-1.7996163522035));
#48960=CARTESIAN_POINT('',(-0.3933,-4.81653586104654E-17,-2.22));
#48961=CARTESIAN_POINT('Ctrl Pts',(-0.392871469582262,0.000278750737986277,
-1.7812836477965));
#48962=CARTESIAN_POINT('Ctrl Pts',(-0.39317461768958,0.0467057909606455,
-1.78362628886315));
#48963=CARTESIAN_POINT('Ctrl Pts',(-0.385570977921022,0.0930367504725677,
-1.78596892992979));
#48964=CARTESIAN_POINT('Ctrl Pts',(-0.369622026727067,0.136290547422904,
-1.78831157099643));
#48965=CARTESIAN_POINT('Ctrl Pts',(-0.324536070831699,0.258564341974944,
-1.79493396331081));
#48966=CARTESIAN_POINT('Ctrl Pts',(-0.212760094011492,0.356247558037995,
-1.80155635562519));
#48967=CARTESIAN_POINT('Ctrl Pts',(-0.085548758656478,0.3845477419658,-1.80817874793957));
#48968=CARTESIAN_POINT('Ctrl Pts',(0.0416625766985363,0.412847925893605,
-1.81480114025395));
#48969=CARTESIAN_POINT('Ctrl Pts',(0.184309270588358,0.371765077686166,
-1.82142353256833));
#48970=CARTESIAN_POINT('Ctrl Pts',(0.276980951801137,0.280137659549723,
-1.82804592488271));
#48971=CARTESIAN_POINT('Ctrl Pts',(0.369652633013916,0.188510241413279,
-1.83466831719709));
#48972=CARTESIAN_POINT('Ctrl Pts',(0.412349301549651,0.0463382533478326,
-1.84129070951147));
#48973=CARTESIAN_POINT('Ctrl Pts',(0.385492480948253,-0.0811856088911138,
-1.84791310182585));
#48974=CARTESIAN_POINT('Ctrl Pts',(0.358635660346854,-0.208709471130062,
-1.85453549414023));
#48975=CARTESIAN_POINT('Ctrl Pts',(0.262225350608317,-0.32158520754251,
-1.86115788645461));
#48976=CARTESIAN_POINT('Ctrl Pts',(0.140470316595559,-0.368053863061106,
-1.86778027876899));
#48977=CARTESIAN_POINT('Ctrl Pts',(0.0187152825828021,-0.414522518579702,
-1.87440267108337));
#48978=CARTESIAN_POINT('Ctrl Pts',(-0.128384475704176,-0.394584093204449,
-1.88102506339775));
#48979=CARTESIAN_POINT('Ctrl Pts',(-0.233376642811389,-0.317381314114025,
-1.88764745571213));
#48980=CARTESIAN_POINT('Ctrl Pts',(-0.331863418218086,-0.244962075855163,
-1.89385951974026));
#48981=CARTESIAN_POINT('Ctrl Pts',(-0.393298980305362,-0.122154921174261,
-1.90007158376838));
#48982=CARTESIAN_POINT('Ctrl Pts',(-0.393882499483816,0.000146440842145469,
-1.9062836477965));
#48983=CARTESIAN_POINT('Ctrl Pts',(-0.393853641092568,0.000174899764659127,
-1.9246163522035));
#48984=CARTESIAN_POINT('Ctrl Pts',(-0.393184076344219,-0.120427053295461,
-1.91849179602645));
#48985=CARTESIAN_POINT('Ctrl Pts',(-0.333693123404451,-0.241600004870103,
-1.91236723984941));
#48986=CARTESIAN_POINT('Ctrl Pts',(-0.237544312713443,-0.314274144743834,
-1.90624268367236));
#48987=CARTESIAN_POINT('Ctrl Pts',(-0.133580021007958,-0.392855620926195,
-1.89962029135798));
#48988=CARTESIAN_POINT('Ctrl Pts',(0.0132438246199847,-0.414733362553856,
-1.8929978990436));
#48989=CARTESIAN_POINT('Ctrl Pts',(0.135601427943425,-0.369875372654999,
-1.88637550672922));
#48990=CARTESIAN_POINT('Ctrl Pts',(0.257959031266865,-0.325017382756143,
-1.87975311441484));
#48991=CARTESIAN_POINT('Ctrl Pts',(0.355850392285805,-0.21342366133077,
-1.87313072210046));
#48992=CARTESIAN_POINT('Ctrl Pts',(0.384387612878835,-0.0862652979029292,
-1.86650832978608));
#48993=CARTESIAN_POINT('Ctrl Pts',(0.412924833471865,0.0408930655249115,
-1.8598859374717));
#48994=CARTESIAN_POINT('Ctrl Pts',(0.372107913638987,0.183616070955221,
-1.85326354515732));
#48995=CARTESIAN_POINT('Ctrl Pts',(0.280653374634137,0.276458354663846,
-1.84664115284294));
#48996=CARTESIAN_POINT('Ctrl Pts',(0.189198835629287,0.369300638372471,
-1.84001876052856));
#48997=CARTESIAN_POINT('Ctrl Pts',(0.0471066774524689,0.41226220035941,
-1.83339636821418));
#48998=CARTESIAN_POINT('Ctrl Pts',(-0.0804670099849952,0.385643097774413,
-1.8267739758998));
#48999=CARTESIAN_POINT('Ctrl Pts',(-0.20804069742246,0.359023995189416,
-1.82015158358542));
#49000=CARTESIAN_POINT('Ctrl Pts',(-0.321095914120569,0.26282422803248,
-1.81352919127104));
#49001=CARTESIAN_POINT('Ctrl Pts',(-0.36779140466704,0.141156017264642,
-1.80690679895666));
#49002=CARTESIAN_POINT('Ctrl Pts',(-0.38492675250312,0.0965087271794117,
-1.80447665003894));
#49003=CARTESIAN_POINT('Ctrl Pts',(-0.393126154036473,0.0484318773639158,
-1.80204650112122));
#49004=CARTESIAN_POINT('Ctrl Pts',(-0.392835179244401,0.000259422774165058,
-1.7996163522035));
#49005=CARTESIAN_POINT('Origin',(0.,0.,-2.22));
#49006=CARTESIAN_POINT('',(-0.392869409576936,-0.000277735283692127,-1.6562836477965));
#49007=CARTESIAN_POINT('',(-0.392908213753388,-0.000295413535636864,-1.6746163522035));
#49008=CARTESIAN_POINT('',(-0.3933,-4.81653586104654E-17,-2.22));
#49009=CARTESIAN_POINT('Ctrl Pts',(-0.392869409576936,-0.000277735283692127,
-1.6562836477965));
#49010=CARTESIAN_POINT('Ctrl Pts',(-0.39231841054015,0.0844454737480786,
-1.66055860164353));
#49011=CARTESIAN_POINT('Ctrl Pts',(-0.365440590195796,0.169487353070121,
-1.66483355549056));
#49012=CARTESIAN_POINT('Ctrl Pts',(-0.314887675254022,0.236730454170513,
-1.66910850933758));
#49013=CARTESIAN_POINT('Ctrl Pts',(-0.236575429704786,0.340897706463111,
-1.67573090165196));
#49014=CARTESIAN_POINT('Ctrl Pts',(-0.10144875175385,0.402352247389522,
-1.68235329396634));
#49015=CARTESIAN_POINT('Ctrl Pts',(0.0285302764476099,0.392914213645273,
-1.68897568628072));
#49016=CARTESIAN_POINT('Ctrl Pts',(0.158509304649072,0.383476179901023,
-1.6955980785951));
#49017=CARTESIAN_POINT('Ctrl Pts',(0.283340683101057,0.30314557148611,-1.70222047090948));
#49018=CARTESIAN_POINT('Ctrl Pts',(0.345783219731226,0.188757836687558,
-1.70884286322386));
#49019=CARTESIAN_POINT('Ctrl Pts',(0.408225756361394,0.0743701018890073,
-1.71546525553824));
#49020=CARTESIAN_POINT('Ctrl Pts',(0.408279451169747,-0.0740747592931836,
-1.72208764785262));
#49021=CARTESIAN_POINT('Ctrl Pts',(0.345919682503651,-0.188507637020978,
-1.728710040167));
#49022=CARTESIAN_POINT('Ctrl Pts',(0.283559913837555,-0.302940514748773,
-1.73533243248138));
#49023=CARTESIAN_POINT('Ctrl Pts',(0.15878668169701,-0.383361409022173,
-1.74195482479577));
#49024=CARTESIAN_POINT('Ctrl Pts',(0.0288145152734106,-0.392893471144811,
-1.74857721711015));
#49025=CARTESIAN_POINT('Ctrl Pts',(-0.101157651150189,-0.402425533267448,
-1.75519960942453));
#49026=CARTESIAN_POINT('Ctrl Pts',(-0.23632875185684,-0.341068763239323,
-1.7618220017389));
#49027=CARTESIAN_POINT('Ctrl Pts',(-0.314716334724902,-0.236958191704746,
-1.76844439405329));
#49028=CARTESIAN_POINT('Ctrl Pts',(-0.36537466779562,-0.169676259847524,
-1.77272414530102));
#49029=CARTESIAN_POINT('Ctrl Pts',(-0.392317650856458,-0.0845384182902281,
-1.77700389654876));
#49030=CARTESIAN_POINT('Ctrl Pts',(-0.392871469582262,0.000278750737986277,
-1.7812836477965));
#49031=CARTESIAN_POINT('Ctrl Pts',(-0.392835179244401,0.000259422774165058,
-1.7996163522035));
#49032=CARTESIAN_POINT('Ctrl Pts',(-0.392333219409033,-0.0828427497644315,
-1.79542410880684));
#49033=CARTESIAN_POINT('Ctrl Pts',(-0.366564232623453,-0.166229438361573,
-1.79123186541018));
#49034=CARTESIAN_POINT('Ctrl Pts',(-0.317815695830655,-0.232784711784617,
-1.78703962201352));
#49035=CARTESIAN_POINT('Ctrl Pts',(-0.240808732052964,-0.3379205756873,
-1.78041722969914));
#49036=CARTESIAN_POINT('Ctrl Pts',(-0.106459040102747,-0.401055649113928,
-1.77379483738475));
#49037=CARTESIAN_POINT('Ctrl Pts',(0.0236275833273017,-0.393239463766141,
-1.76717244507037));
#49038=CARTESIAN_POINT('Ctrl Pts',(0.153714206757352,-0.385423278418353,
-1.76055005275599));
#49039=CARTESIAN_POINT('Ctrl Pts',(0.279537761667233,-0.306655834296148,
-1.75392766044161));
#49040=CARTESIAN_POINT('Ctrl Pts',(0.343402095349705,-0.193055793661839,
-1.74730526812723));
#49041=CARTESIAN_POINT('Ctrl Pts',(0.407266429032176,-0.0794557530275321,
-1.74068287581285));
#49042=CARTESIAN_POINT('Ctrl Pts',(0.409171541487239,0.0689768841188778,
-1.73406048349847));
#49043=CARTESIAN_POINT('Ctrl Pts',(0.348243847008224,0.184178613247801,
-1.72743809118409));
#49044=CARTESIAN_POINT('Ctrl Pts',(0.287316152529208,0.299380342376726,
-1.72081569886971));
#49045=CARTESIAN_POINT('Ctrl Pts',(0.163555651116115,0.381351163488164,
-1.71419330655533));
#49046=CARTESIAN_POINT('Ctrl Pts',(0.033712486204077,0.392503511870799,
-1.70757091424095));
#49047=CARTESIAN_POINT('Ctrl Pts',(-0.0961306787079625,0.403655860253434,
-1.70094852192657));
#49048=CARTESIAN_POINT('Ctrl Pts',(-0.232056507118945,0.343989735907263,
-1.69432612961219));
#49049=CARTESIAN_POINT('Ctrl Pts',(-0.311736467948381,0.240864927102387,
-1.68770373729781));
#49050=CARTESIAN_POINT('Ctrl Pts',(-0.364225170025122,0.172932070337224,
-1.68334127559971));
#49051=CARTESIAN_POINT('Ctrl Pts',(-0.392306329059268,0.0861405888035373,
-1.6789788139016));
#49052=CARTESIAN_POINT('Ctrl Pts',(-0.392908213753388,-0.000295413535636864,
-1.6746163522035));
#49053=CARTESIAN_POINT('Origin',(0.,0.,-2.22));
#49054=CARTESIAN_POINT('',(-0.393881034687168,-0.000148036108369887,-1.5312836477965));
#49055=CARTESIAN_POINT('',(-0.393905480442768,-0.000118364692204371,-1.5496163522035));
#49056=CARTESIAN_POINT('',(-0.3933,-4.81653586104654E-17,-2.22));
#49057=CARTESIAN_POINT('Ctrl Pts',(-0.393881034687168,-0.000148036108369887,
-1.5312836477965));
#49058=CARTESIAN_POINT('Ctrl Pts',(-0.393292473280845,0.122060084085854,
-1.53749091442391));
#49059=CARTESIAN_POINT('Ctrl Pts',(-0.33196452645596,0.244777913826582,
-1.54369818105132));
#49060=CARTESIAN_POINT('Ctrl Pts',(-0.233606185198687,0.317212399183223,
-1.54990544767873));
#49061=CARTESIAN_POINT('Ctrl Pts',(-0.128669896443015,0.394491112651675,
-1.55652783999311));
#49062=CARTESIAN_POINT('Ctrl Pts',(0.0184153992780236,0.414535949323148,
-1.56315023230749));
#49063=CARTESIAN_POINT('Ctrl Pts',(0.140204018292651,0.368155387320699,
-1.56977262462187));
#49064=CARTESIAN_POINT('Ctrl Pts',(0.261992637307281,0.321774825318249,
-1.57639501693625));
#49065=CARTESIAN_POINT('Ctrl Pts',(0.358484579615499,0.208968864641871,
-1.58301740925064));
#49066=CARTESIAN_POINT('Ctrl Pts',(0.385433647894231,0.0814644648273466,
-1.58963980156502));
#49067=CARTESIAN_POINT('Ctrl Pts',(0.412382716172962,-0.0460399349871773,
-1.5962621938794));
#49068=CARTESIAN_POINT('Ctrl Pts',(0.36978891042221,-0.188242773939847,
-1.60288458619378));
#49069=CARTESIAN_POINT('Ctrl Pts',(0.277183539566904,-0.279937209659278,
-1.60950697850816));
#49070=CARTESIAN_POINT('Ctrl Pts',(0.184578168711598,-0.371631645378708,
-1.61612937082254));
#49071=CARTESIAN_POINT('Ctrl Pts',(0.0419612327517392,-0.412817677864899,
-1.62275176313692));
#49072=CARTESIAN_POINT('Ctrl Pts',(-0.0852705425432246,-0.384609529956089,
-1.6293741554513));
#49073=CARTESIAN_POINT('Ctrl Pts',(-0.21250231783819,-0.356401382047279,
-1.63599654776568));
#49074=CARTESIAN_POINT('Ctrl Pts',(-0.324348932468261,-0.258799053743466,
-1.64261894008006));
#49075=CARTESIAN_POINT('Ctrl Pts',(-0.369523333209527,-0.136557907762166,
-1.64924133239444));
#49076=CARTESIAN_POINT('Ctrl Pts',(-0.385536296653187,-0.0932271060295508,
-1.65158877086179));
#49077=CARTESIAN_POINT('Ctrl Pts',(-0.393171971050278,-0.0468004644348565,
-1.65393620932915));
#49078=CARTESIAN_POINT('Ctrl Pts',(-0.392869409576936,-0.000277735283692127,
-1.6562836477965));
#49079=CARTESIAN_POINT('Ctrl Pts',(-0.392908213753388,-0.000295413535636864,
-1.6746163522035));
#49080=CARTESIAN_POINT('Ctrl Pts',(-0.393220014232531,-0.0450727391726227,
-1.67235642158722));
#49081=CARTESIAN_POINT('Ctrl Pts',(-0.386157320865123,-0.089754666397697,
-1.67009649097095));
#49082=CARTESIAN_POINT('Ctrl Pts',(-0.371293088633588,-0.131669969582669,
-1.66783656035467));
#49083=CARTESIAN_POINT('Ctrl Pts',(-0.327735655241467,-0.254496564199282,
-1.66121416804029));
#49084=CARTESIAN_POINT('Ctrl Pts',(-0.217186695209332,-0.353566260168928,
-1.65459177572591));
#49085=CARTESIAN_POINT('Ctrl Pts',(-0.090338224703861,-0.383450836111131,
-1.64796938341153));
#49086=CARTESIAN_POINT('Ctrl Pts',(0.0365102458016081,-0.413335412053333,
-1.64134699109715));
#49087=CARTESIAN_POINT('Ctrl Pts',(0.179658226780413,-0.374034867968095,
-1.63472459878277));
#49088=CARTESIAN_POINT('Ctrl Pts',(0.273465482775833,-0.283570393883337,
-1.62810220646839));
#49089=CARTESIAN_POINT('Ctrl Pts',(0.367272738771253,-0.193105919798579,
-1.62147981415401));
#49090=CARTESIAN_POINT('Ctrl Pts',(0.411739269783289,-0.0514775157143005,
-1.61485742183963));
#49091=CARTESIAN_POINT('Ctrl Pts',(0.386475032266683,0.0763713820186354,
-1.60823502952524));
#49092=CARTESIAN_POINT('Ctrl Pts',(0.361210794750077,0.204220279751574,
-1.60161263721086));
#49093=CARTESIAN_POINT('Ctrl Pts',(0.266215788704827,0.318289671133168,
-1.59499024489648));
#49094=CARTESIAN_POINT('Ctrl Pts',(0.145049794166852,0.366273252871574,
-1.5883678525821));
#49095=CARTESIAN_POINT('Ctrl Pts',(0.0238837996288819,0.414256834609979,
-1.58174546026772));
#49096=CARTESIAN_POINT('Ctrl Pts',(-0.123453183401811,0.396154606705199,
-1.57512306795334));
#49097=CARTESIAN_POINT('Ctrl Pts',(-0.229400060514477,0.320267311464852,
-1.56850067563896));
#49098=CARTESIAN_POINT('Ctrl Pts',(-0.330105616220708,0.248134253403169,
-1.56220590116047));
#49099=CARTESIAN_POINT('Ctrl Pts',(-0.393415005972842,0.12379210044259,
-1.55591112668199));
#49100=CARTESIAN_POINT('Ctrl Pts',(-0.393905480442768,-0.000118364692204371,
-1.5496163522035));
#49101=CARTESIAN_POINT('Origin',(0.,0.,-2.22));
#49102=CARTESIAN_POINT('',(-0.393315558933435,0.000360657844753393,-1.4062836477965));
#49103=CARTESIAN_POINT('',(-0.393263050796212,0.000361685240310451,-1.4246163522035));
#49104=CARTESIAN_POINT('',(-0.3933,-4.81653586104654E-17,-2.22));
#49105=CARTESIAN_POINT('Ctrl Pts',(-0.393315558933435,0.000360657844753393,
-1.4062836477965));
#49106=CARTESIAN_POINT('Ctrl Pts',(-0.393592470507005,0.0303426814093579,
-1.40780083488992));
#49107=CARTESIAN_POINT('Ctrl Pts',(-0.390454628709984,0.0602673346706706,
-1.40931802198333));
#49108=CARTESIAN_POINT('Ctrl Pts',(-0.383683293576175,0.0893458795311712,
-1.41083520907674));
#49109=CARTESIAN_POINT('Ctrl Pts',(-0.354126993009887,0.216271248744692,
-1.41745760139113));
#49110=CARTESIAN_POINT('Ctrl Pts',(-0.255343630670031,0.327076153958157,
-1.42407999370551));
#49111=CARTESIAN_POINT('Ctrl Pts',(-0.132630130193656,0.370951215826925,
-1.43070238601989));
#49112=CARTESIAN_POINT('Ctrl Pts',(-0.00991662971728322,0.414826277695692,
-1.43732477833427));
#49113=CARTESIAN_POINT('Ctrl Pts',(0.13672700889561,0.391771496219764,-1.44394717064865));
#49114=CARTESIAN_POINT('Ctrl Pts',(0.24005762300338,0.312358597763255,-1.45056956296303));
#49115=CARTESIAN_POINT('Ctrl Pts',(0.343388237111154,0.232945699306743,
-1.45719195527741));
#49116=CARTESIAN_POINT('Ctrl Pts',(0.403405826713803,0.0971746838696504,
-1.46381434759179));
#49117=CARTESIAN_POINT('Ctrl Pts',(0.39258943981379,-0.0326969066633951,
-1.47043673990617));
#49118=CARTESIAN_POINT('Ctrl Pts',(0.381773052913776,-0.162568497196441,
-1.47705913222055));
#49119=CARTESIAN_POINT('Ctrl Pts',(0.300122689511095,-0.286540662825437,
-1.48368152453493));
#49120=CARTESIAN_POINT('Ctrl Pts',(0.185078969041886,-0.347766201890081,
-1.49030391684931));
#49121=CARTESIAN_POINT('Ctrl Pts',(0.0700352485726779,-0.408991740954724,
-1.49692630916369));
#49122=CARTESIAN_POINT('Ctrl Pts',(-0.0784018289630594,-0.407470653455019,
-1.50354870147807));
#49123=CARTESIAN_POINT('Ctrl Pts',(-0.192166722903624,-0.343900431181965,
-1.51017109379245));
#49124=CARTESIAN_POINT('Ctrl Pts',(-0.305931616844188,-0.280330208908911,
-1.51679348610683));
#49125=CARTESIAN_POINT('Ctrl Pts',(-0.385024327189582,-0.154710851862508,
-1.52341587842121));
#49126=CARTESIAN_POINT('Ctrl Pts',(-0.393177041467126,-0.0246448782065889,
-1.53003827073559));
#49127=CARTESIAN_POINT('Ctrl Pts',(-0.393688095623158,-0.0164916725216676,
-1.53045339642256));
#49128=CARTESIAN_POINT('Ctrl Pts',(-0.393920396128007,-0.00832099417415774,
-1.53086852210953));
#49129=CARTESIAN_POINT('Ctrl Pts',(-0.393881034687168,-0.000148036108369887,
-1.5312836477965));
#49130=CARTESIAN_POINT('Ctrl Pts',(-0.393905480442768,-0.000118364692204371,
-1.5496163522035));
#49131=CARTESIAN_POINT('Ctrl Pts',(-0.393931007677293,-0.00656740882723717,
-1.54928873436761));
#49132=CARTESIAN_POINT('Ctrl Pts',(-0.393786371902764,-0.0130152836122568,
-1.54896111653171));
#49133=CARTESIAN_POINT('Ctrl Pts',(-0.393467988982188,-0.0194545676714611,
-1.54863349869582));
#49134=CARTESIAN_POINT('Ctrl Pts',(-0.387032269142592,-0.149616788991508,
-1.54201110638144));
#49135=CARTESIAN_POINT('Ctrl Pts',(-0.309604058268761,-0.276268869055684,
-1.53538871406706));
#49136=CARTESIAN_POINT('Ctrl Pts',(-0.196687915754401,-0.341334736517045,
-1.52876632175268));
#49137=CARTESIAN_POINT('Ctrl Pts',(-0.0837717732400437,-0.406400603978403,
-1.5221439294383));
#49138=CARTESIAN_POINT('Ctrl Pts',(0.0646323009148415,-0.40988025883695,
-1.51552153712392));
#49139=CARTESIAN_POINT('Ctrl Pts',(0.180473899686314,-0.350178111950168,
-1.50889914480954));
#49140=CARTESIAN_POINT('Ctrl Pts',(0.29631549845779,-0.290475965063384,
-1.50227675249516));
#49141=CARTESIAN_POINT('Ctrl Pts',(0.379594621845851,-0.167592016431268,
-1.49565436018078));
#49142=CARTESIAN_POINT('Ctrl Pts',(0.392123785609061,-0.0378744678720334,
-1.4890319678664));
#49143=CARTESIAN_POINT('Ctrl Pts',(0.40465294937227,0.0918430806872008,
-1.48240957555202));
#49144=CARTESIAN_POINT('Ctrl Pts',(0.346432153510629,0.228394229173553,
-1.47578718323764));
#49145=CARTESIAN_POINT('Ctrl Pts',(0.244158433656106,0.30916370717076,-1.46916479092326));
#49146=CARTESIAN_POINT('Ctrl Pts',(0.141884713801586,0.389933185167965,
-1.46254239860888));
#49147=CARTESIAN_POINT('Ctrl Pts',(-0.00444193004581186,0.414920992676028,
-1.4559200062945));
#49148=CARTESIAN_POINT('Ctrl Pts',(-0.127723692593558,0.372669017906287,
-1.44929761398012));
#49149=CARTESIAN_POINT('Ctrl Pts',(-0.251005455141308,0.330417043136545,
-1.44267522166574));
#49150=CARTESIAN_POINT('Ctrl Pts',(-0.351242336389405,0.220925286088996,
-1.43605282935135));
#49151=CARTESIAN_POINT('Ctrl Pts',(-0.382470904359394,0.0944009845048089,
-1.42943043703697));
#49152=CARTESIAN_POINT('Ctrl Pts',(-0.390038007419168,0.0637424403610792,
-1.42782574209248));
#49153=CARTESIAN_POINT('Ctrl Pts',(-0.393553230514098,0.0320838163330584,
-1.42622104714799));
#49154=CARTESIAN_POINT('Ctrl Pts',(-0.393263050796212,0.000361685240310451,
-1.4246163522035));
#49155=CARTESIAN_POINT('Origin',(0.,0.,-2.22));
#49156=CARTESIAN_POINT('',(-0.392657025633087,-4.51440007200321E-5,-1.2812836477965));
#49157=CARTESIAN_POINT('',(-0.392664786614424,-7.33973318879278E-5,-1.2996163522035));
#49158=CARTESIAN_POINT('',(-0.3933,-4.81653586104654E-17,-2.22));
#49159=CARTESIAN_POINT('Ctrl Pts',(-0.392657025633087,-4.51440007200321E-5,
-1.2812836477965));
#49160=CARTESIAN_POINT('Ctrl Pts',(-0.392587038824807,0.0684113828747579,
-1.2847331476703));
#49161=CARTESIAN_POINT('Ctrl Pts',(-0.375581983361472,0.136900451219797,
-1.2881826475441));
#49162=CARTESIAN_POINT('Ctrl Pts',(-0.341842476026,0.195804181628159,-1.2916321474179));
#49163=CARTESIAN_POINT('Ctrl Pts',(-0.277068954575367,0.30888828825698,
-1.29825453973228));
#49164=CARTESIAN_POINT('Ctrl Pts',(-0.150617610293015,0.386643913286418,
-1.30487693204666));
#49165=CARTESIAN_POINT('Ctrl Pts',(-0.0204724675134631,0.393416362182065,
-1.31149932436104));
#49166=CARTESIAN_POINT('Ctrl Pts',(0.109672675266089,0.400188811077712,
-1.31812171667542));
#49167=CARTESIAN_POINT('Ctrl Pts',(0.243511616542838,0.335978083839568,
-1.3247441089898));
#49168=CARTESIAN_POINT('Ctrl Pts',(0.319672763377695,0.230227887783232,
-1.33136650130418));
#49169=CARTESIAN_POINT('Ctrl Pts',(0.39583391021255,0.124477691726897,-1.33798889361856));
#49170=CARTESIAN_POINT('Ctrl Pts',(0.414317262605513,-0.0228119731476319,
-1.34461128593294));
#49171=CARTESIAN_POINT('Ctrl Pts',(0.366647314337019,-0.144101710080452,
-1.35123367824732));
#49172=CARTESIAN_POINT('Ctrl Pts',(0.318977366068527,-0.265391447013271,
-1.3578560705617));
#49173=CARTESIAN_POINT('Ctrl Pts',(0.205154117138584,-0.360681256004386,
-1.36447846287608));
#49174=CARTESIAN_POINT('Ctrl Pts',(0.07737100268419,-0.386276175685614,
-1.37110085519046));
#49175=CARTESIAN_POINT('Ctrl Pts',(-0.0504121117702055,-0.411871095366841,
-1.37772324750484));
#49176=CARTESIAN_POINT('Ctrl Pts',(-0.192155091749049,-0.36777112573818,
-1.38434563981922));
#49177=CARTESIAN_POINT('Ctrl Pts',(-0.282861962342114,-0.27419822431706,
-1.3909680321336));
#49178=CARTESIAN_POINT('Ctrl Pts',(-0.352787929778942,-0.202062832422688,
-1.39607323735457));
#49179=CARTESIAN_POINT('Ctrl Pts',(-0.392383775096574,-0.100526295321156,
-1.40117844257554));
#49180=CARTESIAN_POINT('Ctrl Pts',(-0.393315558933435,0.000360657844753393,
-1.4062836477965));
#49181=CARTESIAN_POINT('Ctrl Pts',(-0.393263050796212,0.000361685240310451,
-1.4246163522035));
#49182=CARTESIAN_POINT('Ctrl Pts',(-0.392355692041059,-0.0988297868196482,
-1.41959865483361));
#49183=CARTESIAN_POINT('Ctrl Pts',(-0.354241338381814,-0.198642193679393,
-1.41458095746372));
#49184=CARTESIAN_POINT('Ctrl Pts',(-0.286455499065155,-0.270441834064746,
-1.40956326009383));
#49185=CARTESIAN_POINT('Ctrl Pts',(-0.196991271109047,-0.365203504929285,
-1.40294086777945));
#49186=CARTESIAN_POINT('Ctrl Pts',(-0.0558425605049488,-0.411170000537543,
-1.39631847546507));
#49187=CARTESIAN_POINT('Ctrl Pts',(0.0722671589327426,-0.387263471420634,
-1.38969608315069));
#49188=CARTESIAN_POINT('Ctrl Pts',(0.200376878370438,-0.363356942303724,
-1.38307369083631));
#49189=CARTESIAN_POINT('Ctrl Pts',(0.315447606641727,-0.269577388461642,
-1.37645129852193));
#49190=CARTESIAN_POINT('Ctrl Pts',(0.364713879321218,-0.148927246625453,
-1.36982890620755));
#49191=CARTESIAN_POINT('Ctrl Pts',(0.413980152000709,-0.0282771047892618,
-1.36320651389317));
#49192=CARTESIAN_POINT('Ctrl Pts',(0.397441969088403,0.119243625041034,
-1.35658412157879));
#49193=CARTESIAN_POINT('Ctrl Pts',(0.322682883023998,0.225989591707873,
-1.34996172926441));
#49194=CARTESIAN_POINT('Ctrl Pts',(0.247923796959597,0.332735558374708,
-1.34333933695003));
#49195=CARTESIAN_POINT('Ctrl Pts',(0.114943807743101,0.398706761878086,
-1.33671694463565));
#49196=CARTESIAN_POINT('Ctrl Pts',(-0.015279362526179,0.393652231846543,
-1.33009455232127));
#49197=CARTESIAN_POINT('Ctrl Pts',(-0.145502532795462,0.388597701814998,
-1.32347216000689));
#49198=CARTESIAN_POINT('Ctrl Pts',(-0.272968884117532,0.312517438248528,
-1.31684976769251));
#49199=CARTESIAN_POINT('Ctrl Pts',(-0.339228962602927,0.200297901856989,
-1.31022737537813));
#49200=CARTESIAN_POINT('Ctrl Pts',(-0.374618350354063,0.140361650989309,
-1.30669036765325));
#49201=CARTESIAN_POINT('Ctrl Pts',(-0.392547983298784,0.0701162796154407,
-1.30315335992837));
#49202=CARTESIAN_POINT('Ctrl Pts',(-0.392664786614424,-7.33973318879278E-5,
-1.2996163522035));
#49203=CARTESIAN_POINT('Origin',(0.,0.,-2.22));
#49204=CARTESIAN_POINT('',(-0.393481653172021,-0.000341139932622969,-1.1562836477965));
#49205=CARTESIAN_POINT('',(-0.393533012869392,-0.000329848589259697,-1.1746163522035));
#49206=CARTESIAN_POINT('',(-0.3933,-4.81653586104654E-17,-2.22));
#49207=CARTESIAN_POINT('Ctrl Pts',(-0.393481653172021,-0.000341139932622969,
-1.1562836477965));
#49208=CARTESIAN_POINT('Ctrl Pts',(-0.392511039428293,0.105896743864737,
-1.16166546045068));
#49209=CARTESIAN_POINT('Ctrl Pts',(-0.348003565773197,0.212851082423324,
-1.16704727310487));
#49210=CARTESIAN_POINT('Ctrl Pts',(-0.271182049778677,0.285754880687094,
-1.17242908575905));
#49211=CARTESIAN_POINT('Ctrl Pts',(-0.17665214883428,0.375463977665029,
-1.17905147807343));
#49212=CARTESIAN_POINT('Ctrl Pts',(-0.0331935172773672,0.413615002898312,
-1.18567387038781));
#49213=CARTESIAN_POINT('Ctrl Pts',(0.0934111612013362,0.382713876050605,
-1.19229626270219));
#49214=CARTESIAN_POINT('Ctrl Pts',(0.220015839680038,0.351812749202898,
-1.19891865501657));
#49215=CARTESIAN_POINT('Ctrl Pts',(0.329766565080531,0.251859470274202,
-1.20554104733095));
#49216=CARTESIAN_POINT('Ctrl Pts',(0.372337350214068,0.128687425936748,
-1.21216343964533));
#49217=CARTESIAN_POINT('Ctrl Pts',(0.414908135347607,0.00551538159929298,
-1.21878583195971));
#49218=CARTESIAN_POINT('Ctrl Pts',(0.390298980214189,-0.140875428146921,
-1.22540822427409));
#49219=CARTESIAN_POINT('Ctrl Pts',(0.309794366273512,-0.243357774858033,
-1.23203061658847));
#49220=CARTESIAN_POINT('Ctrl Pts',(0.229289752332836,-0.345840121569143,
-1.23865300890285));
#49221=CARTESIAN_POINT('Ctrl Pts',(0.0928896795849039,-0.404414005245154,
-1.24527540121723));
#49222=CARTESIAN_POINT('Ctrl Pts',(-0.0368598570476348,-0.392220482505807,
-1.25189779353161));
#49223=CARTESIAN_POINT('Ctrl Pts',(-0.166609393680174,-0.38002695976646,
-1.258520185846));
#49224=CARTESIAN_POINT('Ctrl Pts',(-0.289708394197319,-0.297066030611755,
-1.26514257816038));
#49225=CARTESIAN_POINT('Ctrl Pts',(-0.349710045146433,-0.181379271920303,
-1.27176497047476));
#49226=CARTESIAN_POINT('Ctrl Pts',(-0.378457780961706,-0.125951924112699,
-1.27493786291534));
#49227=CARTESIAN_POINT('Ctrl Pts',(-0.392721400360745,-0.0630122999880512,
-1.27811075535592));
#49228=CARTESIAN_POINT('Ctrl Pts',(-0.392657025633087,-4.51440007200321E-5,
-1.2812836477965));
#49229=CARTESIAN_POINT('Ctrl Pts',(-0.392664786614424,-7.33973318879278E-5,
-1.2996163522035));
#49230=CARTESIAN_POINT('Ctrl Pts',(-0.392766675888667,-0.0613008993450839,
-1.29653096761399));
#49231=CARTESIAN_POINT('Ctrl Pts',(-0.379314189765856,-0.122486021613986,
-1.29344558302449));
#49232=CARTESIAN_POINT('Ctrl Pts',(-0.352072966544274,-0.176748874920563,
-1.29036019843499));
#49233=CARTESIAN_POINT('Ctrl Pts',(-0.293603086351501,-0.293217306089983,
-1.28373780612061));
#49234=CARTESIAN_POINT('Ctrl Pts',(-0.171609520317232,-0.37779535921221,
-1.27711541380623));
#49235=CARTESIAN_POINT('Ctrl Pts',(-0.042032187006433,-0.39169992827728,
-1.27049302149184));
#49236=CARTESIAN_POINT('Ctrl Pts',(0.0875451463043619,-0.40560449734235,
-1.26387062917746));
#49237=CARTESIAN_POINT('Ctrl Pts',(0.224706246891688,-0.348835582350259,
-1.25724823686308));
#49238=CARTESIAN_POINT('Ctrl Pts',(0.306556151959042,-0.247424461711115,
-1.2506258445487));
#49239=CARTESIAN_POINT('Ctrl Pts',(0.388406057026397,-0.14601334107197,
-1.24400345223432));
#49240=CARTESIAN_POINT('Ctrl Pts',(0.414944766573788,3.99852142250606E-5,
-1.23738105991994));
#49241=CARTESIAN_POINT('Ctrl Pts',(0.374003005620899,0.123763041104785,
-1.23075866760556));
#49242=CARTESIAN_POINT('Ctrl Pts',(0.333061244668009,0.247486096995346,
-1.22413627529118));
#49243=CARTESIAN_POINT('Ctrl Pts',(0.224639013214835,0.348878882490268,
-1.2175138829768));
#49244=CARTESIAN_POINT('Ctrl Pts',(0.0984531200676662,0.381447927908793,
-1.21089149066242));
#49245=CARTESIAN_POINT('Ctrl Pts',(-0.0277327730795022,0.414016973327319,
-1.20426909834804));
#49246=CARTESIAN_POINT('Ctrl Pts',(-0.171682327920667,0.377762278669448,
-1.19764670603366));
#49247=CARTESIAN_POINT('Ctrl Pts',(-0.267387748823254,0.289308365479125,
-1.19102431371928));
#49248=CARTESIAN_POINT('Ctrl Pts',(-0.346429218455074,0.216255791995698,
-1.18555499321402));
#49249=CARTESIAN_POINT('Ctrl Pts',(-0.392564206260852,0.107599042506983,
-1.18008567270876));
#49250=CARTESIAN_POINT('Ctrl Pts',(-0.393533012869392,-0.000329848589259697,
-1.1746163522035));
#49251=CARTESIAN_POINT('Origin',(0.,0.,-2.22));
#49252=CARTESIAN_POINT('',(-0.393775421980258,0.000232396782078516,-1.0312836477965));
#49253=CARTESIAN_POINT('',(-0.393734572290504,0.000255441356017315,-1.0496163522035));
#49254=CARTESIAN_POINT('',(-0.3933,-4.81653586104654E-17,-2.22));
#49255=CARTESIAN_POINT('Ctrl Pts',(-0.393775421980258,0.000232396782078516,
-1.0312836477965));
#49256=CARTESIAN_POINT('Ctrl Pts',(-0.393870807162874,0.0138608314386894,
-1.03197538091669));
#49257=CARTESIAN_POINT('Ctrl Pts',(-0.393224744870318,0.0274801192648313,
-1.03266711403687));
#49258=CARTESIAN_POINT('Ctrl Pts',(-0.391807383245153,0.0410186590863903,
-1.03335884715706));
#49259=CARTESIAN_POINT('Ctrl Pts',(-0.3782380969709,0.170631539322734,-1.03998123947144));
#49260=CARTESIAN_POINT('Ctrl Pts',(-0.29397593879586,0.292843520708426,
-1.04660363178582));
#49261=CARTESIAN_POINT('Ctrl Pts',(-0.177659161700493,0.351614530732929,
-1.0532260241002));
#49262=CARTESIAN_POINT('Ctrl Pts',(-0.0613423846051261,0.410385540757432,
-1.05984841641458));
#49263=CARTESIAN_POINT('Ctrl Pts',(0.0870290114105677,0.405715579420747,
-1.06647080872896));
#49264=CARTESIAN_POINT('Ctrl Pts',(0.199419603821458,0.33974604864568,-1.07309320104334));
#49265=CARTESIAN_POINT('Ctrl Pts',(0.311810196232349,0.273776517870612,
-1.07971559335772));
#49266=CARTESIAN_POINT('Ctrl Pts',(0.388219985038436,0.146507417657162,
-1.0863379856721));
#49267=CARTESIAN_POINT('Ctrl Pts',(0.393611406355585,0.0162977527726593,
-1.09296037798648));
#49268=CARTESIAN_POINT('Ctrl Pts',(0.399002827672734,-0.113911912111845,
-1.09958277030087));
#49269=CARTESIAN_POINT('Ctrl Pts',(0.333375881500942,-0.247062141667403,
-1.10620516261525));
#49270=CARTESIAN_POINT('Ctrl Pts',(0.226823679664539,-0.322097150409778,
-1.11282755492963));
#49271=CARTESIAN_POINT('Ctrl Pts',(0.120271477828136,-0.397132159152151,
-1.11944994724401));
#49272=CARTESIAN_POINT('Ctrl Pts',(-0.0272059796728769,-0.414051947081344,
-1.12607233955839));
#49273=CARTESIAN_POINT('Ctrl Pts',(-0.147983184125541,-0.365097977500186,
-1.13269473187277));
#49274=CARTESIAN_POINT('Ctrl Pts',(-0.268760388578204,-0.316144007919027,
-1.13931712418715));
#49275=CARTESIAN_POINT('Ctrl Pts',(-0.362837339982519,-0.201316280827518,
-1.14593951650153));
#49276=CARTESIAN_POINT('Ctrl Pts',(-0.387075230518735,-0.0732688329204707,
-1.15256190881591));
#49277=CARTESIAN_POINT('Ctrl Pts',(-0.391615739835896,-0.0492815709352832,
-1.15380248847611));
#49278=CARTESIAN_POINT('Ctrl Pts',(-0.39370539259696,-0.0248303903488462,
-1.1550430681363));
#49279=CARTESIAN_POINT('Ctrl Pts',(-0.393481653172021,-0.000341139932622969,
-1.1562836477965));
#49280=CARTESIAN_POINT('Ctrl Pts',(-0.393533012869392,-0.000329848589259697,
-1.1746163522035));
#49281=CARTESIAN_POINT('Ctrl Pts',(-0.393737261932456,-0.0230840027100406,
-1.17346328039438));
#49282=CARTESIAN_POINT('Ctrl Pts',(-0.391933993525686,-0.045805805447558,
-1.17231020858526));
#49283=CARTESIAN_POINT('Ctrl Pts',(-0.388008326502387,-0.0681548026318557,
-1.17115713677614));
#49284=CARTESIAN_POINT('Ctrl Pts',(-0.365462196314924,-0.196510925829749,
-1.16453474446176));
#49285=CARTESIAN_POINT('Ctrl Pts',(-0.272908648975983,-0.312570040502759,
-1.15791235214738));
#49286=CARTESIAN_POINT('Ctrl Pts',(-0.152787938257515,-0.363113459513673,
-1.151289959833));
#49287=CARTESIAN_POINT('Ctrl Pts',(-0.0326672275390472,-0.413656878524587,
-1.14466756751862));
#49288=CARTESIAN_POINT('Ctrl Pts',(0.115020646558947,-0.398684601873405,
-1.13804517520424));
#49289=CARTESIAN_POINT('Ctrl Pts',(0.222553689191635,-0.325062138650695,
-1.13142278288986));
#49290=CARTESIAN_POINT('Ctrl Pts',(0.330086731824319,-0.251439675427988,
-1.12480039057547));
#49291=CARTESIAN_POINT('Ctrl Pts',(0.3974649429917,-0.119167025633755,-1.11817799826109));
#49292=CARTESIAN_POINT('Ctrl Pts',(0.393792171623827,0.0111024377845789,
-1.11155560594671));
#49293=CARTESIAN_POINT('Ctrl Pts',(0.390119400255954,0.141371901202919,
-1.10493321363233));
#49294=CARTESIAN_POINT('Ctrl Pts',(0.315395646352824,0.269638178245362,
-1.09831082131795));
#49295=CARTESIAN_POINT('Ctrl Pts',(0.203885345688334,0.337085010598986,
-1.09168842900357));
#49296=CARTESIAN_POINT('Ctrl Pts',(0.092375045023848,0.404531842952609,
-1.08506603668919));
#49297=CARTESIAN_POINT('Ctrl Pts',(-0.0559218024019938,0.411159230617415,
-1.07844364437481));
#49298=CARTESIAN_POINT('Ctrl Pts',(-0.173003958178694,0.353928197536556,
-1.07182125206043));
#49299=CARTESIAN_POINT('Ctrl Pts',(-0.290086113955397,0.296697164455695,
-1.06519885974605));
#49300=CARTESIAN_POINT('Ctrl Pts',(-0.375953578082954,0.175607710629166,
-1.05857646743167));
#49301=CARTESIAN_POINT('Ctrl Pts',(-0.391231987577939,0.0461851756820929,
-1.05195407511729));
#49302=CARTESIAN_POINT('Ctrl Pts',(-0.393029761265915,0.0309563373638524,
-1.05117483414603));
#49303=CARTESIAN_POINT('Ctrl Pts',(-0.39385018271193,0.0156121220150227,
-1.05039559317476));
#49304=CARTESIAN_POINT('Ctrl Pts',(-0.393734572290504,0.000255441356017315,
-1.0496163522035));
#49305=CARTESIAN_POINT('Origin',(0.,0.,-2.22));
#49306=CARTESIAN_POINT('',(-0.392765335323044,0.000211032987566279,-0.906283647796502));
#49307=CARTESIAN_POINT('',(-0.392738865073111,0.000187005706935053,-0.924616352203497));
#49308=CARTESIAN_POINT('',(-0.3933,-4.81653586104654E-17,-2.22));
#49309=CARTESIAN_POINT('Ctrl Pts',(-0.392765335323044,0.000211032987566279,
-0.906283647796502));
#49310=CARTESIAN_POINT('Ctrl Pts',(-0.393018178513626,0.0522502699719019,
-0.908907693697072));
#49311=CARTESIAN_POINT('Ctrl Pts',(-0.383411587472077,0.104199912603151,
-0.911531739597643));
#49312=CARTESIAN_POINT('Ctrl Pts',(-0.363507551178323,0.151848003592403,
-0.914155785498213));
#49313=CARTESIAN_POINT('Ctrl Pts',(-0.313275069746406,0.272099082848873,
-0.920778177812594));
#49314=CARTESIAN_POINT('Ctrl Pts',(-0.197455787633044,0.364952588896186,
-0.927400570126975));
#49315=CARTESIAN_POINT('Ctrl Pts',(-0.0691584172096336,0.387830722464993,
-0.934022962441355));
#49316=CARTESIAN_POINT('Ctrl Pts',(0.0591389532137729,0.410708856033799,
-0.940645354755735));
#49317=CARTESIAN_POINT('Ctrl Pts',(0.199914411947228,0.363611617124105,
-0.947267747070115));
#49318=CARTESIAN_POINT('Ctrl Pts',(0.288615639114422,0.268135355403262,
-0.953890139384496));
#49319=CARTESIAN_POINT('Ctrl Pts',(0.377316866281618,0.172659093682417,
-0.960512531698877));
#49320=CARTESIAN_POINT('Ctrl Pts',(0.41394386188255,0.028803809150419,-0.967134924013258));
#49321=CARTESIAN_POINT('Ctrl Pts',(0.38170138648123,-0.0974659300318142,
-0.973757316327638));
#49322=CARTESIAN_POINT('Ctrl Pts',(0.349458911079909,-0.223735669214047,
-0.980379708642019));
#49323=CARTESIAN_POINT('Ctrl Pts',(0.24834696467634,-0.332419863046513,
-0.987002100956397));
#49324=CARTESIAN_POINT('Ctrl Pts',(0.124730238718036,-0.373681580370242,
-0.993624493270778));
#49325=CARTESIAN_POINT('Ctrl Pts',(0.00111351275973311,-0.414943297693971,
-1.00024688558516));
#49326=CARTESIAN_POINT('Ctrl Pts',(-0.145007992753303,-0.388782538508961,
-1.00686927789954));
#49327=CARTESIAN_POINT('Ctrl Pts',(-0.246630538323087,-0.307195269372958,
-1.01349167021392));
#49328=CARTESIAN_POINT('Ctrl Pts',(-0.337638236992966,-0.234130089169133,
-1.01942232940811));
#49329=CARTESIAN_POINT('Ctrl Pts',(-0.392957625356443,-0.116612668084744,
-1.02535298860231));
#49330=CARTESIAN_POINT('Ctrl Pts',(-0.393775421980258,0.000232396782078516,
-1.0312836477965));
#49331=CARTESIAN_POINT('Ctrl Pts',(-0.393734572290504,0.000255441356017315,
-1.0496163522035));
#49332=CARTESIAN_POINT('Ctrl Pts',(-0.392867665628586,-0.114896883184711,
-1.04377320086038));
#49333=CARTESIAN_POINT('Ctrl Pts',(-0.33936979228434,-0.230750104080959,
-1.03793004951726));
#49334=CARTESIAN_POINT('Ctrl Pts',(-0.250662643696462,-0.303914095777196,
-1.03208689817415));
#49335=CARTESIAN_POINT('Ctrl Pts',(-0.150125535457593,-0.386835216221796,
-1.02546450585977));
#49336=CARTESIAN_POINT('Ctrl Pts',(-0.00436196411744454,-0.414921841043383,
-1.01884211354539));
#49337=CARTESIAN_POINT('Ctrl Pts',(0.119788460862806,-0.37529490164548,
-1.01221972123101));
#49338=CARTESIAN_POINT('Ctrl Pts',(0.243938885843059,-0.335667962247576,
-1.00559732891663));
#49339=CARTESIAN_POINT('Ctrl Pts',(0.346476164463412,-0.228327458630178,
-0.998974936602248));
#49340=CARTESIAN_POINT('Ctrl Pts',(0.380382021888903,-0.102494175350018,
-0.992352544287867));
#49341=CARTESIAN_POINT('Ctrl Pts',(0.414287879314394,0.0233391079301406,
-0.985730151973486));
#49342=CARTESIAN_POINT('Ctrl Pts',(0.379562315545022,0.167665170873064,
-0.979107759659106));
#49343=CARTESIAN_POINT('Ctrl Pts',(0.292128672053041,0.264303570769479,
-0.972485367344726));
#49344=CARTESIAN_POINT('Ctrl Pts',(0.204695028561061,0.360941970665893,
-0.965862975030346));
#49345=CARTESIAN_POINT('Ctrl Pts',(0.0645533053464747,0.409892707515805,
-0.959240582715966));
#49346=CARTESIAN_POINT('Ctrl Pts',(-0.064034775935856,0.388709513683181,
-0.952618190401585));
#49347=CARTESIAN_POINT('Ctrl Pts',(-0.19262285721819,0.367526319850557,
-0.945995798087205));
#49348=CARTESIAN_POINT('Ctrl Pts',(-0.309657296568267,0.276209195335393,
-0.939373405772824));
#49349=CARTESIAN_POINT('Ctrl Pts',(-0.361472173566141,0.156631434566436,
-0.932751013458443));
#49350=CARTESIAN_POINT('Ctrl Pts',(-0.382687894025607,0.107670045625049,
-0.930039459706794));
#49351=CARTESIAN_POINT('Ctrl Pts',(-0.39296947761259,0.0539707275446464,
-0.927327905955146));
#49352=CARTESIAN_POINT('Ctrl Pts',(-0.392738865073111,0.000187005706935053,
-0.924616352203497));
#49353=CARTESIAN_POINT('Origin',(0.,0.,-2.22));
#49354=CARTESIAN_POINT('',(-0.393002927928462,-0.000327777057962136,-0.781283647796501));
#49355=CARTESIAN_POINT('',(-0.39304905505562,-0.000339067021170478,-0.799616352203498));
#49356=CARTESIAN_POINT('',(-0.3933,-4.81653586104654E-17,-2.22));
#49357=CARTESIAN_POINT('Ctrl Pts',(-0.393002927928462,-0.000327777057962136,
-0.781283647796501));
#49358=CARTESIAN_POINT('Ctrl Pts',(-0.392293971122862,0.0898952132304527,
-0.785840006477456));
#49359=CARTESIAN_POINT('Ctrl Pts',(-0.36143409706416,0.180556321363059,
-0.790396365158411));
#49360=CARTESIAN_POINT('Ctrl Pts',(-0.304561599573614,0.249875545069579,
-0.794952723839366));
#49361=CARTESIAN_POINT('Ctrl Pts',(-0.221900857377157,0.350626852518592,
-0.801575116153747));
#49362=CARTESIAN_POINT('Ctrl Pts',(-0.084288791991676,0.406293711194743,
-0.808197508468127));
#49363=CARTESIAN_POINT('Ctrl Pts',(0.0451728447326011,0.391350188523557,
-0.814819900782507));
#49364=CARTESIAN_POINT('Ctrl Pts',(0.17463448145688,0.37640666585237,-0.821442293096888));
#49365=CARTESIAN_POINT('Ctrl Pts',(0.295945689519953,0.290852761833842,
-0.828064685411268));
#49366=CARTESIAN_POINT('Ctrl Pts',(0.353479444311675,0.173919057057502,
-0.834687077725648));
#49367=CARTESIAN_POINT('Ctrl Pts',(0.411013199103396,0.056985352281164,
-0.841309470040029));
#49368=CARTESIAN_POINT('Ctrl Pts',(0.404769500623766,-0.0913281532529836,
-0.847931862354409));
#49369=CARTESIAN_POINT('Ctrl Pts',(0.33761138498075,-0.203012582590438,
-0.85455425466879));
#49370=CARTESIAN_POINT('Ctrl Pts',(0.270453269337734,-0.314697011927891,
-0.86117664698317));
#49371=CARTESIAN_POINT('Ctrl Pts',(0.142380736531329,-0.389752365068654,
-0.867799039297551));
#49372=CARTESIAN_POINT('Ctrl Pts',(0.0121212038221099,-0.393762152036687,
-0.874421431611931));
#49373=CARTESIAN_POINT('Ctrl Pts',(-0.118138328887113,-0.397771939004719,
-0.881043823926311));
#49374=CARTESIAN_POINT('Ctrl Pts',(-0.250584861499151,-0.330736159800021,
-0.887666216240692));
#49375=CARTESIAN_POINT('Ctrl Pts',(-0.324485287429933,-0.223393943964857,
-0.894288608555073));
#49376=CARTESIAN_POINT('Ctrl Pts',(-0.369103529444641,-0.15858483218769,
-0.898286954968882));
#49377=CARTESIAN_POINT('Ctrl Pts',(-0.39238006970551,-0.0790828911501493,
-0.902285301382692));
#49378=CARTESIAN_POINT('Ctrl Pts',(-0.392765335323044,0.000211032987566279,
-0.906283647796502));
#49379=CARTESIAN_POINT('Ctrl Pts',(-0.392738865073111,0.000187005706935053,
-0.924616352203497));
#49380=CARTESIAN_POINT('Ctrl Pts',(-0.392406255619253,-0.0773845538766605,
-0.920705513640765));
#49381=CARTESIAN_POINT('Ctrl Pts',(-0.370206263908016,-0.155131689448642,
-0.916794675078034));
#49382=CARTESIAN_POINT('Ctrl Pts',(-0.327404810574654,-0.219092739655027,
-0.912883836515302));
#49383=CARTESIAN_POINT('Ctrl Pts',(-0.254927255939623,-0.32740075608478,
-0.906261444200922));
#49384=CARTESIAN_POINT('Ctrl Pts',(-0.123376832023891,-0.396178391921544,
-0.899639051886542));
#49385=CARTESIAN_POINT('Ctrl Pts',(0.0069242635333148,-0.393887792564699,
-0.893016659572162));
#49386=CARTESIAN_POINT('Ctrl Pts',(0.137225359090526,-0.391597193207854,
-0.886394267257781));
#49387=CARTESIAN_POINT('Ctrl Pts',(0.266277126289207,-0.318238358657399,
-0.8797718749434));
#49388=CARTESIAN_POINT('Ctrl Pts',(0.334903121793558,-0.207449843504157,
-0.87314948262902));
#49389=CARTESIAN_POINT('Ctrl Pts',(0.403529117297906,-0.0966613283509224,
-0.86652709031464));
#49390=CARTESIAN_POINT('Ctrl Pts',(0.411729341107924,0.0515568674050974,
-0.85990469800026));
#49391=CARTESIAN_POINT('Ctrl Pts',(0.355743596132414,0.169239570927571,
-0.85328230568588));
#49392=CARTESIAN_POINT('Ctrl Pts',(0.299757851156902,0.28692227445005,-0.846659913371499));
#49393=CARTESIAN_POINT('Ctrl Pts',(0.179586137395857,0.374069485738985,
-0.840037521057118));
#49394=CARTESIAN_POINT('Ctrl Pts',(0.0503329665062123,0.390720016174824,
-0.833415128742737));
#49395=CARTESIAN_POINT('Ctrl Pts',(-0.0789202043834344,0.407370546610663,
-0.826792736428357));
#49396=CARTESIAN_POINT('Ctrl Pts',(-0.217254832401677,0.353524396193406,
-0.820170344113977));
#49397=CARTESIAN_POINT('Ctrl Pts',(-0.301237835972056,0.253872615175097,
-0.813547951799596));
#49398=CARTESIAN_POINT('Ctrl Pts',(-0.36012982560746,0.183993099018452,
-0.808904085267564));
#49399=CARTESIAN_POINT('Ctrl Pts',(-0.39229530980714,0.0915894274629187,
-0.804260218735531));
#49400=CARTESIAN_POINT('Ctrl Pts',(-0.39304905505562,-0.000339067021170478,
-0.799616352203498));
#49401=CARTESIAN_POINT('Origin',(0.,0.,-2.22));
#49402=CARTESIAN_POINT('',(-0.393941093179356,-4.92117729247177E-5,-0.656283647796501));
#49403=CARTESIAN_POINT('',(-0.393947723570607,-1.70646636204014E-5,-0.674616352203497));
#49404=CARTESIAN_POINT('',(-0.3933,-4.81653586104654E-17,-2.22));
#49405=CARTESIAN_POINT('Ctrl Pts',(-0.393941093179356,-4.92117729247177E-5,
-0.656283647796501));
#49406=CARTESIAN_POINT('Ctrl Pts',(-0.393716310075701,0.12764716684489,
-0.662772319257841));
#49407=CARTESIAN_POINT('Ctrl Pts',(-0.325876029158443,0.255548516106423,
-0.66926099071918));
#49408=CARTESIAN_POINT('Ctrl Pts',(-0.219939066679139,0.326836905668438,
-0.675749662180519));
#49409=CARTESIAN_POINT('Ctrl Pts',(-0.1118189175374,0.399594431758779,-0.6823720544949));
#49410=CARTESIAN_POINT('Ctrl Pts',(0.035984312963528,0.41338155429621,-0.68899444680928));
#49411=CARTESIAN_POINT('Ctrl Pts',(0.155695733519729,0.361876214363877,
-0.69561683912366));
#49412=CARTESIAN_POINT('Ctrl Pts',(0.275407154075931,0.310370874431544,
-0.702239231438041));
#49413=CARTESIAN_POINT('Ctrl Pts',(0.367026764687403,0.193573072029449,
-0.708861623752421));
#49414=CARTESIAN_POINT('Ctrl Pts',(0.388542566498581,0.0650402181532038,
-0.715484016066801));
#49415=CARTESIAN_POINT('Ctrl Pts',(0.410058368309758,-0.0634926357230411,
-0.722106408381182));
#49416=CARTESIAN_POINT('Ctrl Pts',(0.361470361320636,-0.203760541073438,
-0.728728800695563));
#49417=CARTESIAN_POINT('Ctrl Pts',(0.265058484077097,-0.291443915663717,
-0.735351193009943));
#49418=CARTESIAN_POINT('Ctrl Pts',(0.168646606833558,-0.379127290253996,
-0.741973585324323));
#49419=CARTESIAN_POINT('Ctrl Pts',(0.0244108593356022,-0.414226134084162,
-0.748595977638704));
#49420=CARTESIAN_POINT('Ctrl Pts',(-0.101509729683807,-0.380645938817388,
-0.755218369953084));
#49421=CARTESIAN_POINT('Ctrl Pts',(-0.227430318703216,-0.347065743550613,
-0.761840762267464));
#49422=CARTESIAN_POINT('Ctrl Pts',(-0.335035749244076,-0.244806509186898,
-0.768463154581844));
#49423=CARTESIAN_POINT('Ctrl Pts',(-0.37498375501079,-0.120759013894103,
-0.775085546896225));
#49424=CARTESIAN_POINT('Ctrl Pts',(-0.387446611269409,-0.0820590569524739,
-0.77715158052965));
#49425=CARTESIAN_POINT('Ctrl Pts',(-0.393324397046145,-0.0412384571638166,
-0.779217614163076));
#49426=CARTESIAN_POINT('Ctrl Pts',(-0.393002927928462,-0.000327777057962136,
-0.781283647796501));
#49427=CARTESIAN_POINT('Ctrl Pts',(-0.39304905505562,-0.000339067021170478,
-0.799616352203498));
#49428=CARTESIAN_POINT('Ctrl Pts',(-0.393370189265045,-0.0395053297064864,
-0.797637826421151));
#49429=CARTESIAN_POINT('Ctrl Pts',(-0.387989471362798,-0.0785853383517939,
-0.795659300638803));
#49430=CARTESIAN_POINT('Ctrl Pts',(-0.376544560585247,-0.115800399181673,
-0.793680774856456));
#49431=CARTESIAN_POINT('Ctrl Pts',(-0.338236902505551,-0.240364220900791,
-0.787058382542075));
#49432=CARTESIAN_POINT('Ctrl Pts',(-0.231990207223642,-0.344034452719668,
-0.780435990227694));
#49433=CARTESIAN_POINT('Ctrl Pts',(-0.106523695556455,-0.379273306260755,
-0.773813597913313));
#49434=CARTESIAN_POINT('Ctrl Pts',(0.0189428161107277,-0.414512159801841,
-0.767191205598933));
#49435=CARTESIAN_POINT('Ctrl Pts',(0.163629144163188,-0.381319635065142,
-0.760568813284553));
#49436=CARTESIAN_POINT('Ctrl Pts',(0.261189647008292,-0.294916101379107,
-0.753946420970173));
#49437=CARTESIAN_POINT('Ctrl Pts',(0.358750149853395,-0.208512567693073,
-0.747324028655793));
#49438=CARTESIAN_POINT('Ctrl Pts',(0.409184827491143,-0.068898025057705,
-0.740701636341412));
#49439=CARTESIAN_POINT('Ctrl Pts',(0.389366954048811,0.0599075425278824,
-0.734079244027032));
#49440=CARTESIAN_POINT('Ctrl Pts',(0.369549080606479,0.188713110113473,
-0.727456851712651));
#49441=CARTESIAN_POINT('Ctrl Pts',(0.279478656084064,0.306709702649283,
-0.720834459398271));
#49442=CARTESIAN_POINT('Ctrl Pts',(0.160457302990818,0.359790206195045,
-0.71421206708389));
#49443=CARTESIAN_POINT('Ctrl Pts',(0.0414359498975732,0.412870709740808,
-0.70758967476951));
#49444=CARTESIAN_POINT('Ctrl Pts',(-0.106536331766501,0.401035124296523,
-0.700967282455129));
#49445=CARTESIAN_POINT('Ctrl Pts',(-0.215607132606148,0.329710635142869,
-0.694344890140749));
#49446=CARTESIAN_POINT('Ctrl Pts',(-0.323916805307495,0.258883869259115,
-0.687768710828331));
#49447=CARTESIAN_POINT('Ctrl Pts',(-0.39386603477197,0.129395564904208,
-0.681192531515914));
#49448=CARTESIAN_POINT('Ctrl Pts',(-0.393947723570607,-1.70646636204014E-5,
-0.674616352203497));
#49449=CARTESIAN_POINT('Origin',(0.,0.,-2.22));
#49450=CARTESIAN_POINT('',(-0.393149297351444,0.000355296501015012,-0.531283647796502));
#49451=CARTESIAN_POINT('',(-0.393099733010831,0.000348606307955762,-0.549616352203497));
#49452=CARTESIAN_POINT('',(-0.3933,-4.81653586104654E-17,-2.22));
#49453=CARTESIAN_POINT('Ctrl Pts',(-0.393149297351444,0.000355296501015012,
-0.531283647796502));
#49454=CARTESIAN_POINT('Ctrl Pts',(-0.393461166186674,0.0359366493735391,
-0.533082239723845));
#49455=CARTESIAN_POINT('Ctrl Pts',(-0.389030068485141,0.0714416959129314,
-0.534880831651188));
#49456=CARTESIAN_POINT('Ctrl Pts',(-0.37954765186827,0.105542105043303,
-0.53667942357853));
#49457=CARTESIAN_POINT('Ctrl Pts',(-0.344633515998606,0.231099372319518,
-0.543301815892911));
#49458=CARTESIAN_POINT('Ctrl Pts',(-0.241238502260482,0.337613929272207,
-0.549924208207292));
#49459=CARTESIAN_POINT('Ctrl Pts',(-0.116774198388218,0.376243727589222,
-0.556546600521672));
#49460=CARTESIAN_POINT('Ctrl Pts',(0.00769010548404041,0.414873525906236,
-0.563168992836052));
#49461=CARTESIAN_POINT('Ctrl Pts',(0.153223699490438,0.385618565587579,
-0.569791385150432));
#49462=CARTESIAN_POINT('Ctrl Pts',(0.253092429885495,0.30189365327583,-0.576413777464812));
#49463=CARTESIAN_POINT('Ctrl Pts',(0.352961160280556,0.218168740964078,
-0.583036169779193));
#49464=CARTESIAN_POINT('Ctrl Pts',(0.407165027064274,0.0799738766592314,
-0.589658562093574));
#49465=CARTESIAN_POINT('Ctrl Pts',(0.390848949798998,-0.0493219464573787,
-0.596280954407955));
#49466=CARTESIAN_POINT('Ctrl Pts',(0.374532872533722,-0.178617769573987,
-0.602903346722335));
#49467=CARTESIAN_POINT('Ctrl Pts',(0.28769685121945,-0.29901455150236,-0.609525739036715));
#49468=CARTESIAN_POINT('Ctrl Pts',(0.170159378914752,-0.355304575999081,
-0.616148131351095));
#49469=CARTESIAN_POINT('Ctrl Pts',(0.05262190661006,-0.4115946004958,-0.622770523665475));
#49470=CARTESIAN_POINT('Ctrl Pts',(-0.0956170166850531,-0.403777867560876,
-0.629392915979855));
#49471=CARTESIAN_POINT('Ctrl Pts',(-0.206582713566911,-0.33543872527383,
-0.636015308294236));
#49472=CARTESIAN_POINT('Ctrl Pts',(-0.317548410448779,-0.267099582986778,
-0.642637700608617));
#49473=CARTESIAN_POINT('Ctrl Pts',(-0.391240880917382,-0.138238031347586,
-0.649260092922997));
#49474=CARTESIAN_POINT('Ctrl Pts',(-0.393868582260403,-0.00794329070636282,
-0.655882485237378));
#49475=CARTESIAN_POINT('Ctrl Pts',(-0.393921641404054,-0.00531234964485795,
-0.656016206090419));
#49476=CARTESIAN_POINT('Ctrl Pts',(-0.393945725589634,-0.00268082423485301,
-0.65614992694346));
#49477=CARTESIAN_POINT('Ctrl Pts',(-0.393941093179356,-4.92117729247177E-5,
-0.656283647796501));
#49478=CARTESIAN_POINT('Ctrl Pts',(-0.393947723570607,-1.70646636204014E-5,
-0.674616352203497));
#49479=CARTESIAN_POINT('Ctrl Pts',(-0.393948297624998,-0.000926490307316668,
-0.674570139201534));
#49480=CARTESIAN_POINT('Ctrl Pts',(-0.393945421382037,-0.00183591221393385,
-0.674523926199571));
#49481=CARTESIAN_POINT('Ctrl Pts',(-0.393939083907698,-0.00274530999968196,
-0.674477713197608));
#49482=CARTESIAN_POINT('Ctrl Pts',(-0.393030914354389,-0.133063373125564,
-0.667855320883227));
#49483=CARTESIAN_POINT('Ctrl Pts',(-0.321045255232549,-0.262886106514305,
-0.661232928568847));
#49484=CARTESIAN_POINT('Ctrl Pts',(-0.210990994142462,-0.332683541744497,
-0.654610536254467));
#49485=CARTESIAN_POINT('Ctrl Pts',(-0.100936733052379,-0.402480976974688,
-0.647988143940086));
#49486=CARTESIAN_POINT('Ctrl Pts',(0.0471861300059487,-0.412253114046332,
-0.641365751625706));
#49487=CARTESIAN_POINT('Ctrl Pts',(0.165456136825064,-0.357518958020196,
-0.634743359311326));
#49488=CARTESIAN_POINT('Ctrl Pts',(0.283726143644182,-0.302784801994057,
-0.628120966996945));
#49489=CARTESIAN_POINT('Ctrl Pts',(0.372143294224086,-0.183544352870135,
-0.621498574682565));
#49490=CARTESIAN_POINT('Ctrl Pts',(0.390164071687642,-0.0544750926708616,
-0.614876182368184));
#49491=CARTESIAN_POINT('Ctrl Pts',(0.408184849151198,0.0745941675284096,
-0.608253790053804));
#49492=CARTESIAN_POINT('Ctrl Pts',(0.355809253498406,0.213492238803036,
-0.601631397739424));
#49493=CARTESIAN_POINT('Ctrl Pts',(0.257054014883852,0.298527673739638,
-0.595009005425043));
#49494=CARTESIAN_POINT('Ctrl Pts',(0.1582987762693,0.383563108676239,-0.588386613110663));
#49495=CARTESIAN_POINT('Ctrl Pts',(0.0131638946929933,0.414735907274821,
-0.581764220796283));
#49496=CARTESIAN_POINT('Ctrl Pts',(-0.111799304890707,0.377751841799355,
-0.575141828481902));
#49497=CARTESIAN_POINT('Ctrl Pts',(-0.236762504474413,0.340767776323887,
-0.568519436167522));
#49498=CARTESIAN_POINT('Ctrl Pts',(-0.341554022065504,0.235626846774361,
-0.561897043853141));
#49499=CARTESIAN_POINT('Ctrl Pts',(-0.378121905807111,0.110541227188991,
-0.555274651538761));
#49500=CARTESIAN_POINT('Ctrl Pts',(-0.388536673484437,0.0749160409747374,
-0.553388551760339));
#49501=CARTESIAN_POINT('Ctrl Pts',(-0.39341750218428,0.0376730473914621,
-0.551502451981918));
#49502=CARTESIAN_POINT('Ctrl Pts',(-0.393099733010831,0.000348606307955763,
-0.549616352203497));
#49503=CARTESIAN_POINT('Origin',(0.,0.,-2.22));
#49504=CARTESIAN_POINT('',(-0.392695136859145,-0.000134165267275832,-0.406283647796501));
#49505=CARTESIAN_POINT('',(-0.392714565881386,-0.000160383691160823,-0.424616352203497));
#49506=CARTESIAN_POINT('',(-0.3933,-4.81653586104654E-17,-2.22));
#49507=CARTESIAN_POINT('Ctrl Pts',(-0.392695136859145,-0.000134165267275832,
-0.406283647796501));
#49508=CARTESIAN_POINT('Ctrl Pts',(-0.39246894279338,0.0738890083694187,
-0.410014552504228));
#49509=CARTESIAN_POINT('Ctrl Pts',(-0.37239005838269,0.148026006512791,
-0.413745457211955));
#49510=CARTESIAN_POINT('Ctrl Pts',(-0.333228315284828,0.210129594475008,
-0.417476361919683));
#49511=CARTESIAN_POINT('Ctrl Pts',(-0.263715838600052,0.320364069980268,
-0.424098754234063));
#49512=CARTESIAN_POINT('Ctrl Pts',(-0.134079768270662,0.392685365088865,
-0.430721146548443));
#49513=CARTESIAN_POINT('Ctrl Pts',(-0.00376448297534652,0.393930685299415,
-0.437343538862824));
#49514=CARTESIAN_POINT('Ctrl Pts',(0.126550802319978,0.395176005509965,
-0.443965931177205));
#49515=CARTESIAN_POINT('Ctrl Pts',(0.257545302581228,0.325345350822453,
-0.450588323491586));
#49516=CARTESIAN_POINT('Ctrl Pts',(0.329151740126991,0.216459436501167,
-0.457210715805967));
#49517=CARTESIAN_POINT('Ctrl Pts',(0.400758177672747,0.107573522179891,
-0.463833108120347));
#49518=CARTESIAN_POINT('Ctrl Pts',(0.412976552503033,-0.0403676517751508,
-0.470455500434727));
#49519=CARTESIAN_POINT('Ctrl Pts',(0.360204150830326,-0.159525940801276,
-0.477077892749107));
#49520=CARTESIAN_POINT('Ctrl Pts',(0.307431749157616,-0.278684229827407,
-0.483700285063487));
#49521=CARTESIAN_POINT('Ctrl Pts',(0.189668570981906,-0.369059633924617,
-0.490322677377868));
#49522=CARTESIAN_POINT('Ctrl Pts',(0.0609146991362926,-0.389210682541646,
-0.496945069692248));
#49523=CARTESIAN_POINT('Ctrl Pts',(-0.0678391727093149,-0.409361731158675,
-0.503567462006628));
#49524=CARTESIAN_POINT('Ctrl Pts',(-0.207583738224827,-0.359288424295527,
-0.510189854321009));
#49525=CARTESIAN_POINT('Ctrl Pts',(-0.29423939198198,-0.261951782064089,
-0.516812246635389));
#49526=CARTESIAN_POINT('Ctrl Pts',(-0.357360022154415,-0.191051039525867,
-0.521636047022427));
#49527=CARTESIAN_POINT('Ctrl Pts',(-0.392312869151574,-0.0950734336898258,
-0.526459847409464));
#49528=CARTESIAN_POINT('Ctrl Pts',(-0.393149297351444,0.000355296501015012,
-0.531283647796502));
#49529=CARTESIAN_POINT('Ctrl Pts',(-0.393099733010831,0.000348606307955763,
-0.549616352203497));
#49530=CARTESIAN_POINT('Ctrl Pts',(-0.392301764747654,-0.0933789227099603,
-0.544880059667538));
#49531=CARTESIAN_POINT('Ctrl Pts',(-0.358721910614404,-0.187620052264415,
-0.540143767131579));
#49532=CARTESIAN_POINT('Ctrl Pts',(-0.297670339742412,-0.258046327990718,
-0.535407474595619));
#49533=CARTESIAN_POINT('Ctrl Pts',(-0.212306640043985,-0.356517953963846,
-0.528785082281239));
#49534=CARTESIAN_POINT('Ctrl Pts',(-0.0732349907550094,-0.408430896288897,
-0.522162689966859));
#49535=CARTESIAN_POINT('Ctrl Pts',(0.0557735668882773,-0.389980573611445,
-0.515540297652478));
#49536=CARTESIAN_POINT('Ctrl Pts',(0.184782124531568,-0.371530250933992,
-0.508917905338098));
#49537=CARTESIAN_POINT('Ctrl Pts',(0.303727590529166,-0.282716663254033,
-0.502295513023718));
#49538=CARTESIAN_POINT('Ctrl Pts',(0.358067746721792,-0.16426511294754,
-0.495673120709337));
#49539=CARTESIAN_POINT('Ctrl Pts',(0.412407902914418,-0.0458135626410491,
-0.489050728394957));
#49540=CARTESIAN_POINT('Ctrl Pts',(0.402142749302071,0.102275950291979,
-0.482428336080576));
#49541=CARTESIAN_POINT('Ctrl Pts',(0.331979352798454,0.212097260317369,
-0.475805943766196));
#49542=CARTESIAN_POINT('Ctrl Pts',(0.261815956294839,0.321918570342758,
-0.469183551451815));
#49543=CARTESIAN_POINT('Ctrl Pts',(0.131754316899958,0.393471677460513,
-0.462561159137435));
#49544=CARTESIAN_POINT('Ctrl Pts',(0.00143395259859793,0.393946039901013,
-0.455938766823055));
#49545=CARTESIAN_POINT('Ctrl Pts',(-0.128886411702766,0.394420402341514,
-0.449316374508674));
#49546=CARTESIAN_POINT('Ctrl Pts',(-0.259465500910607,0.323816020104756,
-0.442693982194294));
#49547=CARTESIAN_POINT('Ctrl Pts',(-0.33042652043779,0.214508399029338,
-0.436071589879914));
#49548=CARTESIAN_POINT('Ctrl Pts',(-0.371342013704453,0.151482596075745,
-0.432253177321108));
#49549=CARTESIAN_POINT('Ctrl Pts',(-0.392437043766175,0.0755896183641849,
-0.428434764762302));
#49550=CARTESIAN_POINT('Ctrl Pts',(-0.392714565881386,-0.000160383691160823,
-0.424616352203497));
#49551=CARTESIAN_POINT('Origin',(0.,0.,-2.22));
#49552=CARTESIAN_POINT('',(-0.393642003299011,-0.000296307799958484,-0.281283647796501));
#49553=CARTESIAN_POINT('',(-0.393688345169262,-0.000277587037033014,-0.299616352203497));
#49554=CARTESIAN_POINT('',(-0.3933,-4.81653586104654E-17,-2.22));
#49555=CARTESIAN_POINT('Ctrl Pts',(-0.393642003299011,-0.000296307799958484,
-0.281283647796501));
#49556=CARTESIAN_POINT('Ctrl Pts',(-0.392705570089931,0.111378501625261,
-0.286946865284613));
#49557=CARTESIAN_POINT('Ctrl Pts',(-0.342835655720549,0.223784343425498,
-0.292610082772724));
#49558=CARTESIAN_POINT('Ctrl Pts',(-0.258815660133244,0.297001729802868,
-0.298273300260836));
#49559=CARTESIAN_POINT('Ctrl Pts',(-0.160565261980655,0.382619889063466,
-0.304895692575216));
#49560=CARTESIAN_POINT('Ctrl Pts',(-0.0156172090648659,0.414650797671215,
-0.311518084889597));
#49561=CARTESIAN_POINT('Ctrl Pts',(0.109562634218419,0.378406661592715,
-0.318140477203977));
#49562=CARTESIAN_POINT('Ctrl Pts',(0.234742477501703,0.342162525514216,
-0.324762869518358));
#49563=CARTESIAN_POINT('Ctrl Pts',(0.340154111152485,0.237643344749466,
-0.331385261832738));
#49564=CARTESIAN_POINT('Ctrl Pts',(0.37746133962886,0.112776234214326,-0.338007654147118));
#49565=CARTESIAN_POINT('Ctrl Pts',(0.414768568105235,-0.0120908763208124,
-0.344630046461499));
#49566=CARTESIAN_POINT('Ctrl Pts',(0.383971391407208,-0.157305916626339,
-0.351252438775879));
#49567=CARTESIAN_POINT('Ctrl Pts',(0.299191739449069,-0.256280827360889,
-0.357874831090259));
#49568=CARTESIAN_POINT('Ctrl Pts',(0.214412087490928,-0.35525573809544,
-0.36449722340464));
#49569=CARTESIAN_POINT('Ctrl Pts',(0.0756499602726728,-0.407990519259011,
-0.37111961571902));
#49570=CARTESIAN_POINT('Ctrl Pts',(-0.0534655018538449,-0.390303725242715,
-0.377742008033401));
#49571=CARTESIAN_POINT('Ctrl Pts',(-0.182580963980366,-0.37261693122642,
-0.384364400347781));
#49572=CARTESIAN_POINT('Ctrl Pts',(-0.302049761015151,-0.284508562030254,
-0.390986792662162));
#49573=CARTESIAN_POINT('Ctrl Pts',(-0.357089718012459,-0.166380549481205,
-0.397609184976543));
#49574=CARTESIAN_POINT('Ctrl Pts',(-0.381121419242666,-0.114803163535286,
-0.400500672583195));
#49575=CARTESIAN_POINT('Ctrl Pts',(-0.392870439470467,-0.0575028481854697,
-0.403392160189848));
#49576=CARTESIAN_POINT('Ctrl Pts',(-0.392695136859145,-0.000134165267275832,
-0.406283647796501));
#49577=CARTESIAN_POINT('Ctrl Pts',(-0.392714565881386,-0.000160383691160823,
-0.424616352203497));
#49578=CARTESIAN_POINT('Ctrl Pts',(-0.392918359049566,-0.0557859791387052,
-0.421812372447922));
#49579=CARTESIAN_POINT('Ctrl Pts',(-0.381896468881979,-0.111334476047582,
-0.419008392692347));
#49580=CARTESIAN_POINT('Ctrl Pts',(-0.359254083037642,-0.161654081597039,
-0.416204412936772));
#49581=CARTESIAN_POINT('Ctrl Pts',(-0.305777676263785,-0.28049808123393,
-0.409582020622392));
#49582=CARTESIAN_POINT('Ctrl Pts',(-0.187481912869543,-0.370175220593635,
-0.402959628308012));
#49583=CARTESIAN_POINT('Ctrl Pts',(-0.0586110886880626,-0.389564216829724,
-0.396337235993631));
#49584=CARTESIAN_POINT('Ctrl Pts',(0.0702597354934178,-0.408953213065813,
-0.389714843679251));
#49585=CARTESIAN_POINT('Ctrl Pts',(0.209705620462139,-0.358054066178287,
-0.38309245136487));
#49586=CARTESIAN_POINT('Ctrl Pts',(0.29578391539786,-0.260206484498071,
-0.376470059050489));
#49587=CARTESIAN_POINT('Ctrl Pts',(0.381862210333579,-0.162358902817856,
-0.369847666736109));
#49588=CARTESIAN_POINT('Ctrl Pts',(0.414572915236302,-0.0175628863449562,
-0.363225274421729));
#49589=CARTESIAN_POINT('Ctrl Pts',(0.378916606915431,0.1077856277556,-0.356602882107349));
#49590=CARTESIAN_POINT('Ctrl Pts',(0.34326029859456,0.233134141856158,-0.349980489792969));
#49591=CARTESIAN_POINT('Ctrl Pts',(0.23923697705009,0.33903515358437,-0.343358097478588));
#49592=CARTESIAN_POINT('Ctrl Pts',(0.114546322886326,0.376927951129987,
-0.336735705164207));
#49593=CARTESIAN_POINT('Ctrl Pts',(-0.0101443312774386,0.414820748675605,
-0.330113312849827));
#49594=CARTESIAN_POINT('Ctrl Pts',(-0.155502318060499,0.384705332038629,
-0.323490920535446));
#49595=CARTESIAN_POINT('Ctrl Pts',(-0.254873976640853,0.300391075219788,
-0.316868528221066));
#49596=CARTESIAN_POINT('Ctrl Pts',(-0.341165921887652,0.227174613535666,
-0.311117802881876));
#49597=CARTESIAN_POINT('Ctrl Pts',(-0.392780654944496,0.11308807687727,
-0.305367077542686));
#49598=CARTESIAN_POINT('Ctrl Pts',(-0.393688345169262,-0.000277587037033014,
-0.299616352203497));
#49599=CARTESIAN_POINT('Origin',(0.,0.,-2.22));
#49600=CARTESIAN_POINT('',(-0.393631981127146,0.00030016282702406,-0.156283647796501));
#49601=CARTESIAN_POINT('',(-0.393585661406795,0.000315388445219644,-0.174616352203498));
#49602=CARTESIAN_POINT('',(-0.3933,-4.81653586104654E-17,-2.22));
#49603=CARTESIAN_POINT('Ctrl Pts',(-0.393631981127146,0.00030016282702406,
-0.156283647796501));
#49604=CARTESIAN_POINT('Ctrl Pts',(-0.393792621966079,0.0194912539892937,
-0.157256785750617));
#49605=CARTESIAN_POINT('Ctrl Pts',(-0.392509708971423,0.0386605451791385,
-0.158229923704732));
#49606=CARTESIAN_POINT('Ctrl Pts',(-0.389708810446672,0.0576052757599894,
-0.159203061658848));
#49607=CARTESIAN_POINT('Ctrl Pts',(-0.370648153337135,0.186527837731874,
-0.165825453973228));
#49608=CARTESIAN_POINT('Ctrl Pts',(-0.281288581648335,0.305050849275526,
-0.172447846287608));
#49609=CARTESIAN_POINT('Ctrl Pts',(-0.16258600572988,0.358833504095236,
-0.179070238601988));
#49610=CARTESIAN_POINT('Ctrl Pts',(-0.0438834298114263,0.412616158914947,
-0.185692630916368));
#49611=CARTESIAN_POINT('Ctrl Pts',(0.104162150336679,0.401658457010715,
-0.192315023230749));
#49612=CARTESIAN_POINT('Ctrl Pts',(0.213654399121235,0.330981012427604,
-0.198937415545129));
#49613=CARTESIAN_POINT('Ctrl Pts',(0.323146647905798,0.26030356784449,-0.20555980785951));
#49614=CARTESIAN_POINT('Ctrl Pts',(0.394085565326806,0.129906380582479,
-0.212182200173891));
#49615=CARTESIAN_POINT('Ctrl Pts',(0.393947632619649,-0.000415066957393126,
-0.218804592488271));
#49616=CARTESIAN_POINT('Ctrl Pts',(0.393809699912491,-0.130736514497255,
-0.225426984802652));
#49617=CARTESIAN_POINT('Ctrl Pts',(0.322594917077188,-0.260982222314982,
-0.232049377117032));
#49618=CARTESIAN_POINT('Ctrl Pts',(0.212955874119221,-0.331429364260128,
-0.238671769431412));
#49619=CARTESIAN_POINT('Ctrl Pts',(0.103316831161247,-0.401876506205278,
-0.245294161745793));
#49620=CARTESIAN_POINT('Ctrl Pts',(-0.0447464719193912,-0.412525082277837,
-0.251916554060173));
#49621=CARTESIAN_POINT('Ctrl Pts',(-0.163338418470475,-0.358491635469819,
-0.258538946374553));
#49622=CARTESIAN_POINT('Ctrl Pts',(-0.281930365021556,-0.304458188661802,
-0.265161338688934));
#49623=CARTESIAN_POINT('Ctrl Pts',(-0.371050955043081,-0.185742718973213,
-0.271783731003314));
#49624=CARTESIAN_POINT('Ctrl Pts',(-0.389834878359152,-0.0567822791721963,
-0.278406123317694));
#49625=CARTESIAN_POINT('Ctrl Pts',(-0.392555506423457,-0.0381038920320804,
-0.279365298143963));
#49626=CARTESIAN_POINT('Ctrl Pts',(-0.393800606277357,-0.0192105850909033,
-0.280324472970232));
#49627=CARTESIAN_POINT('Ctrl Pts',(-0.393642003299011,-0.000296307799958484,
-0.281283647796501));
#49628=CARTESIAN_POINT('Ctrl Pts',(-0.393688345169262,-0.000277587037033014,
-0.299616352203497));
#49629=CARTESIAN_POINT('Ctrl Pts',(-0.393825928438496,-0.017461002958714,
-0.298744685228306));
#49630=CARTESIAN_POINT('Ctrl Pts',(-0.392798516291064,-0.0346278568133537,
-0.297873018253116));
#49631=CARTESIAN_POINT('Ctrl Pts',(-0.390550285770528,-0.0516333105353148,
-0.297001351277925));
#49632=CARTESIAN_POINT('Ctrl Pts',(-0.373469605942206,-0.18083034247088,
-0.290378958963545));
#49633=CARTESIAN_POINT('Ctrl Pts',(-0.285922915907914,-0.300711309341301,
-0.283756566649164));
#49634=CARTESIAN_POINT('Ctrl Pts',(-0.168054469471746,-0.35630499614788,
-0.277134174334784));
#49635=CARTESIAN_POINT('Ctrl Pts',(-0.0501860230355798,-0.411898682954459,
-0.270511782020403));
#49636=CARTESIAN_POINT('Ctrl Pts',(0.0980041798024627,-0.403205089697194,
-0.263889389706022));
#49637=CARTESIAN_POINT('Ctrl Pts',(0.208563582086416,-0.334210694524994,
-0.257266997391642));
#49638=CARTESIAN_POINT('Ctrl Pts',(0.319122984370366,-0.265216299352795,
-0.250644605077262));
#49639=CARTESIAN_POINT('Ctrl Pts',(0.392051586100232,-0.135921102265661,
-0.244022212762882));
#49640=CARTESIAN_POINT('Ctrl Pts',(0.39390853670177,-0.00561308011220472,
-0.237399820448502));
#49641=CARTESIAN_POINT('Ctrl Pts',(0.395765487303308,0.124694942041256,
-0.230777428134121));
#49642=CARTESIAN_POINT('Ctrl Pts',(0.326550786776514,0.256015789261044,
-0.22415503581974));
#49643=CARTESIAN_POINT('Ctrl Pts',(0.218001897880293,0.328132362043281,
-0.21753264350536));
#49644=CARTESIAN_POINT('Ctrl Pts',(0.109453008984069,0.400248934825521,
-0.210910251190979));
#49645=CARTESIAN_POINT('Ctrl Pts',(-0.0384300682815738,0.413161233170207,
-0.204287858876599));
#49646=CARTESIAN_POINT('Ctrl Pts',(-0.157834284113371,0.360948679891727,
-0.197665466562219));
#49647=CARTESIAN_POINT('Ctrl Pts',(-0.277238499945161,0.308736126613249,
-0.191043074247839));
#49648=CARTESIAN_POINT('Ctrl Pts',(-0.368163854343102,0.191398721711606,
-0.184420681933458));
#49649=CARTESIAN_POINT('Ctrl Pts',(-0.38891965580233,0.0627406728828643,
-0.177798289619078));
#49650=CARTESIAN_POINT('Ctrl Pts',(-0.392243915783628,0.0421347327155593,
-0.176737643813884));
#49651=CARTESIAN_POINT('Ctrl Pts',(-0.39376822901556,0.0212384022666582,
-0.175676998008691));
#49652=CARTESIAN_POINT('Ctrl Pts',(-0.393585661406795,0.000315388445219644,
-0.174616352203498));
#49653=CARTESIAN_POINT('Origin',(0.,0.,-2.22));
#49654=CARTESIAN_POINT('',(-0.3933,-4.81653586104654E-17,-0.04));
#49655=CARTESIAN_POINT('',(-0.39272888104496,9.19390291685468E-5,-0.0496163522034977));
#49656=CARTESIAN_POINT('',(-0.3933,-4.81653586104654E-17,-2.22));
#49657=CARTESIAN_POINT('',(-0.356151197810523,0.166856867698425,-0.04));
#49658=CARTESIAN_POINT('Origin',(0.,0.,-0.04));
#49659=CARTESIAN_POINT('Ctrl Pts',(-0.356151197810523,0.166856867698425,
-0.04));
#49660=CARTESIAN_POINT('Ctrl Pts',(-0.300608260002572,0.285411675199488,
-0.0466223923143805));
#49661=CARTESIAN_POINT('Ctrl Pts',(-0.181688079154573,0.373019047260479,
-0.0532447846287612));
#49662=CARTESIAN_POINT('Ctrl Pts',(-0.0527476824217043,0.390367240993339,
-0.0598671769431416));
#49663=CARTESIAN_POINT('Ctrl Pts',(0.0761927143111604,0.407715434726198,
-0.0664895692575218));
#49664=CARTESIAN_POINT('Ctrl Pts',(0.215153326928898,0.35480445013093,-0.0731119615719019));
#49665=CARTESIAN_POINT('Ctrl Pts',(0.2998027398245,0.25567960187594,-0.0797343538862821));
#49666=CARTESIAN_POINT('Ctrl Pts',(0.384452152720104,0.156554753620946,
-0.0863567462006626));
#49667=CARTESIAN_POINT('Ctrl Pts',(0.414790365893573,0.0112160417062353,
-0.0929791385150429));
#49668=CARTESIAN_POINT('Ctrl Pts',(0.377183219450442,-0.113586432810944,
-0.0996015308294233));
#49669=CARTESIAN_POINT('Ctrl Pts',(0.33957607300731,-0.238388907328124,
-0.106223923143804));
#49670=CARTESIAN_POINT('Ctrl Pts',(0.234023566947572,-0.342655144447766,
-0.112846315458184));
#49671=CARTESIAN_POINT('Ctrl Pts',(0.108786645000273,-0.378628284581708,
-0.119468707772564));
#49672=CARTESIAN_POINT('Ctrl Pts',(-0.0164502769470251,-0.41460142471565,
-0.126091100086945));
#49673=CARTESIAN_POINT('Ctrl Pts',(-0.161371614781888,-0.382281467863894,
-0.132713492401325));
#49674=CARTESIAN_POINT('Ctrl Pts',(-0.259451412434183,-0.296460433237957,
-0.139335884715706));
#49675=CARTESIAN_POINT('Ctrl Pts',(-0.34311871848278,-0.223250506817523,
-0.144985139075971));
#49676=CARTESIAN_POINT('Ctrl Pts',(-0.39269942993444,-0.11110783946927,
-0.150634393436236));
#49677=CARTESIAN_POINT('Ctrl Pts',(-0.393631981127146,0.00030016282702406,
-0.156283647796501));
#49678=CARTESIAN_POINT('Ctrl Pts',(-0.393585661406795,0.000315388445219644,
-0.174616352203498));
#49679=CARTESIAN_POINT('Ctrl Pts',(-0.39262832507852,-0.109399370726316,
-0.169054605694311));
#49680=CARTESIAN_POINT('Ctrl Pts',(-0.34473728496773,-0.219847836359808,
-0.163492859185123));
#49681=CARTESIAN_POINT('Ctrl Pts',(-0.263331321875656,-0.293007221603574,
-0.157931112675936));
#49682=CARTESIAN_POINT('Ctrl Pts',(-0.166400937969243,-0.380118374505416,
-0.151308720361556));
#49683=CARTESIAN_POINT('Ctrl Pts',(-0.0219539216358963,-0.414361987553257,
-0.144686328047175));
#49684=CARTESIAN_POINT('Ctrl Pts',(0.103762983130385,-0.380038051262661,
-0.138063935732795));
#49685=CARTESIAN_POINT('Ctrl Pts',(0.22947988789667,-0.345714114972064,
-0.131441543418414));
#49686=CARTESIAN_POINT('Ctrl Pts',(0.336466681095895,-0.242822629343032,
-0.124819151104034));
#49687=CARTESIAN_POINT('Ctrl Pts',(0.375685521011522,-0.118539821363215,
-0.118196758789653));
#49688=CARTESIAN_POINT('Ctrl Pts',(0.414904360927149,0.0057429866165986,
-0.111574366475273));
#49689=CARTESIAN_POINT('Ctrl Pts',(0.386355247559182,0.151417116947191,
-0.104951974160893));
#49690=CARTESIAN_POINT('Ctrl Pts',(0.303089588085626,0.251675418462943,
-0.0983295818465127));
#49691=CARTESIAN_POINT('Ctrl Pts',(0.219823928612068,0.351933719978697,
-0.0917071895321323));
#49692=CARTESIAN_POINT('Ctrl Pts',(0.081841723032909,0.406776192679608,
-0.0850847972177514));
#49693=CARTESIAN_POINT('Ctrl Pts',(-0.0475093665302487,0.391071300758949,
-0.0784624049033708));
#49694=CARTESIAN_POINT('Ctrl Pts',(-0.176860456093399,0.37536640883829,
-0.0718400125889905));
#49695=CARTESIAN_POINT('Ctrl Pts',(-0.297580429640553,0.289114152296078,
-0.0652176202746104));
#49696=CARTESIAN_POINT('Ctrl Pts',(-0.354460273107469,0.171833994016063,
-0.0585952279602302));
#49697=CARTESIAN_POINT('Ctrl Pts',(-0.380166846769823,0.118829786476159,
-0.0556022693746527));
#49698=CARTESIAN_POINT('Ctrl Pts',(-0.392833787442048,0.0594879907984162,
-0.0526093107890752));
#49699=CARTESIAN_POINT('Ctrl Pts',(-0.39272888104496,9.19390291685468E-5,
-0.0496163522034977));
#49700=CARTESIAN_POINT('Origin',(0.,0.,-3.17777734492731));
#49701=CARTESIAN_POINT('',(-0.322547029539158,0.000245957221170181,-0.115277344927309));
#49702=CARTESIAN_POINT('',(-0.321807017896681,7.53360046316098E-5,-0.0906226550726903));
#49703=CARTESIAN_POINT('',(-0.322275,-1.53308031181269E-15,-3.17777734492731));
#49704=CARTESIAN_POINT('',(0.258431022718474,0.193451597832761,-0.0400000000000002));
#49705=CARTESIAN_POINT('Ctrl Pts',(-0.322547029539158,0.000245957221170202,
-0.115277344927309));
#49706=CARTESIAN_POINT('Ctrl Pts',(-0.321782885283814,-0.0910431705185724,
-0.109628090567044));
#49707=CARTESIAN_POINT('Ctrl Pts',(-0.233530360647496,-0.290654535970315,
-0.0973564438923979));
#49708=CARTESIAN_POINT('Ctrl Pts',(0.105270814003626,-0.366213039015092,
-0.0784624049033714));
#49709=CARTESIAN_POINT('Ctrl Pts',(0.359206608534133,-0.115371720754992,
-0.0590192109545344));
#49710=CARTESIAN_POINT('Ctrl Pts',(0.317979897957302,0.113102706613816,
-0.046198409320077));
#49711=CARTESIAN_POINT('Ctrl Pts',(0.258434353604258,0.193455249693963,
-0.0400000000000002));
#49712=CARTESIAN_POINT('',(0.266526038810872,-0.181176836987473,-0.04));
#49713=CARTESIAN_POINT('Origin',(0.,0.,-0.04));
#49714=CARTESIAN_POINT('Ctrl Pts',(-0.321807017896681,7.53360046315855E-5,
-0.0906226550726902));
#49715=CARTESIAN_POINT('Ctrl Pts',(-0.3217027758797,-0.0589445560984634,
-0.0869932213438877));
#49716=CARTESIAN_POINT('Ctrl Pts',(-0.277937787262726,-0.225838884443167,
-0.0767413953007049));
#49717=CARTESIAN_POINT('Ctrl Pts',(-0.00893422490495668,-0.380826657875824,
-0.0598671769431404));
#49718=CARTESIAN_POINT('Ctrl Pts',(0.206216301921741,-0.269897423691928,
-0.0466223923143805));
#49719=CARTESIAN_POINT('Ctrl Pts',(0.266526038810872,-0.181176836987473,
-0.04));
#49720=CARTESIAN_POINT('Origin',(0.,0.,-3.17777734492731));
#49721=CARTESIAN_POINT('',(-0.322555241833687,-0.000242798363153271,-0.240277344927309));
#49722=CARTESIAN_POINT('',(-0.322509074573798,0.000258433285462066,-0.21562265507269));
#49723=CARTESIAN_POINT('',(-0.322275,-1.53308031181269E-15,-3.17777734492731));
#49724=CARTESIAN_POINT('Ctrl Pts',(-0.322555241833687,-0.000242798363153243,
-0.240277344927309));
#49725=CARTESIAN_POINT('Ctrl Pts',(-0.322685203122389,-0.0157413966696349,
-0.23931817010104));
#49726=CARTESIAN_POINT('Ctrl Pts',(-0.314620877302866,-0.138110524338227,
-0.23173660296039));
#49727=CARTESIAN_POINT('Ctrl Pts',(-0.157990771009751,-0.346753853915265,
-0.21753264350536));
#49728=CARTESIAN_POINT('Ctrl Pts',(0.205984064995685,-0.320577119714015,
-0.197665466562219));
#49729=CARTESIAN_POINT('Ctrl Pts',(0.381046949345406,-0.000402173207826333,
-0.177798289619077));
#49730=CARTESIAN_POINT('Ctrl Pts',(0.206662207836228,0.320145145822377,
-0.157931112675937));
#49731=CARTESIAN_POINT('Ctrl Pts',(-0.157269060983239,0.347081784885588,
-0.138063935732795));
#49732=CARTESIAN_POINT('Ctrl Pts',(-0.314473566646606,0.138571928724442,
-0.12384601314992));
#49733=CARTESIAN_POINT('Ctrl Pts',(-0.322678660676628,0.0159713803188515,
-0.116250482881424));
#49734=CARTESIAN_POINT('Ctrl Pts',(-0.322547029539158,0.000245957221170202,
-0.115277344927309));
#49735=CARTESIAN_POINT('Ctrl Pts',(-0.322509074573798,0.000258433285462089,
-0.21562265507269));
#49736=CARTESIAN_POINT('Ctrl Pts',(-0.321724621064523,-0.08964322959784,
-0.210060908563503));
#49737=CARTESIAN_POINT('Ctrl Pts',(-0.235755875896869,-0.287908207227001,
-0.197876769739936));
#49738=CARTESIAN_POINT('Ctrl Pts',(0.100372392813672,-0.367593109417031,
-0.179070238601988));
#49739=CARTESIAN_POINT('Ctrl Pts',(0.363371391885224,-0.114661350979993,
-0.159203061658847));
#49740=CARTESIAN_POINT('Ctrl Pts',(0.29319087692976,0.243440329815534,-0.139335884715706));
#49741=CARTESIAN_POINT('Ctrl Pts',(-0.0460022222542214,0.378256179469882,
-0.119468707772565));
#49742=CARTESIAN_POINT('Ctrl Pts',(-0.28854735638966,0.204962030061018,
-0.103230964558226));
#49743=CARTESIAN_POINT('Ctrl Pts',(-0.32189297952679,0.0487452129025094,
-0.093615613658268));
#49744=CARTESIAN_POINT('Ctrl Pts',(-0.321807017896681,7.53360046315855E-5,
-0.0906226550726902));
#49745=CARTESIAN_POINT('Origin',(0.,0.,-3.17777734492731));
#49746=CARTESIAN_POINT('',(-0.321779367483552,-0.000109936718809572,-0.365277344927308));
#49747=CARTESIAN_POINT('',(-0.322593214948955,-0.000227458332986402,-0.340622655072689));
#49748=CARTESIAN_POINT('',(-0.322275,-1.53308031181269E-15,-3.17777734492731));
#49749=CARTESIAN_POINT('Ctrl Pts',(-0.321779367483552,-0.000109936718809583,
-0.365277344927308));
#49750=CARTESIAN_POINT('Ctrl Pts',(-0.321923012662968,-0.0471185619094107,
-0.362385857320655));
#49751=CARTESIAN_POINT('Ctrl Pts',(-0.290246260065477,-0.201607010980205,
-0.352871977399622));
#49752=CARTESIAN_POINT('Ctrl Pts',(-0.0517149087271477,-0.377524144911485,
-0.336735705164208));
#49753=CARTESIAN_POINT('Ctrl Pts',(0.289395423456396,-0.247889502657562,
-0.316868528221066));
#49754=CARTESIAN_POINT('Ctrl Pts',(0.365102213085359,0.109083625599228,
-0.297001351277925));
#49755=CARTESIAN_POINT('Ctrl Pts',(0.105975331050231,0.366016646048953,
-0.277134174334784));
#49756=CARTESIAN_POINT('Ctrl Pts',(-0.233138726856483,0.291078548034463,
-0.258226172217912));
#49757=CARTESIAN_POINT('Ctrl Pts',(-0.321787916604962,0.0912649545163569,
-0.24594056241542));
#49758=CARTESIAN_POINT('Ctrl Pts',(-0.322555241833687,-0.000242798363153243,
-0.240277344927309));
#49759=CARTESIAN_POINT('Ctrl Pts',(-0.322593214948955,-0.000227458332986343,
-0.340622655072689));
#49760=CARTESIAN_POINT('Ctrl Pts',(-0.322705952421856,-0.0143077669171678,
-0.339750988097499));
#49761=CARTESIAN_POINT('Ctrl Pts',(-0.315468030408353,-0.135244967949515,
-0.332256928807928));
#49762=CARTESIAN_POINT('Ctrl Pts',(-0.162551991338471,-0.344638636705144,
-0.318140477203977));
#49763=CARTESIAN_POINT('Ctrl Pts',(0.201734794471057,-0.323267715522956,
-0.298273300260835));
#49764=CARTESIAN_POINT('Ctrl Pts',(0.381010653528974,-0.00542935060109167,
-0.278406123317695));
#49765=CARTESIAN_POINT('Ctrl Pts',(0.210864447485707,0.317388544423747,
-0.258538946374552));
#49766=CARTESIAN_POINT('Ctrl Pts',(-0.152667350575211,0.34913004670471,
-0.238671769431413));
#49767=CARTESIAN_POINT('Ctrl Pts',(-0.313610945544451,0.141435461467442,
-0.224366338997457));
#49768=CARTESIAN_POINT('Ctrl Pts',(-0.322658672784109,0.0174030157398424,
-0.216683300877883));
#49769=CARTESIAN_POINT('Ctrl Pts',(-0.322509074573798,0.000258433285462089,
-0.21562265507269));
#49770=CARTESIAN_POINT('Origin',(0.,0.,-3.17777734492731));
#49771=CARTESIAN_POINT('',(-0.322151512341563,0.00029113445171856,-0.490277344927309));
#49772=CARTESIAN_POINT('',(-0.321795287870388,-0.000131420427339407,-0.465622655072689));
#49773=CARTESIAN_POINT('',(-0.322275,-1.53308031181269E-15,-3.17777734492731));
#49774=CARTESIAN_POINT('Ctrl Pts',(-0.322151512341563,0.000291134451718522,
-0.490277344927308));
#49775=CARTESIAN_POINT('Ctrl Pts',(-0.321466132483658,-0.0779043753938241,
-0.485453544540271));
#49776=CARTESIAN_POINT('Ctrl Pts',(-0.253505572034916,-0.264518412404189,
-0.474007351838853));
#49777=CARTESIAN_POINT('Ctrl Pts',(0.0589201893379548,-0.376466887562887,
-0.455938766823054));
#49778=CARTESIAN_POINT('Ctrl Pts',(0.348410107313365,-0.154302636186626,
-0.436071589879914));
#49779=CARTESIAN_POINT('Ctrl Pts',(0.318374434175064,0.20937197736306,-0.416204412936773));
#49780=CARTESIAN_POINT('Ctrl Pts',(-0.0036412223595689,0.38103234532199,
-0.396337235993631));
#49781=CARTESIAN_POINT('Ctrl Pts',(-0.27593708477359,0.229124088827818,
-0.379361546657143));
#49782=CARTESIAN_POINT('Ctrl Pts',(-0.321594021201972,0.0605455890471819,
-0.369008249635035));
#49783=CARTESIAN_POINT('Ctrl Pts',(-0.321779367483552,-0.000109936718809583,
-0.365277344927308));
#49784=CARTESIAN_POINT('Ctrl Pts',(-0.321795287870388,-0.000131420427339393,
-0.465622655072689));
#49785=CARTESIAN_POINT('Ctrl Pts',(-0.321962278572841,-0.0457117376733506,
-0.462818675317115));
#49786=CARTESIAN_POINT('Ctrl Pts',(-0.291600412951676,-0.198730500604296,
-0.453392303247159));
#49787=CARTESIAN_POINT('Ctrl Pts',(-0.0566920069213143,-0.376808846437738,
-0.437343538862825));
#49788=CARTESIAN_POINT('Ctrl Pts',(0.286099164537831,-0.251686630090085,
-0.417476361919683));
#49789=CARTESIAN_POINT('Ctrl Pts',(0.366509861887374,0.104256437864189,
-0.397609184976542));
#49790=CARTESIAN_POINT('Ctrl Pts',(0.110795781408782,0.364586327678901,
-0.3777420080334));
#49791=CARTESIAN_POINT('Ctrl Pts',(-0.230851227146932,0.293803550391354,
-0.35874649806545));
#49792=CARTESIAN_POINT('Ctrl Pts',(-0.321849442085529,0.0926658021246373,
-0.346373380411879));
#49793=CARTESIAN_POINT('Ctrl Pts',(-0.322593214948955,-0.000227458332986343,
-0.340622655072689));
#49794=CARTESIAN_POINT('Origin',(0.,0.,-3.17777734492731));
#49795=CARTESIAN_POINT('',(-0.322800319868744,-4.03247498678985E-5,-0.615277344927307));
#49796=CARTESIAN_POINT('',(-0.322110898693276,0.000285652422795588,-0.590622655072689));
#49797=CARTESIAN_POINT('',(-0.322275,-1.53308031181269E-15,-3.17777734492731));
#49798=CARTESIAN_POINT('Ctrl Pts',(-0.322800319868744,-4.03247498679347E-5,
-0.615277344927308));
#49799=CARTESIAN_POINT('Ctrl Pts',(-0.322804115724382,-0.00219670132288585,
-0.615143624074267));
#49800=CARTESIAN_POINT('Ctrl Pts',(-0.32180703019643,-0.111141880060886,
-0.608387510906845));
#49801=CARTESIAN_POINT('Ctrl Pts',(-0.199818644945625,-0.324455567408028,
-0.595009005425044));
#49802=CARTESIAN_POINT('Ctrl Pts',(0.164587907342214,-0.343670957237192,
-0.575141828481902));
#49803=CARTESIAN_POINT('Ctrl Pts',(0.378051513513506,-0.0477070144762039,
-0.555274651538762));
#49804=CARTESIAN_POINT('Ctrl Pts',(0.24480550918305,0.2920088504654,-0.535407474595619));
#49805=CARTESIAN_POINT('Ctrl Pts',(-0.112950699881881,0.363924505207545,
-0.515540297652479));
#49806=CARTESIAN_POINT('Ctrl Pts',(-0.30540724597967,0.165661329846195,
-0.500496921096375));
#49807=CARTESIAN_POINT('Ctrl Pts',(-0.322407061614062,0.0294469455297607,
-0.492075936854651));
#49808=CARTESIAN_POINT('Ctrl Pts',(-0.322151512341563,0.000291134451718522,
-0.490277344927308));
#49809=CARTESIAN_POINT('Ctrl Pts',(-0.322110898693276,0.000285652422795598,
-0.590622655072689));
#49810=CARTESIAN_POINT('Ctrl Pts',(-0.321457033394476,-0.0765158716408842,
-0.58588636253673));
#49811=CARTESIAN_POINT('Ctrl Pts',(-0.25546811539684,-0.261712333349606,
-0.574527677686391));
#49812=CARTESIAN_POINT('Ctrl Pts',(0.0539473916324327,-0.377211570275388,
-0.556546600521672));
#49813=CARTESIAN_POINT('Ctrl Pts',(0.346343654442317,-0.158886635343591,
-0.53667942357853));
#49814=CARTESIAN_POINT('Ctrl Pts',(0.321109463897549,0.205152630716595,
-0.516812246635389));
#49815=CARTESIAN_POINT('Ctrl Pts',(0.00138700138049073,0.381047196669113,
-0.496945069692247));
#49816=CARTESIAN_POINT('Ctrl Pts',(-0.274303504523829,0.231980772818264,
-0.479881872504682));
#49817=CARTESIAN_POINT('Ctrl Pts',(-0.321567882735176,0.0619390904101579,
-0.469441067631495));
#49818=CARTESIAN_POINT('Ctrl Pts',(-0.321795287870388,-0.000131420427339393,
-0.465622655072689));
#49819=CARTESIAN_POINT('Origin',(0.,0.,-3.17777734492731));
#49820=CARTESIAN_POINT('',(-0.322031575383028,-0.00026858467163699,-0.740277344927308));
#49821=CARTESIAN_POINT('',(-0.32280575289529,-1.39830014679876E-5,-0.715622655072688));
#49822=CARTESIAN_POINT('',(-0.322275,-1.53308031181269E-15,-3.17777734492731));
#49823=CARTESIAN_POINT('Ctrl Pts',(-0.322031575383028,-0.000268584671637075,
-0.740277344927308));
#49824=CARTESIAN_POINT('Ctrl Pts',(-0.322294991248528,-0.0337913139650879,
-0.738211311293882));
#49825=CARTESIAN_POINT('Ctrl Pts',(-0.302040555874669,-0.174456222783985,
-0.729522885346076));
#49826=CARTESIAN_POINT('Ctrl Pts',(-0.098186030593751,-0.368182576296315,
-0.714212067083892));
#49827=CARTESIAN_POINT('Ctrl Pts',(0.256379762883779,-0.281901265118838,
-0.694344890140749));
#49828=CARTESIAN_POINT('Ctrl Pts',(0.375820647341585,0.0629106280680267,
-0.674477713197609));
#49829=CARTESIAN_POINT('Ctrl Pts',(0.150597840249194,0.35002742264572,-0.654610536254467));
#49830=CARTESIAN_POINT('Ctrl Pts',(-0.210292157648995,0.316363512819851,
-0.634877080164367));
#49831=CARTESIAN_POINT('Ctrl Pts',(-0.322616129747388,0.104595704792612,
-0.621766016388647));
#49832=CARTESIAN_POINT('Ctrl Pts',(-0.322800319868744,-4.03247498679347E-5,
-0.615277344927308));
#49833=CARTESIAN_POINT('Ctrl Pts',(-0.32280575289529,-1.39830014679308E-5,
-0.715622655072688));
#49834=CARTESIAN_POINT('Ctrl Pts',(-0.322806223282726,-0.000759177889134405,
-0.715576442070726));
#49835=CARTESIAN_POINT('Ctrl Pts',(-0.322466129202107,-0.10829147308526,
-0.708907836754383));
#49836=CARTESIAN_POINT('Ctrl Pts',(-0.204082586668139,-0.321790595931231,
-0.695616839123661));
#49837=CARTESIAN_POINT('Ctrl Pts',(0.160038661936921,-0.345812834487786,
-0.675749662180518));
#49838=CARTESIAN_POINT('Ctrl Pts',(0.377389060130195,-0.0526914329514625,
-0.655882485237377));
#49839=CARTESIAN_POINT('Ctrl Pts',(0.248637381342986,0.288753082075454,
-0.636015308294237));
#49840=CARTESIAN_POINT('Ctrl Pts',(-0.108138697680715,0.365383239728838,
-0.616148131351095));
#49841=CARTESIAN_POINT('Ctrl Pts',(-0.304329303822686,0.168538464761997,
-0.601017246943913));
#49842=CARTESIAN_POINT('Ctrl Pts',(-0.322371282777625,0.0308697720520624,
-0.59250875485111));
#49843=CARTESIAN_POINT('Ctrl Pts',(-0.322110898693276,0.000285652422795598,
-0.590622655072689));
#49844=CARTESIAN_POINT('Origin',(0.,0.,-3.17777734492731));
#49845=CARTESIAN_POINT('',(-0.32183688899373,0.000172923102116511,-0.865277344927308));
#49846=CARTESIAN_POINT('',(-0.322069372535088,-0.000277835810467392,-0.840622655072689));
#49847=CARTESIAN_POINT('',(-0.322275,-1.53308031181269E-15,-3.17777734492731));
#49848=CARTESIAN_POINT('Ctrl Pts',(-0.32183688899373,0.000172923102116473,
-0.865277344927309));
#49849=CARTESIAN_POINT('Ctrl Pts',(-0.321521197468452,-0.0648015223631276,
-0.861278998513499));
#49850=CARTESIAN_POINT('Ctrl Pts',(-0.270857672103809,-0.237844790870895,
-0.850658259785309));
#49851=CARTESIAN_POINT('Ctrl Pts',(0.0117243233039672,-0.38086932973796,
-0.833415128742737));
#49852=CARTESIAN_POINT('Ctrl Pts',(0.326557088446483,-0.196365409574429,
-0.813547951799597));
#49853=CARTESIAN_POINT('Ctrl Pts',(0.341905585223924,0.168224483606484,
-0.793680774856455));
#49854=CARTESIAN_POINT('Ctrl Pts',(0.0436937654029756,0.378536340338528,
-0.773813597913315));
#49855=CARTESIAN_POINT('Ctrl Pts',(-0.259410588849515,0.255924509718627,
-0.756012454603599));
#49856=CARTESIAN_POINT('Ctrl Pts',(-0.321450647199645,0.0736612759823137,
-0.744833703608263));
#49857=CARTESIAN_POINT('Ctrl Pts',(-0.322031575383028,-0.000268584671637075,
-0.740277344927308));
#49858=CARTESIAN_POINT('Ctrl Pts',(-0.322069372535088,-0.000277835810467364,
-0.840622655072689));
#49859=CARTESIAN_POINT('Ctrl Pts',(-0.322332513972518,-0.032371167381551,
-0.838644129290342));
#49860=CARTESIAN_POINT('Ctrl Pts',(-0.303165873677557,-0.171577957634514,
-0.830043211193615));
#49861=CARTESIAN_POINT('Ctrl Pts',(-0.103035825860727,-0.366854887387893,
-0.814819900782507));
#49862=CARTESIAN_POINT('Ctrl Pts',(0.25263760185176,-0.285259762219933,
-0.794952723839366));
#49863=CARTESIAN_POINT('Ctrl Pts',(0.376618042246158,0.0579460099220519,
-0.775085546896225));
#49864=CARTESIAN_POINT('Ctrl Pts',(0.15520350324569,0.348009715944001,-0.755218369953084));
#49865=CARTESIAN_POINT('Ctrl Pts',(-0.207701459761879,0.318982707307465,
-0.735397406011905));
#49866=CARTESIAN_POINT('Ctrl Pts',(-0.322738816059344,0.106028364300782,
-0.722198834385106));
#49867=CARTESIAN_POINT('Ctrl Pts',(-0.32280575289529,-1.39830014679308E-5,
-0.715622655072688));
#49868=CARTESIAN_POINT('Origin',(0.,0.,-3.17777734492731));
#49869=CARTESIAN_POINT('',(-0.322664566790459,0.000190428865854771,-0.990277344927309));
#49870=CARTESIAN_POINT('',(-0.321815198935766,0.000153234844127104,-0.965622655072689));
#49871=CARTESIAN_POINT('',(-0.322275,-1.53308031181269E-15,-3.17777734492731));
#49872=CARTESIAN_POINT('Ctrl Pts',(-0.322664566790459,0.00019042886585479,
-0.990277344927309));
#49873=CARTESIAN_POINT('Ctrl Pts',(-0.321994453881888,-0.0955538967887449,
-0.984346685733115));
#49874=CARTESIAN_POINT('Ctrl Pts',(-0.226048562226605,-0.299375993968961,
-0.97179363422454));
#49875=CARTESIAN_POINT('Ctrl Pts',(0.12064623827576,-0.361446249505908,
-0.952618190401585));
#49876=CARTESIAN_POINT('Ctrl Pts',(0.369203465790718,-0.0942746357198006,
-0.932751013458444));
#49877=CARTESIAN_POINT('Ctrl Pts',(0.279165593881561,0.259355889242436,
-0.912883836515302));
#49878=CARTESIAN_POINT('Ctrl Pts',(-0.0668939863116134,0.375132110978679,
-0.893016659572163));
#49879=CARTESIAN_POINT('Ctrl Pts',(-0.294306079939019,0.192813503700519,
-0.87714782904283));
#49880=CARTESIAN_POINT('Ctrl Pts',(-0.322044071905618,0.0428145328125884,
-0.867901390827879));
#49881=CARTESIAN_POINT('Ctrl Pts',(-0.32183688899373,0.000172923102116473,
-0.865277344927309));
#49882=CARTESIAN_POINT('Ctrl Pts',(-0.321815198935766,0.000153234844127097,
-0.965622655072689));
#49883=CARTESIAN_POINT('Ctrl Pts',(-0.321542654537741,-0.0634098832967347,
-0.961711816509958));
#49884=CARTESIAN_POINT('Ctrl Pts',(-0.272548169464614,-0.23499467138165,
-0.951178585632847));
#49885=CARTESIAN_POINT('Ctrl Pts',(0.00669754469093416,-0.380990856460232,
-0.934022962441355));
#49886=CARTESIAN_POINT('Ctrl Pts',(0.323937501014007,-0.200657382739803,
-0.914155785498214));
#49887=CARTESIAN_POINT('Ctrl Pts',(0.34409560267971,0.163698216324051,-0.894288608555072));
#49888=CARTESIAN_POINT('Ctrl Pts',(0.0486849310371447,0.377926801512009,
-0.874421431611931));
#49889=CARTESIAN_POINT('Ctrl Pts',(-0.257508780691039,0.258742235111471,
-0.856532780451136));
#49890=CARTESIAN_POINT('Ctrl Pts',(-0.321451744134498,0.0750495365766745,
-0.845266521604723));
#49891=CARTESIAN_POINT('Ctrl Pts',(-0.322069372535088,-0.000277835810467364,
-0.840622655072689));
#49892=CARTESIAN_POINT('Origin',(0.,0.,-3.17777734492731));
#49893=CARTESIAN_POINT('',(-0.322423848909263,-0.000279534380340588,-1.11527734492731));
#49894=CARTESIAN_POINT('',(-0.322631094037432,0.000209311881509786,-1.09062265507269));
#49895=CARTESIAN_POINT('',(-0.322275,-1.53308031181269E-15,-3.17777734492731));
#49896=CARTESIAN_POINT('Ctrl Pts',(-0.322423848909263,-0.000279534380340587,
-1.11527734492731));
#49897=CARTESIAN_POINT('Ctrl Pts',(-0.322607183827066,-0.0203463362564853,
-1.11403676526711));
#49898=CARTESIAN_POINT('Ctrl Pts',(-0.311754457112276,-0.14733488942806,
-1.10617379329253));
#49899=CARTESIAN_POINT('Ctrl Pts',(-0.14313782027769,-0.353143696670534,
-1.09168842900357));
#49900=CARTESIAN_POINT('Ctrl Pts',(0.219396867869826,-0.311550831263358,
-1.07182125206043));
#49901=CARTESIAN_POINT('Ctrl Pts',(0.380723519872219,0.0157641209106834,
-1.05195407511729));
#49902=CARTESIAN_POINT('Ctrl Pts',(0.192890074506225,0.328621857533794,
-1.03208689817415));
#49903=CARTESIAN_POINT('Ctrl Pts',(-0.171842127255466,0.340101733886045,
-1.01221972123101));
#49904=CARTESIAN_POINT('Ctrl Pts',(-0.317145139018747,0.129357440676627,
-0.998283203482062));
#49905=CARTESIAN_POINT('Ctrl Pts',(-0.322742726616871,0.0113577407879511,
-0.990969078047496));
#49906=CARTESIAN_POINT('Ctrl Pts',(-0.322664566790459,0.00019042886585479,
-0.990277344927309));
#49907=CARTESIAN_POINT('Ctrl Pts',(-0.322631094037432,0.000209311881509799,
-1.09062265507269));
#49908=CARTESIAN_POINT('Ctrl Pts',(-0.321920739741796,-0.0941479609162504,
-1.08477950372957));
#49909=CARTESIAN_POINT('Ctrl Pts',(-0.228401002517511,-0.296671203383949,
-1.07231396007208));
#49910=CARTESIAN_POINT('Ctrl Pts',(0.115866267398166,-0.363006746342826,
-1.0532260241002));
#49911=CARTESIAN_POINT('Ctrl Pts',(0.367927300711469,-0.0991382428851851,
-1.03335884715706));
#49912=CARTESIAN_POINT('Ctrl Pts',(0.282563600758959,0.255649567449899,
-1.01349167021392));
#49913=CARTESIAN_POINT('Ctrl Pts',(-0.0619381067084859,0.375982128230261,
-0.99362449327078));
#49914=CARTESIAN_POINT('Ctrl Pts',(-0.293003380988379,0.19569146729556,
-0.977668154890368));
#49915=CARTESIAN_POINT('Ctrl Pts',(-0.322004165770655,0.0442242975322807,
-0.968334208824338));
#49916=CARTESIAN_POINT('Ctrl Pts',(-0.321815198935766,0.000153234844127097,
-0.965622655072689));
#49917=CARTESIAN_POINT('Origin',(0.,0.,-3.17777734492731));
#49918=CARTESIAN_POINT('',(-0.321748138662352,-3.69915658214744E-5,-1.24027734492731));
#49919=CARTESIAN_POINT('',(-0.32246593369561,-0.000270282110639619,-1.21562265507269));
#49920=CARTESIAN_POINT('',(-0.322275,-1.53308031181269E-15,-3.17777734492731));
#49921=CARTESIAN_POINT('Ctrl Pts',(-0.321748138662352,-3.69915658215321E-5,
-1.24027734492731));
#49922=CARTESIAN_POINT('Ctrl Pts',(-0.321800888129312,-0.0516330764776327,
-1.23710445248673));
#49923=CARTESIAN_POINT('Ctrl Pts',(-0.285718595171699,-0.210849744615903,
-1.22730916773176));
#49924=CARTESIAN_POINT('Ctrl Pts',(-0.0356529670902981,-0.379378138576325,
-1.21089149066242));
#49925=CARTESIAN_POINT('Ctrl Pts',(0.299650873068665,-0.235389592720591,
-1.19102431371928));
#49926=CARTESIAN_POINT('Ctrl Pts',(0.360146033027642,0.124473856638375,
-1.17115713677614));
#49927=CARTESIAN_POINT('Ctrl Pts',(0.0903526308274595,0.37018280375314,
-1.151289959833));
#49928=CARTESIAN_POINT('Ctrl Pts',(-0.240281721815781,0.28225474119053,
-1.13266336255005));
#49929=CARTESIAN_POINT('Ctrl Pts',(-0.321628515717655,0.0867731327968641,
-1.12065915758149));
#49930=CARTESIAN_POINT('Ctrl Pts',(-0.322423848909263,-0.000279534380340587,
-1.11527734492731));
#49931=CARTESIAN_POINT('Ctrl Pts',(-0.32246593369561,-0.000270282110639604,
-1.21562265507269));
#49932=CARTESIAN_POINT('Ctrl Pts',(-0.322633297964103,-0.0189153241123458,
-1.21446958326357));
#49933=CARTESIAN_POINT('Ctrl Pts',(-0.312669314181208,-0.144464950082961,
-1.20669411914007));
#49934=CARTESIAN_POINT('Ctrl Pts',(-0.147785253953922,-0.351224157091969,
-1.19229626270219));
#49935=CARTESIAN_POINT('Ctrl Pts',(0.21526668826523,-0.314418737887087,
-1.17242908575905));
#49936=CARTESIAN_POINT('Ctrl Pts',(0.38089836640381,0.0107389143816884,
-1.15256190881591));
#49937=CARTESIAN_POINT('Ctrl Pts',(0.197209596082445,0.326047948964853,
-1.13269473187277));
#49938=CARTESIAN_POINT('Ctrl Pts',(-0.167339347503859,0.342339645072217,
-1.11282755492962));
#49939=CARTESIAN_POINT('Ctrl Pts',(-0.316340318579248,0.132219940356831,
-1.0988035293296));
#49940=CARTESIAN_POINT('Ctrl Pts',(-0.322725826680619,0.0127927704611822,
-1.09140189604395));
#49941=CARTESIAN_POINT('Ctrl Pts',(-0.322631094037432,0.000209311881509799,
-1.09062265507269));
#49942=CARTESIAN_POINT('Origin',(0.,0.,-3.17777734492731));
#49943=CARTESIAN_POINT('',(-0.322287749187065,0.000295527604654457,-1.36527734492731));
#49944=CARTESIAN_POINT('',(-0.32175449810873,-6.01427031357848E-5,-1.34062265507269));
#49945=CARTESIAN_POINT('',(-0.322275,-1.53308031181269E-15,-3.17777734492731));
#49946=CARTESIAN_POINT('Ctrl Pts',(-0.322287749187065,0.000295527604654462,
-1.36527734492731));
#49947=CARTESIAN_POINT('Ctrl Pts',(-0.321524233712806,-0.0823725192591668,
-1.36017213970634));
#49948=CARTESIAN_POINT('Ctrl Pts',(-0.246991313292718,-0.273499001818416,
-1.348444542171));
#49949=CARTESIAN_POINT('Ctrl Pts',(0.0748376698498334,-0.373628464203982,
-1.33009455232127));
#49950=CARTESIAN_POINT('Ctrl Pts',(0.354642304090093,-0.139383436037601,
-1.31022737537813));
#49951=CARTESIAN_POINT('Ctrl Pts',(0.309205825124097,0.222689613141937,
-1.29036019843499));
#49952=CARTESIAN_POINT('Ctrl Pts',(-0.0198021443645707,0.380534861964767,
-1.27049302149184));
#49953=CARTESIAN_POINT('Ctrl Pts',(-0.281005665237226,0.219919384599868,
-1.25379873698929));
#49954=CARTESIAN_POINT('Ctrl Pts',(-0.32169079058547,0.056057153358656,
-1.24372684480111));
#49955=CARTESIAN_POINT('Ctrl Pts',(-0.321748138662352,-3.69915658215321E-5,
-1.24027734492731));
#49956=CARTESIAN_POINT('Ctrl Pts',(-0.32175449810873,-6.01427031357918E-5,
-1.34062265507269));
#49957=CARTESIAN_POINT('Ctrl Pts',(-0.321837987470172,-0.0502307331208825,
-1.33753727048319));
#49958=CARTESIAN_POINT('Ctrl Pts',(-0.287155063447946,-0.207976961406838,
-1.3278294935793));
#49959=CARTESIAN_POINT('Ctrl Pts',(-0.040655941181135,-0.378874628680604,
-1.31149932436104));
#49960=CARTESIAN_POINT('Ctrl Pts',(0.296518686521221,-0.239323125407717,
-1.29163214741789));
#49961=CARTESIAN_POINT('Ctrl Pts',(0.361757150437206,0.119710709290111,
-1.27176497047476));
#49962=CARTESIAN_POINT('Ctrl Pts',(0.0952295025228559,0.368958306127452,
-1.25189779353161));
#49963=CARTESIAN_POINT('Ctrl Pts',(-0.238094936424389,0.285008232302127,
-1.23318368839759));
#49964=CARTESIAN_POINT('Ctrl Pts',(-0.321672081293464,0.0881680178589641,
-1.22109197557795));
#49965=CARTESIAN_POINT('Ctrl Pts',(-0.32246593369561,-0.000270282110639604,
-1.21562265507269));
#49966=CARTESIAN_POINT('Origin',(0.,0.,-3.17777734492731));
#49967=CARTESIAN_POINT('',(-0.322751107179779,-0.000121302661654257,-1.49027734492731));
#49968=CARTESIAN_POINT('',(-0.322244723354561,0.000296369465573723,-1.46562265507269));
#49969=CARTESIAN_POINT('',(-0.322275,-1.53308031181269E-15,-3.17777734492731));
#49970=CARTESIAN_POINT('Ctrl Pts',(-0.322751107179779,-0.000121302661654219,
-1.49027734492731));
#49971=CARTESIAN_POINT('Ctrl Pts',(-0.3227833604428,-0.00681832798748842,
-1.48986221924034));
#49972=CARTESIAN_POINT('Ctrl Pts',(-0.319556406731551,-0.120319591508497,
-1.48282470123899));
#49973=CARTESIAN_POINT('Ctrl Pts',(-0.185874672239764,-0.332640214513727,
-1.46916479092326));
#49974=CARTESIAN_POINT('Ctrl Pts',(0.179018990329492,-0.336379409585943,
-1.44929761398012));
#49975=CARTESIAN_POINT('Ctrl Pts',(0.379735015238712,-0.0316263227965929,
-1.42943043703697));
#49976=CARTESIAN_POINT('Ctrl Pts',(0.232197496633113,0.302131144785331,
-1.40956326009383));
#49977=CARTESIAN_POINT('Ctrl Pts',(-0.128287466249961,0.358805284374608,
-1.38969608315069));
#49978=CARTESIAN_POINT('Ctrl Pts',(-0.308720453379187,0.156414319310542,
-1.37493411142852));
#49979=CARTESIAN_POINT('Ctrl Pts',(-0.322514654036729,0.024863177348577,
-1.36679453202072));
#49980=CARTESIAN_POINT('Ctrl Pts',(-0.322287749187065,0.000295527604654462,
-1.36527734492731));
#49981=CARTESIAN_POINT('Ctrl Pts',(-0.322244723354561,0.000296369465573685,
-1.46562265507269));
#49982=CARTESIAN_POINT('Ctrl Pts',(-0.321501222101524,-0.0809823787116948,
-1.4606049577028));
#49983=CARTESIAN_POINT('Ctrl Pts',(-0.249050437632911,-0.270713713036289,
-1.44896486801853));
#49984=CARTESIAN_POINT('Ctrl Pts',(0.0699009395453964,-0.374583433245331,
-1.43070238601989));
#49985=CARTESIAN_POINT('Ctrl Pts',(0.352772174889632,-0.144050971655273,
-1.41083520907674));
#49986=CARTESIAN_POINT('Ctrl Pts',(0.312117385430717,0.218590090175839,
-1.3909680321336));
#49987=CARTESIAN_POINT('Ctrl Pts',(-0.0147790754750554,0.380763008627795,
-1.37110085519046));
#49988=CARTESIAN_POINT('Ctrl Pts',(-0.279459402901632,0.222784460857227,
-1.35431906283682));
#49989=CARTESIAN_POINT('Ctrl Pts',(-0.321658787992924,0.0574541673355203,
-1.34415966279757));
#49990=CARTESIAN_POINT('Ctrl Pts',(-0.32175449810873,-6.01427031357918E-5,
-1.34062265507269));
#49991=CARTESIAN_POINT('Origin',(0.,0.,-3.17777734492731));
#49992=CARTESIAN_POINT('',(-0.321922168755166,-0.000227579808175941,-1.61527734492731));
#49993=CARTESIAN_POINT('',(-0.322771138341452,-9.69895275597654E-5,-1.59062265507269));
#49994=CARTESIAN_POINT('',(-0.322275,-1.53308031181269E-15,-3.17777734492731));
#49995=CARTESIAN_POINT('Ctrl Pts',(-0.321922168755166,-0.000227579808175983,
-1.61527734492731));
#49996=CARTESIAN_POINT('Ctrl Pts',(-0.322170091457483,-0.038348893149621,
-1.61292990645995));
#49997=CARTESIAN_POINT('Ctrl Pts',(-0.298262264464941,-0.183713933271471,
-1.60396007567822));
#49998=CARTESIAN_POINT('Ctrl Pts',(-0.0824785577203104,-0.372016388897528,
-1.5883678525821));
#49999=CARTESIAN_POINT('Ctrl Pts',(0.268107811741657,-0.270771319336224,
-1.56850067563896));
#50000=CARTESIAN_POINT('Ctrl Pts',(0.372813523017964,0.0787971011326718,
-1.54863349869582));
#50001=CARTESIAN_POINT('Ctrl Pts',(0.135613365066933,0.35610099874502,-1.52876632175268));
#50002=CARTESIAN_POINT('Ctrl Pts',(-0.218402258481575,0.307855623037052,
-1.50931427049651));
#50003=CARTESIAN_POINT('Ctrl Pts',(-0.322268832511024,0.100017578435714,
-1.49648461155472));
#50004=CARTESIAN_POINT('Ctrl Pts',(-0.322751107179779,-0.000121302661654219,
-1.49027734492731));
#50005=CARTESIAN_POINT('Ctrl Pts',(-0.322771138341452,-9.69895275597966E-5,
-1.59062265507269));
#50006=CARTESIAN_POINT('Ctrl Pts',(-0.32279205568065,-0.00538141795017537,
-1.5902950372368));
#50007=CARTESIAN_POINT('Ctrl Pts',(-0.320277876082452,-0.117463752275654,
-1.58334502708653));
#50008=CARTESIAN_POINT('Ctrl Pts',(-0.190247829186885,-0.330158527530134,
-1.56977262462188));
#50009=CARTESIAN_POINT('Ctrl Pts',(0.174564703217894,-0.338712347282523,
-1.54990544767873));
#50010=CARTESIAN_POINT('Ctrl Pts',(0.379284607793692,-0.0366343568522026,
-1.53003827073559));
#50011=CARTESIAN_POINT('Ctrl Pts',(0.236164035815733,0.299040863425743,
-1.51017109379245));
#50012=CARTESIAN_POINT('Ctrl Pts',(-0.123541678493353,0.360466841035667,
-1.49030391684931));
#50013=CARTESIAN_POINT('Ctrl Pts',(-0.307714925372633,0.159288869904934,
-1.47545443727605));
#50014=CARTESIAN_POINT('Ctrl Pts',(-0.322482500289682,0.0262898853514597,
-1.46722735001718));
#50015=CARTESIAN_POINT('Ctrl Pts',(-0.322244723354561,0.000296369465573685,
-1.46562265507269));
#50016=CARTESIAN_POINT('Origin',(0.,0.,-3.17777734492731));
#50017=CARTESIAN_POINT('',(-0.321923856749615,0.00022841188425891,-1.74027734492731));
#50018=CARTESIAN_POINT('',(-0.321953965388694,-0.000242065591690599,-1.71562265507269));
#50019=CARTESIAN_POINT('',(-0.322275,-1.53308031181269E-15,-3.17777734492731));
#50020=CARTESIAN_POINT('Ctrl Pts',(-0.321923856749615,0.000228411884258914,
-1.74027734492731));
#50021=CARTESIAN_POINT('Ctrl Pts',(-0.321470050673185,-0.0692718503800838,
-1.73599759367957));
#50022=CARTESIAN_POINT('Ctrl Pts',(-0.265230516068486,-0.246984636511405,
-1.72509545011745));
#50023=CARTESIAN_POINT('Ctrl Pts',(0.0278710512479263,-0.380029091773661,
-1.70757091424095));
#50024=CARTESIAN_POINT('Ctrl Pts',(0.334593350165504,-0.182335394580983,
-1.68770373729781));
#50025=CARTESIAN_POINT('Ctrl Pts',(0.334461355547943,0.182577402043658,
-1.66783656035467));
#50026=CARTESIAN_POINT('Ctrl Pts',(0.0275961191588265,0.380049155109377,
-1.64796938341153));
#50027=CARTESIAN_POINT('Ctrl Pts',(-0.265328911815288,0.246829175329326,
-1.63044964493574));
#50028=CARTESIAN_POINT('Ctrl Pts',(-0.321470673167627,0.0691956904453584,
-1.61955229877433));
#50029=CARTESIAN_POINT('Ctrl Pts',(-0.321922168755166,-0.000227579808175983,
-1.61527734492731));
#50030=CARTESIAN_POINT('Ctrl Pts',(-0.321953965388694,-0.000242065591690606,
-1.71562265507269));
#50031=CARTESIAN_POINT('Ctrl Pts',(-0.322209458649345,-0.0369331731931518,
-1.71336272445641));
#50032=CARTESIAN_POINT('Ctrl Pts',(-0.299463487975333,-0.180834904933275,
-1.70448040152576));
#50033=CARTESIAN_POINT('Ctrl Pts',(-0.0873803104607973,-0.370895633777163,
-1.68897568628072));
#50034=CARTESIAN_POINT('Ctrl Pts',(0.264511494039161,-0.27428554342575,
-1.66910850933758));
#50035=CARTESIAN_POINT('Ctrl Pts',(0.373820809690602,0.0738707794290245,
-1.64924133239444));
#50036=CARTESIAN_POINT('Ctrl Pts',(0.140300477324218,0.354280490393961,
-1.6293741554513));
#50037=CARTESIAN_POINT('Ctrl Pts',(-0.215916241007796,0.310514722383114,
-1.60983459634405));
#50038=CARTESIAN_POINT('Ctrl Pts',(-0.322369237350371,0.10143681456936,
-1.59691742955118));
#50039=CARTESIAN_POINT('Ctrl Pts',(-0.322771138341452,-9.69895275597966E-5,
-1.59062265507269));
#50040=CARTESIAN_POINT('Origin',(0.,0.,-3.17777734492731));
#50041=CARTESIAN_POINT('',(-0.3227523074527,0.000119995480296377,-1.86527734492731));
#50042=CARTESIAN_POINT('',(-0.32189411998726,0.000212574305966731,-1.84062265507269));
#50043=CARTESIAN_POINT('',(-0.322275,-1.53308031181269E-15,-3.17777734492731));
#50044=CARTESIAN_POINT('Ctrl Pts',(-0.3227523074527,0.000119995480296356,
-1.86527734492731));
#50045=CARTESIAN_POINT('Ctrl Pts',(-0.322274164449301,-0.1000952891468,
-1.85906528089919));
#50046=CARTESIAN_POINT('Ctrl Pts',(-0.218266807444085,-0.308001705979866,
-1.84623082455668));
#50047=CARTESIAN_POINT('Ctrl Pts',(0.13587094405367,-0.356002798660267,
-1.8267739758998));
#50048=CARTESIAN_POINT('Ctrl Pts',(0.372870429720997,-0.0785273756829916,
-1.80690679895666));
#50049=CARTESIAN_POINT('Ctrl Pts',(0.267911857239273,0.270965205963022,
-1.78703962201352));
#50050=CARTESIAN_POINT('Ctrl Pts',(-0.0827476642965211,0.371956624010715,
-1.76717244507038));
#50051=CARTESIAN_POINT('Ctrl Pts',(-0.298328740556997,0.183556097792722,
-1.75158501937497));
#50052=CARTESIAN_POINT('Ctrl Pts',(-0.322172260147241,0.0382713165060726,
-1.74261998599395));
#50053=CARTESIAN_POINT('Ctrl Pts',(-0.321923856749615,0.000228411884258914,
-1.74027734492731));
#50054=CARTESIAN_POINT('Ctrl Pts',(-0.32189411998726,0.000212574305966721,
-1.84062265507269));
#50055=CARTESIAN_POINT('Ctrl Pts',(-0.321482807742295,-0.067882398119342,
-1.83643041167603));
#50056=CARTESIAN_POINT('Ctrl Pts',(-0.267011798870114,-0.244146878061487,
-1.82561577596499));
#50057=CARTESIAN_POINT('Ctrl Pts',(0.0228539532777633,-0.380363755674442,
-1.80817874793957));
#50058=CARTESIAN_POINT('Ctrl Pts',(0.332158195524763,-0.186734632451837,
-1.78831157099643));
#50059=CARTESIAN_POINT('Ctrl Pts',(0.336841415329915,0.178148114583703,
-1.76844439405329));
#50060=CARTESIAN_POINT('Ctrl Pts',(0.0326086495564207,0.379651900805587,
-1.74857721711014));
#50061=CARTESIAN_POINT('Ctrl Pts',(-0.263520523765027,0.249662771554132,
-1.73096997078328));
#50062=CARTESIAN_POINT('Ctrl Pts',(-0.321460773449221,0.0705846891854826,
-1.71998511677079));
#50063=CARTESIAN_POINT('Ctrl Pts',(-0.321953965388694,-0.000242065591690606,
-1.71562265507269));
#50064=CARTESIAN_POINT('Origin',(0.,0.,-3.17777734492731));
#50065=CARTESIAN_POINT('',(-0.32228538328799,-0.000295626100757004,-1.99027734492731));
#50066=CARTESIAN_POINT('',(-0.322728660521504,0.000143315081735037,-1.96562265507269));
#50067=CARTESIAN_POINT('',(-0.322275,-1.53308031181269E-15,-3.17777734492731));
#50068=CARTESIAN_POINT('Ctrl Pts',(-0.32228538328799,-0.000295626100757031,
-1.99027734492731));
#50069=CARTESIAN_POINT('Ctrl Pts',(-0.32251292564102,-0.0249414224581168,
-1.98875536043318));
#50070=CARTESIAN_POINT('Ctrl Pts',(-0.308665902992896,-0.156571884968343,
-1.98061098362468));
#50071=CARTESIAN_POINT('Ctrl Pts',(-0.128027861842815,-0.358897997603687,
-1.96584421450179));
#50072=CARTESIAN_POINT('Ctrl Pts',(0.232416006884924,-0.301963086875939,
-1.94597703755865));
#50073=CARTESIAN_POINT('Ctrl Pts',(0.37971203641127,0.0319010265725857,
-1.9261098606155));
#50074=CARTESIAN_POINT('Ctrl Pts',(0.178775596218371,0.336508829436531,
-1.90624268367236));
#50075=CARTESIAN_POINT('Ctrl Pts',(-0.18611526581757,0.332505659984359,
-1.88637550672922));
#50076=CARTESIAN_POINT('Ctrl Pts',(-0.319596470562309,0.120162984611006,
-1.8727203938142));
#50077=CARTESIAN_POINT('Ctrl Pts',(-0.322783890449637,0.00673956118529448,
-1.86568767321357));
#50078=CARTESIAN_POINT('Ctrl Pts',(-0.3227523074527,0.000119995480296356,
-1.86527734492731));
#50079=CARTESIAN_POINT('Ctrl Pts',(-0.322728660521503,0.000143315081735021,
-1.96562265507269));
#50080=CARTESIAN_POINT('Ctrl Pts',(-0.32218001068861,-0.0986794523285048,
-1.95949809889565));
#50081=CARTESIAN_POINT('Ctrl Pts',(-0.220722265880929,-0.305331620279144,
-1.94675115040422));
#50082=CARTESIAN_POINT('Ctrl Pts',(0.131161475792397,-0.357764667175434,
-1.92738180959841));
#50083=CARTESIAN_POINT('Ctrl Pts',(0.371801737976828,-0.0834407421383482,
-1.90751463265528));
#50084=CARTESIAN_POINT('Ctrl Pts',(0.271464035161107,0.267406371325063,
-1.88764745571213));
#50085=CARTESIAN_POINT('Ctrl Pts',(-0.0778323056202418,0.373016114950851,
-1.86778027876899));
#50086=CARTESIAN_POINT('Ctrl Pts',(-0.297104761464683,0.18643508125568,
-1.85210534522251));
#50087=CARTESIAN_POINT('Ctrl Pts',(-0.322132548416235,0.0396856935607706,
-1.84305280399041));
#50088=CARTESIAN_POINT('Ctrl Pts',(-0.32189411998726,0.000212574305966721,
-1.84062265507269));
#50089=CARTESIAN_POINT('Origin',(0.,0.,-3.17777734492731));
#50090=CARTESIAN_POINT('',(-0.321748409289639,3.82678754979511E-5,-2.11527734492731));
#50091=CARTESIAN_POINT('',(-0.322328587652096,-0.00029287054778171,-2.09062265507269));
#50092=CARTESIAN_POINT('',(-0.322275,-1.53308031181269E-15,-3.17777734492731));
#50093=CARTESIAN_POINT('Ctrl Pts',(-0.321748409289639,3.82678754979639E-5,
-2.11527734492731));
#50094=CARTESIAN_POINT('Ctrl Pts',(-0.32168899726537,-0.0561337723056524,
-2.1118230476528));
#50095=CARTESIAN_POINT('Ctrl Pts',(-0.280921590087898,-0.220076513828276,
-2.10174635806391));
#50096=CARTESIAN_POINT('Ctrl Pts',(-0.0195268484971016,-0.380549087871386,
-2.08504727616063));
#50097=CARTESIAN_POINT('Ctrl Pts',(0.309366844764242,-0.222465865814493,
-2.06518009921749));
#50098=CARTESIAN_POINT('Ctrl Pts',(0.354541377001136,0.139639958772985,
-2.04531292227435));
#50099=CARTESIAN_POINT('Ctrl Pts',(0.0745673558825864,0.373682506318743,
-2.02544574533121));
#50100=CARTESIAN_POINT('Ctrl Pts',(-0.247104986648104,0.273346487692639,
-2.0071005528822));
#50101=CARTESIAN_POINT('Ctrl Pts',(-0.321522853313923,0.0822962879184196,
-1.99537775274756));
#50102=CARTESIAN_POINT('Ctrl Pts',(-0.32228538328799,-0.000295626100757031,
-1.99027734492731));
#50103=CARTESIAN_POINT('Ctrl Pts',(-0.322328587652096,-0.000292870547781703,
-2.09062265507269));
#50104=CARTESIAN_POINT('Ctrl Pts',(-0.322543800094343,-0.0235136571889884,
-2.08918817842964));
#50105=CARTESIAN_POINT('Ctrl Pts',(-0.309650508248358,-0.153698251766603,
-2.08113130947221));
#50106=CARTESIAN_POINT('Ctrl Pts',(-0.132752542720296,-0.357177340004209,
-2.0664520482004));
#50107=CARTESIAN_POINT('Ctrl Pts',(0.228411208027658,-0.305003622697395,
-2.04658487125726));
#50108=CARTESIAN_POINT('Ctrl Pts',(0.380099905430515,0.0268877612103093,
-2.02671769431412));
#50109=CARTESIAN_POINT('Ctrl Pts',(0.183200419906357,0.334120481200005,
-2.00685051737098));
#50110=CARTESIAN_POINT('Ctrl Pts',(-0.181711476497752,0.334932573990939,
-1.98698334042784));
#50111=CARTESIAN_POINT('Ctrl Pts',(-0.318856304620057,0.123020370421255,
-1.97324071966174));
#50112=CARTESIAN_POINT('Ctrl Pts',(-0.32277325766547,0.0081761493616704,
-1.96612049121003));
#50113=CARTESIAN_POINT('Ctrl Pts',(-0.322728660521503,0.000143315081735021,
-1.96562265507269));
#50114=CARTESIAN_POINT('Origin',(0.,0.,-3.17777734492731));
#50115=CARTESIAN_POINT('',(-0.322426177028279,0.000279078778166078,-2.24027734492731));
#50116=CARTESIAN_POINT('',(-0.321744902911595,1.49008663381245E-5,-2.21562265507269));
#50117=CARTESIAN_POINT('',(-0.322275,-1.53308031181269E-15,-3.17777734492731));
#50118=CARTESIAN_POINT('Ctrl Pts',(-0.322426177028279,0.000279078778166082,
-2.24027734492731));
#50119=CARTESIAN_POINT('Ctrl Pts',(-0.321630768589567,-0.0868495651447256,
-2.23489073487241));
#50120=CARTESIAN_POINT('Ctrl Pts',(-0.240162640512569,-0.282405909728632,
-2.22288173250314));
#50121=CARTESIAN_POINT('Ctrl Pts',(0.090620408871829,-0.370117342997772,
-2.20425033781948));
#50122=CARTESIAN_POINT('Ctrl Pts',(0.360235987022344,-0.124213283290337,
-2.18438316087634));
#50123=CARTESIAN_POINT('Ctrl Pts',(0.299480506547509,0.235606307831963,
-2.1645159839332));
#50124=CARTESIAN_POINT('Ctrl Pts',(-0.0359274116371167,0.379352246843221,
-2.14464880699006));
#50125=CARTESIAN_POINT('Ctrl Pts',(-0.285798019731171,0.210692290217066,
-2.12823592732143));
#50126=CARTESIAN_POINT('Ctrl Pts',(-0.321802898791972,0.0515562316565445,
-2.11844543996718));
#50127=CARTESIAN_POINT('Ctrl Pts',(-0.321748409289639,3.82678754979639E-5,
-2.11527734492731));
#50128=CARTESIAN_POINT('Ctrl Pts',(-0.321744902911595,1.49008663381453E-5,
-2.21562265507269));
#50129=CARTESIAN_POINT('Ctrl Pts',(-0.321722368475626,-0.0547356078121411,
-2.21225586564926));
#50130=CARTESIAN_POINT('Ctrl Pts',(-0.282442567683545,-0.217209365600774,
-2.20226668391144));
#50131=CARTESIAN_POINT('Ctrl Pts',(-0.0245466787495387,-0.380258267988377,
-2.18565510985925));
#50132=CARTESIAN_POINT('Ctrl Pts',(0.306404346658912,-0.226528731422051,
-2.16578793291611));
#50133=CARTESIAN_POINT('Ctrl Pts',(0.356353106829473,0.134949446327866,
-2.14592075597297));
#50134=CARTESIAN_POINT('Ctrl Pts',(0.0794917830842547,0.372665998225311,
-2.12605357902982));
#50135=CARTESIAN_POINT('Ctrl Pts',(-0.245017099497695,0.276125023901044,
-2.10762087872974));
#50136=CARTESIAN_POINT('Ctrl Pts',(-0.321550252217212,0.0836872231681876,
-2.09581057074402));
#50137=CARTESIAN_POINT('Ctrl Pts',(-0.322328587652096,-0.000292870547781703,
-2.09062265507269));
#50138=CARTESIAN_POINT('Origin',(0.,0.,-3.17777734492731));
#50139=CARTESIAN_POINT('',(-0.322662798805829,-0.000191504950135908,-2.36527734492731));
#50140=CARTESIAN_POINT('',(-0.322383419286056,0.000286438788401844,-2.34062265507269));
#50141=CARTESIAN_POINT('',(-0.322275,-1.53308031181269E-15,-3.17777734492731));
#50142=CARTESIAN_POINT('Ctrl Pts',(-0.322662798805829,-0.00019150495013591,
-2.36527734492731));
#50143=CARTESIAN_POINT('Ctrl Pts',(-0.322741850192619,-0.0114364278866111,
-2.36458081440641));
#50144=CARTESIAN_POINT('Ctrl Pts',(-0.317101545247626,-0.129514330580757,
-2.35726189157113));
#50145=CARTESIAN_POINT('Ctrl Pts',(-0.171596042253934,-0.340225960835699,
-2.34332057642147));
#50146=CARTESIAN_POINT('Ctrl Pts',(0.193127759284308,-0.328482228877282,
-2.32345339947833));
#50147=CARTESIAN_POINT('Ctrl Pts',(0.380734824477702,-0.0154886896292257,
-2.30358622253519));
#50148=CARTESIAN_POINT('Ctrl Pts',(0.219171424964897,0.311709468221516,
-2.28371904559205));
#50149=CARTESIAN_POINT('Ctrl Pts',(-0.143393257897354,0.353040053933262,
-2.2638518686489));
#50150=CARTESIAN_POINT('Ctrl Pts',(-0.311805167411146,0.147177520159949,
-2.24937130176066));
#50151=CARTESIAN_POINT('Ctrl Pts',(-0.322608657591674,0.0202679087390474,
-2.24151312718679));
#50152=CARTESIAN_POINT('Ctrl Pts',(-0.322426177028279,0.000279078778166082,
-2.24027734492731));
#50153=CARTESIAN_POINT('Ctrl Pts',(-0.322383419286056,0.000286438788401826,
-2.34062265507269));
#50154=CARTESIAN_POINT('Ctrl Pts',(-0.321592096098541,-0.0854560343740861,
-2.33532355286887));
#50155=CARTESIAN_POINT('Ctrl Pts',(-0.242320152705578,-0.279644670426524,
-2.32340205835068));
#50156=CARTESIAN_POINT('Ctrl Pts',(0.0857286345377398,-0.371280878892406,
-2.3048581715181));
#50157=CARTESIAN_POINT('Ctrl Pts',(0.358565548084728,-0.128955951921072,
-2.28499099457496));
#50158=CARTESIAN_POINT('Ctrl Pts',(0.302563356235795,0.231633989897339,
-2.26512381763181));
#50159=CARTESIAN_POINT('Ctrl Pts',(-0.0309185430950134,0.379793277328495,
-2.24525664068868));
#50160=CARTESIAN_POINT('Ctrl Pts',(-0.284336907323424,0.213563599955149,
-2.22875625316897));
#50161=CARTESIAN_POINT('Ctrl Pts',(-0.321766693159115,0.0529573014494938,
-2.21887825796364));
#50162=CARTESIAN_POINT('Ctrl Pts',(-0.321744902911595,1.49008663381453E-5,
-2.21562265507269));
#50163=CARTESIAN_POINT('Origin',(0.,0.,-3.17777734492731));
#50164=CARTESIAN_POINT('',(-0.321835633176319,-0.000171871078531275,-2.49027734492731));
#50165=CARTESIAN_POINT('',(-0.322693718878697,-0.000171168389977605,-2.46562265507269));
#50166=CARTESIAN_POINT('',(-0.322275,-1.53308031181269E-15,-3.17777734492731));
#50167=CARTESIAN_POINT('Ctrl Pts',(-0.321835633176319,-0.000171871078531286,
-2.49027734492731));
#50168=CARTESIAN_POINT('Ctrl Pts',(-0.322041881997969,-0.042891857212214,
-2.48764850162603));
#50169=CARTESIAN_POINT('Ctrl Pts',(-0.294235300856302,-0.192971292817336,
-2.47839726601036));
#50170=CARTESIAN_POINT('Ctrl Pts',(-0.066622590386437,-0.375180407854742,
-2.46252363808032));
#50171=CARTESIAN_POINT('Ctrl Pts',(0.279353148857915,-0.259153863380453,
-2.44265646113718));
#50172=CARTESIAN_POINT('Ctrl Pts',(0.369135166970047,0.0945417037460469,
-2.42278928419404));
#50173=CARTESIAN_POINT('Ctrl Pts',(0.120384725846265,0.361533434408456,
-2.40292210725089));
#50174=CARTESIAN_POINT('Ctrl Pts',(-0.226178354733955,0.29922797675211,
-2.38375146082865));
#50175=CARTESIAN_POINT('Ctrl Pts',(-0.321990254561689,0.0954767496352355,
-2.37120320672079));
#50176=CARTESIAN_POINT('Ctrl Pts',(-0.322662798805829,-0.00019150495013591,
-2.36527734492731));
#50177=CARTESIAN_POINT('Ctrl Pts',(-0.322693718878697,-0.000171168389977631,
-2.46562265507269));
#50178=CARTESIAN_POINT('Ctrl Pts',(-0.322756909832245,-0.0100008653975118,
-2.46501363240287));
#50179=CARTESIAN_POINT('Ctrl Pts',(-0.317887136349063,-0.126653283447023,
-2.45778221741867));
#50180=CARTESIAN_POINT('Ctrl Pts',(-0.176070541289752,-0.337932026630971,
-2.44392841012009));
#50181=CARTESIAN_POINT('Ctrl Pts',(0.188776450434642,-0.331002026615422,
-2.42406123317694));
#50182=CARTESIAN_POINT('Ctrl Pts',(0.380497273760583,-0.0205113226115502,
-2.40419405623381));
#50183=CARTESIAN_POINT('Ctrl Pts',(0.223265489718655,0.308790237805464,
-2.38432687929066));
#50184=CARTESIAN_POINT('Ctrl Pts',(-0.13872222919299,0.354901441165425,
-2.36445970234752));
#50185=CARTESIAN_POINT('Ctrl Pts',(-0.310869984589673,0.150048604980915,
-2.3498916276082));
#50186=CARTESIAN_POINT('Ctrl Pts',(-0.322581028259807,0.0216980218126806,
-2.34194594518325));
#50187=CARTESIAN_POINT('Ctrl Pts',(-0.322383419286056,0.000286438788401826,
-2.34062265507269));
#50188=CARTESIAN_POINT('Origin',(0.,0.,-3.17777734492731));
#50189=CARTESIAN_POINT('',(-0.322033807694356,0.000269037653784302,-2.61527734492731));
#50190=CARTESIAN_POINT('',(-0.321859793408538,-0.000190557072052594,-2.59062265507269));
#50191=CARTESIAN_POINT('',(-0.322275,-1.53308031181269E-15,-3.17777734492731));
#50192=CARTESIAN_POINT('Ctrl Pts',(-0.322033807694356,0.000269037653784287,
-2.61527734492731));
#50193=CARTESIAN_POINT('Ctrl Pts',(-0.321450758150024,-0.0737374573484295,
-2.61071618884564));
#50194=CARTESIAN_POINT('Ctrl Pts',(-0.259306789923588,-0.256078975821658,
-2.59953264044959));
#50195=CARTESIAN_POINT('Ctrl Pts',(0.0439674142038161,-0.378504723556717,
-2.58172669973917));
#50196=CARTESIAN_POINT('Ctrl Pts',(0.342027290992345,-0.167977046624136,
-2.56185952279602));
#50197=CARTESIAN_POINT('Ctrl Pts',(0.32641489581436,0.196601574673756,-2.54199234585288));
#50198=CARTESIAN_POINT('Ctrl Pts',(0.0114488138936679,0.380877724874727,
-2.52212516890974));
#50199=CARTESIAN_POINT('Ctrl Pts',(-0.270951082513467,0.23768862691842,
-2.50488683526788));
#50200=CARTESIAN_POINT('Ctrl Pts',(-0.321522314851962,0.0647252486472288,
-2.49427089394041));
#50201=CARTESIAN_POINT('Ctrl Pts',(-0.321835633176319,-0.000171871078531286,
-2.49027734492731));
#50202=CARTESIAN_POINT('Ctrl Pts',(-0.321859793408538,-0.000190557072052674,
-2.59062265507269));
#50203=CARTESIAN_POINT('Ctrl Pts',(-0.322081837109745,-0.0414807282665668,
-2.58808131962248));
#50204=CARTESIAN_POINT('Ctrl Pts',(-0.295514570226463,-0.190092842203374,
-2.5789175918579));
#50205=CARTESIAN_POINT('Ctrl Pts',(-0.0715674996361506,-0.374268611298861,
-2.56313147177894));
#50206=CARTESIAN_POINT('Ctrl Pts',(0.275909162196494,-0.262817483673361,
-2.54326429483579));
#50207=CARTESIAN_POINT('Ctrl Pts',(0.370350525192519,0.0896625461742955,
-2.52339711789266));
#50208=CARTESIAN_POINT('Ctrl Pts',(0.125144851946343,0.359913403121745,
-2.5035299409495));
#50209=CARTESIAN_POINT('Ctrl Pts',(-0.223795756394066,0.301922936457637,
-2.4842717866762));
#50210=CARTESIAN_POINT('Ctrl Pts',(-0.322069783874789,0.0968853198647176,
-2.47163602471725));
#50211=CARTESIAN_POINT('Ctrl Pts',(-0.322693718878697,-0.000171168389977631,
-2.46562265507269));
#50212=CARTESIAN_POINT('Origin',(0.,0.,-3.17777734492731));
#50213=CARTESIAN_POINT('',(-0.322809309401469,3.43315038937645E-5,-2.74027734492731));
#50214=CARTESIAN_POINT('',(-0.321998819203686,0.000257793408019194,-2.71562265507269));
#50215=CARTESIAN_POINT('',(-0.322275,-1.53308031181269E-15,-3.17777734492731));
#50216=CARTESIAN_POINT('Ctrl Pts',(-0.322809858836148,3.43668072568986E-5,
-2.74027734492731));
#50217=CARTESIAN_POINT('Ctrl Pts',(-0.322638450561074,-0.104681964129316,
-2.73378387606526));
#50218=CARTESIAN_POINT('Ctrl Pts',(-0.210133729114781,-0.316498876460796,
-2.72066801488882));
#50219=CARTESIAN_POINT('Ctrl Pts',(0.150841923458968,-0.349922901607075,
-2.70092976139801));
#50220=CARTESIAN_POINT('Ctrl Pts',(0.375870812198945,-0.0626363718479885,
-2.68106258445487));
#50221=CARTESIAN_POINT('Ctrl Pts',(0.256173277980071,0.282085432090484,
-2.66119540751173));
#50222=CARTESIAN_POINT('Ctrl Pts',(-0.0984510634044162,0.368112092752765,
-2.64132823056859));
#50223=CARTESIAN_POINT('Ctrl Pts',(-0.302103077194693,0.174298307700632,
-2.62602220970711));
#50224=CARTESIAN_POINT('Ctrl Pts',(-0.322297294149265,0.0337133807596303,
-2.61733858116002));
#50225=CARTESIAN_POINT('Ctrl Pts',(-0.322033807694356,0.000269037653784287,
-2.61527734492731));
#50226=CARTESIAN_POINT('Ctrl Pts',(-0.321998819203686,0.000257793408019166,
-2.71562265507269));
#50227=CARTESIAN_POINT('Ctrl Pts',(-0.321453931795426,-0.072349355039821,
-2.7111490068421));
#50228=CARTESIAN_POINT('Ctrl Pts',(-0.261178988720823,-0.253255718009303,
-2.70005296629713));
#50229=CARTESIAN_POINT('Ctrl Pts',(0.0389678303295289,-0.379052262416539,
-2.68233453343778));
#50230=CARTESIAN_POINT('Ctrl Pts',(0.339781580148665,-0.172475450822871,
-2.66246735649464));
#50231=CARTESIAN_POINT('Ctrl Pts',(0.32898038540163,0.192277148854254,-2.6426001795515));
#50232=CARTESIAN_POINT('Ctrl Pts',(0.0164738552685434,0.380693518847251,
-2.62273300260836));
#50233=CARTESIAN_POINT('Ctrl Pts',(-0.269234143322179,0.240535337111991,
-2.60540716111542));
#50234=CARTESIAN_POINT('Ctrl Pts',(-0.321503219871233,0.0661161308398998,
-2.59470371193687));
#50235=CARTESIAN_POINT('Ctrl Pts',(-0.321859793408538,-0.000190557072052674,
-2.59062265507269));
#50236=CARTESIAN_POINT('Origin',(5.160062080289E-17,2.1385152528819E-17,
-0.04));
#50237=CARTESIAN_POINT('Ctrl Pts',(0.258434353604258,0.193455249693963,
-0.0400000000000002));
#50238=CARTESIAN_POINT('Ctrl Pts',(0.254935552790794,0.199417319786304,
-0.0400000000000001));
#50239=CARTESIAN_POINT('Ctrl Pts',(0.251237159329282,0.205249124536648,
-0.0400000000000005));
#50240=CARTESIAN_POINT('Ctrl Pts',(0.247341514049974,0.21093929920956,-0.0400000000000005));
#50241=CARTESIAN_POINT('Ctrl Pts',(0.238878778768656,0.223300394357799,
-0.0400000000000004));
#50242=CARTESIAN_POINT('Ctrl Pts',(0.229486688116491,0.234993819321299,
-0.0399999999999996));
#50243=CARTESIAN_POINT('Ctrl Pts',(0.219284430274965,0.24599200395083,-0.0399999999999995));
#50244=CARTESIAN_POINT('Ctrl Pts',(0.215221055483291,0.250372381987926,
-0.0399999999999995));
#50245=CARTESIAN_POINT('Ctrl Pts',(0.211028923384398,0.254642373102135,
-0.0399999999999999));
#50246=CARTESIAN_POINT('Ctrl Pts',(0.206714685254849,0.258799772813936,
-0.0399999999999998));
#50247=CARTESIAN_POINT('Ctrl Pts',(0.202264841585829,0.263087848305281,
-0.0399999999999998));
#50248=CARTESIAN_POINT('Ctrl Pts',(0.197691588390428,0.267249800115209,
-0.0400000000000002));
#50249=CARTESIAN_POINT('Ctrl Pts',(0.193005768999244,0.271281678715959,
-0.0400000000000001));
#50250=CARTESIAN_POINT('Ctrl Pts',(0.183472268352816,0.279484708759944,
-0.0400000000000001));
#50251=CARTESIAN_POINT('Ctrl Pts',(0.173470125375889,0.287152749594996,
-0.0399999999999997));
#50252=CARTESIAN_POINT('Ctrl Pts',(0.163063775287283,0.294268502238259,
-0.0399999999999998));
#50253=CARTESIAN_POINT('Ctrl Pts',(0.156857205698134,0.298512489186952,
-0.0399999999999998));
#50254=CARTESIAN_POINT('Ctrl Pts',(0.150506682275409,0.30255992574958,-0.0400000000000011));
#50255=CARTESIAN_POINT('Ctrl Pts',(0.144024608694813,0.306406173056219,
-0.0400000000000014));
#50256=CARTESIAN_POINT('Ctrl Pts',(0.13801492013987,0.309972122768266,-0.0400000000000016));
#50257=CARTESIAN_POINT('Ctrl Pts',(0.131889073078277,0.313366371281921,
-0.0400000000000001));
#50258=CARTESIAN_POINT('Ctrl Pts',(0.125679686933379,0.316573570273351,
-0.0400000000000002));
#50259=CARTESIAN_POINT('Ctrl Pts',(0.107830520217822,0.325792811620591,
-0.0400000000000006));
#50260=CARTESIAN_POINT('Ctrl Pts',(0.0892595211029016,0.333491457102897,
-0.0400000000000009));
#50261=CARTESIAN_POINT('Ctrl Pts',(0.0702059907982684,0.33959923982706,
-0.040000000000001));
#50262=CARTESIAN_POINT('Ctrl Pts',(0.0580714236002871,0.343489085892962,
-0.0400000000000011));
#50263=CARTESIAN_POINT('Ctrl Pts',(0.0457401932381266,0.346733050166134,
-0.0400000000000004));
#50264=CARTESIAN_POINT('Ctrl Pts',(0.0332675301001174,0.349304263700216,
-0.0400000000000004));
#50265=CARTESIAN_POINT('Ctrl Pts',(0.0265485814021288,0.350689360983445,
-0.0400000000000004));
#50266=CARTESIAN_POINT('Ctrl Pts',(0.0197885224519527,0.351879102946484,
-0.0400000000000001));
#50267=CARTESIAN_POINT('Ctrl Pts',(0.0129956579817659,0.352868294018133,
-0.0400000000000001));
#50268=CARTESIAN_POINT('Ctrl Pts',(0.00804678818067408,0.353588958745581,
-0.0400000000000001));
#50269=CARTESIAN_POINT('Ctrl Pts',(0.00308158879209203,0.354202813440212,
-0.0400000000000002));
#50270=CARTESIAN_POINT('Ctrl Pts',(-0.00188381180052424,0.354706990746059,
-0.0400000000000001));
#50271=CARTESIAN_POINT('Ctrl Pts',(-0.0172998207958895,0.356272302897055,
-0.0399999999999999));
#50272=CARTESIAN_POINT('Ctrl Pts',(-0.0327495771761552,0.356786600192842,
-0.0399999999999995));
#50273=CARTESIAN_POINT('Ctrl Pts',(-0.0481326344100983,0.356212876732489,
-0.0399999999999997));
#50274=CARTESIAN_POINT('Ctrl Pts',(-0.0637031171152668,0.355632163088827,
-0.0399999999999999));
#50275=CARTESIAN_POINT('Ctrl Pts',(-0.0792056774455648,0.353937153629172,
-0.0399999999999999));
#50276=CARTESIAN_POINT('Ctrl Pts',(-0.0945633679186374,0.351199965874531,
-0.0399999999999999));
#50277=CARTESIAN_POINT('Ctrl Pts',(-0.101975271573269,0.34987894876212,
-0.04));
#50278=CARTESIAN_POINT('Ctrl Pts',(-0.109353466694925,0.348314883920549,
-0.0400000000000002));
#50279=CARTESIAN_POINT('Ctrl Pts',(-0.116689311574246,0.346514258971721,
-0.0400000000000003));
#50280=CARTESIAN_POINT('Ctrl Pts',(-0.124329759338377,0.344638867508211,
-0.0400000000000004));
#50281=CARTESIAN_POINT('Ctrl Pts',(-0.131930906052299,0.342504388350935,
-0.0399999999999999));
#50282=CARTESIAN_POINT('Ctrl Pts',(-0.139446701840371,0.340129574738105,
-0.0399999999999998));
#50283=CARTESIAN_POINT('Ctrl Pts',(-0.159130311566537,0.333910019863884,
-0.0399999999999996));
#50284=CARTESIAN_POINT('Ctrl Pts',(-0.178265201866502,0.326040008951898,
-0.0399999999999999));
#50285=CARTESIAN_POINT('Ctrl Pts',(-0.196681848896184,0.316683365411485,
-0.0399999999999997));
#50286=CARTESIAN_POINT('Ctrl Pts',(-0.213113725529896,0.308335091585425,
-0.0399999999999996));
#50287=CARTESIAN_POINT('Ctrl Pts',(-0.228974568785446,0.298802296753521,
-0.04));
#50288=CARTESIAN_POINT('Ctrl Pts',(-0.244138579475071,0.288168648000194,
-0.0399999999999999));
#50289=CARTESIAN_POINT('Ctrl Pts',(-0.248431468701942,0.285158291630113,
-0.0399999999999999));
#50290=CARTESIAN_POINT('Ctrl Pts',(-0.252668440607336,0.282059536997446,
-0.0399999999999993));
#50291=CARTESIAN_POINT('Ctrl Pts',(-0.256846437163618,0.278873893021272,
-0.0399999999999991));
#50292=CARTESIAN_POINT('Ctrl Pts',(-0.260954469218941,0.275741595664231,
-0.039999999999999));
#50293=CARTESIAN_POINT('Ctrl Pts',(-0.264998315768473,0.272530722669869,
-0.0399999999999999));
#50294=CARTESIAN_POINT('Ctrl Pts',(-0.268973925848638,0.269244900831608,
-0.0399999999999999));
#50295=CARTESIAN_POINT('Ctrl Pts',(-0.286388122571056,0.254852154376976,
-0.0400000000000002));
#50296=CARTESIAN_POINT('Ctrl Pts',(-0.302504949569424,0.239018084297059,
-0.0400000000000004));
#50297=CARTESIAN_POINT('Ctrl Pts',(-0.317110814018719,0.221907185131117,
-0.0399999999999999));
#50298=CARTESIAN_POINT('Ctrl Pts',(-0.33092057051697,0.205728933459118,
-0.0399999999999994));
#50299=CARTESIAN_POINT('Ctrl Pts',(-0.343380775179789,0.188408133777718,
-0.0400000000000002));
#50300=CARTESIAN_POINT('Ctrl Pts',(-0.354281586312166,0.170043374953611,
-0.0400000000000005));
#50301=CARTESIAN_POINT('Ctrl Pts',(-0.354909998725984,0.168984679203204,
-0.0400000000000005));
#50302=CARTESIAN_POINT('Ctrl Pts',(-0.355533217432698,0.167922504900279,
-0.04));
#50303=CARTESIAN_POINT('Ctrl Pts',(-0.356151197810523,0.166856867698425,
-0.04));
#50304=CARTESIAN_POINT('',(-0.348766791062876,-0.183211156103301,-0.0400000000000003));
#50305=CARTESIAN_POINT('Origin',(0.,0.,-0.04));
#50306=CARTESIAN_POINT('Ctrl Pts',(-0.348771505299647,-0.183214908972786,
-0.0400000000000003));
#50307=CARTESIAN_POINT('Ctrl Pts',(-0.344281860949048,-0.190269236295522,
-0.0400000000000003));
#50308=CARTESIAN_POINT('Ctrl Pts',(-0.339556668524804,-0.197160576599915,
-0.0399999999999999));
#50309=CARTESIAN_POINT('Ctrl Pts',(-0.334595493859032,-0.203875367646479,
-0.0399999999999998));
#50310=CARTESIAN_POINT('Ctrl Pts',(-0.325338386804792,-0.216404565619235,
-0.0399999999999996));
#50311=CARTESIAN_POINT('Ctrl Pts',(-0.315260129136267,-0.228319778085478,
-0.04));
#50312=CARTESIAN_POINT('Ctrl Pts',(-0.304447112191422,-0.239582838373425,
-0.04));
#50313=CARTESIAN_POINT('Ctrl Pts',(-0.297795698249758,-0.246511087594449,
-0.04));
#50314=CARTESIAN_POINT('Ctrl Pts',(-0.29086607385478,-0.253192358646992,
-0.0400000000000009));
#50315=CARTESIAN_POINT('Ctrl Pts',(-0.283677124011411,-0.25961550153745,
-0.0400000000000011));
#50316=CARTESIAN_POINT('Ctrl Pts',(-0.27883471219124,-0.263942072696393,
-0.0400000000000013));
#50317=CARTESIAN_POINT('Ctrl Pts',(-0.273882118054872,-0.26814477485101,
-0.0399999999999996));
#50318=CARTESIAN_POINT('Ctrl Pts',(-0.268826637302453,-0.272220395003461,
-0.0399999999999996));
#50319=CARTESIAN_POINT('Ctrl Pts',(-0.252040976976963,-0.285752634338373,
-0.0399999999999998));
#50320=CARTESIAN_POINT('Ctrl Pts',(-0.234119262469246,-0.29789035047311,
-0.0399999999999999));
#50321=CARTESIAN_POINT('Ctrl Pts',(-0.215283052615073,-0.308512792785733,
-0.04));
#50322=CARTESIAN_POINT('Ctrl Pts',(-0.210201809912688,-0.311378295341735,
-0.04));
#50323=CARTESIAN_POINT('Ctrl Pts',(-0.205051943084034,-0.314134253626617,
-0.0399999999999998));
#50324=CARTESIAN_POINT('Ctrl Pts',(-0.199844116499647,-0.316774415575878,
-0.0399999999999997));
#50325=CARTESIAN_POINT('Ctrl Pts',(-0.181065974193667,-0.326294190474429,
-0.0399999999999996));
#50326=CARTESIAN_POINT('Ctrl Pts',(-0.161610877978346,-0.33427555732133,
-0.0399999999999996));
#50327=CARTESIAN_POINT('Ctrl Pts',(-0.141687478465979,-0.340616307280008,
-0.0399999999999995));
#50328=CARTESIAN_POINT('Ctrl Pts',(-0.122302515671901,-0.346785696292121,
-0.0399999999999994));
#50329=CARTESIAN_POINT('Ctrl Pts',(-0.102472851443113,-0.351402165887278,
-0.0400000000000007));
#50330=CARTESIAN_POINT('Ctrl Pts',(-0.0823890484208069,-0.354323211780531,
-0.0400000000000007));
#50331=CARTESIAN_POINT('Ctrl Pts',(-0.0767749361799088,-0.355139744360905,
-0.0400000000000007));
#50332=CARTESIAN_POINT('Ctrl Pts',(-0.0711410219815515,-0.355823489525933,
-0.0400000000000009));
#50333=CARTESIAN_POINT('Ctrl Pts',(-0.0654916600524661,-0.356370597325589,
-0.0400000000000009));
#50334=CARTESIAN_POINT('Ctrl Pts',(-0.0604220160106905,-0.356861562824268,
-0.0400000000000009));
#50335=CARTESIAN_POINT('Ctrl Pts',(-0.0553499384085825,-0.357241508756984,
-0.0400000000000003));
#50336=CARTESIAN_POINT('Ctrl Pts',(-0.0502793161526174,-0.357508750027682,
-0.0400000000000003));
#50337=CARTESIAN_POINT('Ctrl Pts',(-0.0364167837107168,-0.358239358737591,
-0.0400000000000004));
#50338=CARTESIAN_POINT('Ctrl Pts',(-0.0225628301172705,-0.358128707187053,
-0.0400000000000002));
#50339=CARTESIAN_POINT('Ctrl Pts',(-0.00877966728186113,-0.357135742011749,
-0.0400000000000002));
#50340=CARTESIAN_POINT('Ctrl Pts',(0.0117257534661439,-0.355658492635037,
-0.0400000000000003));
#50341=CARTESIAN_POINT('Ctrl Pts',(0.0320762654196419,-0.35223025391618,
-0.0399999999999998));
#50342=CARTESIAN_POINT('Ctrl Pts',(0.0520546625937477,-0.346973284194516,
-0.0399999999999998));
#50343=CARTESIAN_POINT('Ctrl Pts',(0.057542659920442,-0.345529212604209,
-0.0399999999999998));
#50344=CARTESIAN_POINT('Ctrl Pts',(0.0630024049445004,-0.343946874059417,
-0.0400000000000005));
#50345=CARTESIAN_POINT('Ctrl Pts',(0.0684289356558515,-0.342228230074204,
-0.0400000000000005));
#50346=CARTESIAN_POINT('Ctrl Pts',(0.0736357693981515,-0.34057916661742,
-0.0400000000000005));
#50347=CARTESIAN_POINT('Ctrl Pts',(0.0788044417638721,-0.338806902750585,
-0.0400000000000001));
#50348=CARTESIAN_POINT('Ctrl Pts',(0.0839245765806507,-0.336916643979113,
-0.0400000000000001));
#50349=CARTESIAN_POINT('Ctrl Pts',(0.103108695538129,-0.329834223216773,
-0.0400000000000002));
#50350=CARTESIAN_POINT('Ctrl Pts',(0.121643544170652,-0.321089833264376,
-0.0400000000000006));
#50351=CARTESIAN_POINT('Ctrl Pts',(0.139316889058501,-0.310813500312407,
-0.0400000000000003));
#50352=CARTESIAN_POINT('Ctrl Pts',(0.153758842758092,-0.302416090221918,
-0.0400000000000001));
#50353=CARTESIAN_POINT('Ctrl Pts',(0.167625439375493,-0.292994385994367,
-0.0399999999999986));
#50354=CARTESIAN_POINT('Ctrl Pts',(0.180778458081028,-0.28259993810822,
-0.0399999999999982));
#50355=CARTESIAN_POINT('Ctrl Pts',(0.18501406420843,-0.27925266185604,-0.0399999999999981));
#50356=CARTESIAN_POINT('Ctrl Pts',(0.189176410882292,-0.275803308569567,
-0.0400000000000001));
#50357=CARTESIAN_POINT('Ctrl Pts',(0.193246995837017,-0.27226575337169,
-0.0400000000000001));
#50358=CARTESIAN_POINT('Ctrl Pts',(0.208094771338353,-0.259362245402719,
-0.0399999999999999));
#50359=CARTESIAN_POINT('Ctrl Pts',(0.22176966298894,-0.245254393801563,
-0.0399999999999998));
#50360=CARTESIAN_POINT('Ctrl Pts',(0.234062004541931,-0.23004354120916,
-0.0399999999999999));
#50361=CARTESIAN_POINT('Ctrl Pts',(0.2454650733056,-0.215933097131644,-0.0399999999999999));
#50362=CARTESIAN_POINT('Ctrl Pts',(0.255678773688448,-0.200872367689583,
-0.0400000000000001));
#50363=CARTESIAN_POINT('Ctrl Pts',(0.264490302733435,-0.184924190981102,
-0.0399999999999997));
#50364=CARTESIAN_POINT('Ctrl Pts',(0.265177473281506,-0.18368046616631,
-0.0399999999999997));
#50365=CARTESIAN_POINT('Ctrl Pts',(0.265856090160851,-0.182431338984764,
-0.04));
#50366=CARTESIAN_POINT('Ctrl Pts',(0.266526038810872,-0.181176836987473,
-0.04));
#50367=CARTESIAN_POINT('Ctrl Pts',(0.142815504361805,0.288902937573994,
-2.88100630286919));
#50368=CARTESIAN_POINT('Ctrl Pts',(0.0466461460635961,0.336443040574824,
-2.87438391055481));
#50369=CARTESIAN_POINT('Ctrl Pts',(-0.195237416096998,0.327094963396398,
-2.86113912592605));
#50370=CARTESIAN_POINT('Ctrl Pts',(-0.381101025730574,0.012353614834551,
-2.84127194898291));
#50371=CARTESIAN_POINT('Ctrl Pts',(-0.216533073052069,-0.313416506212782,
-2.82140477203977));
#50372=CARTESIAN_POINT('Ctrl Pts',(0.146152353759915,-0.351899746021385,
-2.80153759509663));
#50373=CARTESIAN_POINT('Ctrl Pts',(0.375042359224723,-0.0675819005554749,
-2.78167041815349));
#50374=CARTESIAN_POINT('Ctrl Pts',(0.259857122798181,0.278675922139343,
-2.76180324121035));
#50375=CARTESIAN_POINT('Ctrl Pts',(-0.0935766607715254,0.369381537016774,
-2.7419360642672));
#50376=CARTESIAN_POINT('Ctrl Pts',(-0.361225822360449,0.121318076485742,
-2.72206888732406));
#50377=CARTESIAN_POINT('Ctrl Pts',(-0.297578297103382,-0.238000159986643,
-2.70220171038092));
#50378=CARTESIAN_POINT('Ctrl Pts',(0.0389678303295289,-0.379052262416539,
-2.68233453343778));
#50379=CARTESIAN_POINT('Ctrl Pts',(0.339781580148665,-0.172475450822871,
-2.66246735649464));
#50380=CARTESIAN_POINT('Ctrl Pts',(0.32898038540163,0.192277148854254,-2.6426001795515));
#50381=CARTESIAN_POINT('Ctrl Pts',(0.0164738552685434,0.380693518847251,
-2.62273300260836));
#50382=CARTESIAN_POINT('Ctrl Pts',(-0.311141479570281,0.219977088554462,
-2.60286582566522));
#50383=CARTESIAN_POINT('Ctrl Pts',(-0.353409779756908,-0.142479382852879,
-2.58299864872207));
#50384=CARTESIAN_POINT('Ctrl Pts',(-0.0715674996361506,-0.374268611298861,
-2.56313147177894));
#50385=CARTESIAN_POINT('Ctrl Pts',(0.275909162196494,-0.262817483673361,
-2.54326429483579));
#50386=CARTESIAN_POINT('Ctrl Pts',(0.370350525192519,0.0896625461742955,
-2.52339711789266));
#50387=CARTESIAN_POINT('Ctrl Pts',(0.125144851946343,0.359913403121745,
-2.5035299409495));
#50388=CARTESIAN_POINT('Ctrl Pts',(-0.234830704909087,0.300089037511211,
-2.48366276400638));
#50389=CARTESIAN_POINT('Ctrl Pts',(-0.379443904784244,-0.034945844948649,
-2.46379558706322));
#50390=CARTESIAN_POINT('Ctrl Pts',(-0.176070541289752,-0.337932026630971,
-2.44392841012009));
#50391=CARTESIAN_POINT('Ctrl Pts',(0.188776450434642,-0.331002026615422,
-2.42406123317694));
#50392=CARTESIAN_POINT('Ctrl Pts',(0.380497273760583,-0.0205113226115502,
-2.40419405623381));
#50393=CARTESIAN_POINT('Ctrl Pts',(0.223265489718655,0.308790237805464,
-2.38432687929066));
#50394=CARTESIAN_POINT('Ctrl Pts',(-0.13872222919299,0.354901441165425,
-2.36445970234752));
#50395=CARTESIAN_POINT('Ctrl Pts',(-0.373488317233333,0.0755338777360533,
-2.34459252540438));
#50396=CARTESIAN_POINT('Ctrl Pts',(-0.265729684906711,-0.27310551876284,
-2.32472534846124));
#50397=CARTESIAN_POINT('Ctrl Pts',(0.0857286345377398,-0.371280878892406,
-2.3048581715181));
#50398=CARTESIAN_POINT('Ctrl Pts',(0.358565548084728,-0.128955951921072,
-2.28499099457496));
#50399=CARTESIAN_POINT('Ctrl Pts',(0.302563356235795,0.231633989897339,
-2.26512381763181));
#50400=CARTESIAN_POINT('Ctrl Pts',(-0.0309185430950134,0.379793277328495,
-2.24525664068868));
#50401=CARTESIAN_POINT('Ctrl Pts',(-0.33604516371248,0.17964558930402,-2.22538946374553));
#50402=CARTESIAN_POINT('Ctrl Pts',(-0.332986038093936,-0.185254387926107,
-2.20552228680239));
#50403=CARTESIAN_POINT('Ctrl Pts',(-0.0245466787495387,-0.380258267988377,
-2.18565510985925));
#50404=CARTESIAN_POINT('Ctrl Pts',(0.306404346658912,-0.226528731422051,
-2.16578793291611));
#50405=CARTESIAN_POINT('Ctrl Pts',(0.356353106829473,0.134949446327866,
-2.14592075597297));
#50406=CARTESIAN_POINT('Ctrl Pts',(0.0794917830842547,0.372665998225311,
-2.12605357902982));
#50407=CARTESIAN_POINT('Ctrl Pts',(-0.270271153702829,0.26861197532375,
-2.10618640208669));
#50408=CARTESIAN_POINT('Ctrl Pts',(-0.372169439589422,-0.0817850722741498,
-2.08631922514355));
#50409=CARTESIAN_POINT('Ctrl Pts',(-0.132752542720296,-0.357177340004209,
-2.0664520482004));
#50410=CARTESIAN_POINT('Ctrl Pts',(0.228411208027658,-0.305003622697395,
-2.04658487125726));
#50411=CARTESIAN_POINT('Ctrl Pts',(0.380099905430515,0.0268877612103093,
-2.02671769431412));
#50412=CARTESIAN_POINT('Ctrl Pts',(0.183200419906357,0.334120481200005,
-2.00685051737098));
#50413=CARTESIAN_POINT('Ctrl Pts',(-0.181711476497752,0.334932573990939,
-1.98698334042784));
#50414=CARTESIAN_POINT('Ctrl Pts',(-0.379976466379767,0.0285792723618732,
-1.9671161634847));
#50415=CARTESIAN_POINT('Ctrl Pts',(-0.229766478820454,-0.303983971652517,
-1.94724898654156));
#50416=CARTESIAN_POINT('Ctrl Pts',(0.131161475792397,-0.357764667175434,
-1.92738180959841));
#50417=CARTESIAN_POINT('Ctrl Pts',(0.371801737976828,-0.0834407421383482,
-1.90751463265528));
#50418=CARTESIAN_POINT('Ctrl Pts',(0.271464035161107,0.267406371325063,
-1.88764745571213));
#50419=CARTESIAN_POINT('Ctrl Pts',(-0.0778323056202418,0.373016114950851,
-1.86778027876899));
#50420=CARTESIAN_POINT('Ctrl Pts',(-0.355748933853518,0.136534193055344,
-1.84791310182585));
#50421=CARTESIAN_POINT('Ctrl Pts',(-0.307409562917938,-0.225162719911157,
-1.82804592488271));
#50422=CARTESIAN_POINT('Ctrl Pts',(0.0228539532777633,-0.380363755674442,
-1.80817874793957));
#50423=CARTESIAN_POINT('Ctrl Pts',(0.332158195524763,-0.186734632451837,
-1.78831157099643));
#50424=CARTESIAN_POINT('Ctrl Pts',(0.336841415329915,0.178148114583703,
-1.76844439405329));
#50425=CARTESIAN_POINT('Ctrl Pts',(0.0326086495564207,0.379651900805587,
-1.74857721711014));
#50426=CARTESIAN_POINT('Ctrl Pts',(-0.301529385158674,0.23297836744432,
-1.72871004016701));
#50427=CARTESIAN_POINT('Ctrl Pts',(-0.359135963354434,-0.127358743856361,
-1.70884286322386));
#50428=CARTESIAN_POINT('Ctrl Pts',(-0.0873803104607973,-0.370895633777163,
-1.68897568628072));
#50429=CARTESIAN_POINT('Ctrl Pts',(0.264511494039161,-0.27428554342575,
-1.66910850933758));
#50430=CARTESIAN_POINT('Ctrl Pts',(0.373820809690602,0.0738707794290245,
-1.64924133239444));
#50431=CARTESIAN_POINT('Ctrl Pts',(0.140300477324218,0.354280490393961,
-1.6293741554513));
#50432=CARTESIAN_POINT('Ctrl Pts',(-0.22188889114426,0.309780906122309,
-1.60950697850816));
#50433=CARTESIAN_POINT('Ctrl Pts',(-0.380584798365858,-0.0188175732762695,
-1.58963980156501));
#50434=CARTESIAN_POINT('Ctrl Pts',(-0.190247829186885,-0.330158527530134,
-1.56977262462188));
#50435=CARTESIAN_POINT('Ctrl Pts',(0.174564703217894,-0.338712347282523,
-1.54990544767873));
#50436=CARTESIAN_POINT('Ctrl Pts',(0.379284607793692,-0.0366343568522026,
-1.53003827073559));
#50437=CARTESIAN_POINT('Ctrl Pts',(0.236164035815733,0.299040863425743,
-1.51017109379245));
#50438=CARTESIAN_POINT('Ctrl Pts',(-0.123541678493353,0.360466841035667,
-1.49030391684931));
#50439=CARTESIAN_POINT('Ctrl Pts',(-0.36994778760266,0.0913100446779361,
-1.47043673990617));
#50440=CARTESIAN_POINT('Ctrl Pts',(-0.277076182574637,-0.261586847645394,
-1.45056956296303));
#50441=CARTESIAN_POINT('Ctrl Pts',(0.0699009395453964,-0.374583433245331,
-1.43070238601989));
#50442=CARTESIAN_POINT('Ctrl Pts',(0.352772174889632,-0.144050971655273,
-1.41083520907674));
#50443=CARTESIAN_POINT('Ctrl Pts',(0.312117385430717,0.218590090175839,
-1.3909680321336));
#50444=CARTESIAN_POINT('Ctrl Pts',(-0.0147790754750554,0.380763008627795,
-1.37110085519046));
#50445=CARTESIAN_POINT('Ctrl Pts',(-0.328121702266199,0.193739614723267,
-1.35123367824732));
#50446=CARTESIAN_POINT('Ctrl Pts',(-0.340545159287118,-0.170961645690779,
-1.33136650130418));
#50447=CARTESIAN_POINT('Ctrl Pts',(-0.040655941181135,-0.378874628680604,
-1.31149932436104));
#50448=CARTESIAN_POINT('Ctrl Pts',(0.296518686521221,-0.239323125407717,
-1.29163214741789));
#50449=CARTESIAN_POINT('Ctrl Pts',(0.361757150437206,0.119710709290111,
-1.27176497047476));
#50450=CARTESIAN_POINT('Ctrl Pts',(0.0952295025228559,0.368958306127452,
-1.25189779353161));
#50451=CARTESIAN_POINT('Ctrl Pts',(-0.258632761294349,0.279835638538854,
-1.23203061658847));
#50452=CARTESIAN_POINT('Ctrl Pts',(-0.375303899786546,-0.0659232327499082,
-1.21216343964533));
#50453=CARTESIAN_POINT('Ctrl Pts',(-0.147785253953922,-0.351224157091969,
-1.19229626270219));
#50454=CARTESIAN_POINT('Ctrl Pts',(0.21526668826523,-0.314418737887087,
-1.17242908575905));
#50455=CARTESIAN_POINT('Ctrl Pts',(0.38089836640381,0.0107389143816884,
-1.15256190881591));
#50456=CARTESIAN_POINT('Ctrl Pts',(0.197209596082445,0.326047948964853,
-1.13269473187277));
#50457=CARTESIAN_POINT('Ctrl Pts',(-0.167339347503859,0.342339645072217,
-1.11282755492962));
#50458=CARTESIAN_POINT('Ctrl Pts',(-0.378422009606898,0.0446729499391543,
-1.09296037798649));
#50459=CARTESIAN_POINT('Ctrl Pts',(-0.242455280684575,-0.293963138300284,
-1.07309320104334));
#50460=CARTESIAN_POINT('Ctrl Pts',(0.115866267398166,-0.363006746342826,
-1.0532260241002));
#50461=CARTESIAN_POINT('Ctrl Pts',(0.367927300711469,-0.0991382428851851,
-1.03335884715706));
#50462=CARTESIAN_POINT('Ctrl Pts',(0.282563600758959,0.255649567449899,
-1.01349167021392));
#50463=CARTESIAN_POINT('Ctrl Pts',(-0.0619381067084859,0.375982128230261,
-0.99362449327078));
#50464=CARTESIAN_POINT('Ctrl Pts',(-0.349636611220657,0.151502903950139,
-0.973757316327636));
#50465=CARTESIAN_POINT('Ctrl Pts',(-0.316684704488649,-0.211919059440451,
-0.953890139384496));
#50466=CARTESIAN_POINT('Ctrl Pts',(0.00669754469093416,-0.380990856460232,
-0.934022962441355));
#50467=CARTESIAN_POINT('Ctrl Pts',(0.323937501014007,-0.200657382739803,
-0.914155785498214));
#50468=CARTESIAN_POINT('Ctrl Pts',(0.34409560267971,0.163698216324051,-0.894288608555072));
#50469=CARTESIAN_POINT('Ctrl Pts',(0.0486849310371447,0.377926801512009,
-0.874421431611931));
#50470=CARTESIAN_POINT('Ctrl Pts',(-0.291374506373835,0.245560149141897,
-0.854554254668789));
#50471=CARTESIAN_POINT('Ctrl Pts',(-0.364215488118362,-0.112008785485316,
-0.834687077725649));
#50472=CARTESIAN_POINT('Ctrl Pts',(-0.103035825860727,-0.366854887387893,
-0.814819900782507));
#50473=CARTESIAN_POINT('Ctrl Pts',(0.25263760185176,-0.285259762219933,
-0.794952723839366));
#50474=CARTESIAN_POINT('Ctrl Pts',(0.376618042246158,0.0579460099220519,
-0.775085546896225));
#50475=CARTESIAN_POINT('Ctrl Pts',(0.15520350324569,0.348009715944001,-0.755218369953084));
#50476=CARTESIAN_POINT('Ctrl Pts',(-0.208547580455982,0.318915030215117,
-0.735351193009942));
#50477=CARTESIAN_POINT('Ctrl Pts',(-0.381040468388129,-0.00265542123362842,
-0.7154840160668));
#50478=CARTESIAN_POINT('Ctrl Pts',(-0.204082586668139,-0.321790595931231,
-0.695616839123661));
#50479=CARTESIAN_POINT('Ctrl Pts',(0.160038661936921,-0.345812834487786,
-0.675749662180518));
#50480=CARTESIAN_POINT('Ctrl Pts',(0.377389060130195,-0.0526914329514625,
-0.655882485237377));
#50481=CARTESIAN_POINT('Ctrl Pts',(0.248637381342986,0.288753082075454,
-0.636015308294237));
#50482=CARTESIAN_POINT('Ctrl Pts',(-0.108138697680715,0.365383239728838,
-0.616148131351095));
#50483=CARTESIAN_POINT('Ctrl Pts',(-0.36574118686201,0.106921812798457,
-0.596280954407954));
#50484=CARTESIAN_POINT('Ctrl Pts',(-0.287923819462959,-0.249597203472902,
-0.576413777464812));
#50485=CARTESIAN_POINT('Ctrl Pts',(0.0539473916324327,-0.377211570275388,
-0.556546600521672));
#50486=CARTESIAN_POINT('Ctrl Pts',(0.346343654442317,-0.158886635343591,
-0.53667942357853));
#50487=CARTESIAN_POINT('Ctrl Pts',(0.321109463897549,0.205152630716595,
-0.516812246635389));
#50488=CARTESIAN_POINT('Ctrl Pts',(0.00138700138049073,0.381047196669113,
-0.496945069692247));
#50489=CARTESIAN_POINT('Ctrl Pts',(-0.319607475922761,0.207484822257589,
-0.477077892749107));
#50490=CARTESIAN_POINT('Ctrl Pts',(-0.347491146111847,-0.156361095963684,
-0.457210715805965));
#50491=CARTESIAN_POINT('Ctrl Pts',(-0.0566920069213143,-0.376808846437738,
-0.437343538862825));
#50492=CARTESIAN_POINT('Ctrl Pts',(0.286099164537831,-0.251686630090085,
-0.417476361919683));
#50493=CARTESIAN_POINT('Ctrl Pts',(0.366509861887374,0.104256437864189,
-0.397609184976542));
#50494=CARTESIAN_POINT('Ctrl Pts',(0.110795781408782,0.364586327678901,
-0.3777420080334));
#50495=CARTESIAN_POINT('Ctrl Pts',(-0.246528743309069,0.290555466529541,
-0.357874831090259));
#50496=CARTESIAN_POINT('Ctrl Pts',(-0.377762590352976,-0.0499426901134978,
-0.338007654147118));
#50497=CARTESIAN_POINT('Ctrl Pts',(-0.162551991338471,-0.344638636705144,
-0.318140477203977));
#50498=CARTESIAN_POINT('Ctrl Pts',(0.201734794471057,-0.323267715522956,
-0.298273300260835));
#50499=CARTESIAN_POINT('Ctrl Pts',(0.381010653528974,-0.00542935060109167,
-0.278406123317695));
#50500=CARTESIAN_POINT('Ctrl Pts',(0.210864447485707,0.317388544423747,
-0.258538946374552));
#50501=CARTESIAN_POINT('Ctrl Pts',(-0.152667350575211,0.34913004670471,
-0.238671769431413));
#50502=CARTESIAN_POINT('Ctrl Pts',(-0.376183510671294,0.0606867807651417,
-0.21880459248827));
#50503=CARTESIAN_POINT('Ctrl Pts',(-0.254712749740312,-0.2834141590357,
-0.19893741554513));
#50504=CARTESIAN_POINT('Ctrl Pts',(0.100372392813672,-0.367593109417031,
-0.179070238601988));
#50505=CARTESIAN_POINT('Ctrl Pts',(0.363371391885224,-0.114661350979993,
-0.159203061658847));
#50506=CARTESIAN_POINT('Ctrl Pts',(0.29319087692976,0.243440329815534,-0.139335884715706));
#50507=CARTESIAN_POINT('Ctrl Pts',(-0.0460022222542214,0.378256179469882,
-0.119468707772565));
#50508=CARTESIAN_POINT('Ctrl Pts',(-0.34276064692937,0.166227606036299,
-0.099601530829423));
#50509=CARTESIAN_POINT('Ctrl Pts',(-0.32565060598116,-0.198348900769526,
-0.0797343538862829));
#50510=CARTESIAN_POINT('Ctrl Pts',(-0.00893422490495668,-0.380826657875824,
-0.0598671769431404));
#50511=CARTESIAN_POINT('Ctrl Pts',(0.206216301921741,-0.269897423691928,
-0.0466223923143805));
#50512=CARTESIAN_POINT('Ctrl Pts',(0.266526038810872,-0.181176836987473,
-0.04));
#50513=CARTESIAN_POINT('Ctrl Pts',(0.153307031988105,0.310126355608481,
-2.86733753524613));
#50514=CARTESIAN_POINT('Ctrl Pts',(0.0500728701596497,0.361158854664061,
-2.86071514293175));
#50515=CARTESIAN_POINT('Ctrl Pts',(-0.209579967725564,0.351124048055182,
-2.84747035830299));
#50516=CARTESIAN_POINT('Ctrl Pts',(-0.409097509429811,0.0132611373889164,
-2.82760318135985));
#50517=CARTESIAN_POINT('Ctrl Pts',(-0.232440048475256,-0.336440742608989,
-2.80773600441671));
#50518=CARTESIAN_POINT('Ctrl Pts',(0.156889013368218,-0.377751042234421,
-2.78786882747356));
#50519=CARTESIAN_POINT('Ctrl Pts',(0.402593760526857,-0.0725466092534843,
-2.76800165053042));
#50520=CARTESIAN_POINT('Ctrl Pts',(0.278946774127782,0.299148042088607,
-2.74813447358728));
#50521=CARTESIAN_POINT('Ctrl Pts',(-0.100450999282939,0.39651708240153,
-2.72826729664414));
#50522=CARTESIAN_POINT('Ctrl Pts',(-0.387762231775959,0.130230357800768,
-2.708400119701));
#50523=CARTESIAN_POINT('Ctrl Pts',(-0.319439025313521,-0.255484152811664,
-2.68853294275786));
#50524=CARTESIAN_POINT('Ctrl Pts',(0.0418304891862556,-0.406898239649373,
-2.66866576581472));
#50525=CARTESIAN_POINT('Ctrl Pts',(0.364742650383773,-0.185145860560615,
-2.64879858887157));
#50526=CARTESIAN_POINT('Ctrl Pts',(0.353147977130382,0.206402233018786,
-2.62893141192844));
#50527=CARTESIAN_POINT('Ctrl Pts',(0.0176840593597166,0.408660066232896,
-2.60906423498529));
#50528=CARTESIAN_POINT('Ctrl Pts',(-0.333998587719615,0.236137068607296,
-2.58919705804216));
#50529=CARTESIAN_POINT('Ctrl Pts',(-0.379372006227298,-0.152946218285481,
-2.56932988109901));
#50530=CARTESIAN_POINT('Ctrl Pts',(-0.0768249988336868,-0.401763171449355,
-2.54946270415587));
#50531=CARTESIAN_POINT('Ctrl Pts',(0.296178030135373,-0.282124609345433,
-2.52959552721273));
#50532=CARTESIAN_POINT('Ctrl Pts',(0.397557254488719,0.0962493455868358,
-2.50972835026959));
#50533=CARTESIAN_POINT('Ctrl Pts',(0.134338256243387,0.386353399456885,
-2.48986117332645));
#50534=CARTESIAN_POINT('Ctrl Pts',(-0.252081862891316,0.322134209997684,
-2.4699939963833));
#50535=CARTESIAN_POINT('Ctrl Pts',(-0.407318652889952,-0.0375130402916304,
-2.45012681944016));
#50536=CARTESIAN_POINT('Ctrl Pts',(-0.189005053942099,-0.362757224770722,
-2.43025964249702));
#50537=CARTESIAN_POINT('Ctrl Pts',(0.202644365923092,-0.355318132363991,
-2.41039246555388));
#50538=CARTESIAN_POINT('Ctrl Pts',(0.408449404568997,-0.0220181275540013,
-2.39052528861074));
#50539=CARTESIAN_POINT('Ctrl Pts',(0.239667042644229,0.331474618784579,
-2.3706581116676));
#50540=CARTESIAN_POINT('Ctrl Pts',(-0.148913056207633,0.380973248223346,
-2.35079093472446));
#50541=CARTESIAN_POINT('Ctrl Pts',(-0.400925555338986,0.0810827554194012,
-2.33092375778132));
#50542=CARTESIAN_POINT('Ctrl Pts',(-0.285250747012572,-0.293168425152445,
-2.31105658083817));
#50543=CARTESIAN_POINT('Ctrl Pts',(0.0920264405192182,-0.398555953930116,
-2.29118940389504));
#50544=CARTESIAN_POINT('Ctrl Pts',(0.384906528151149,-0.138429327645939,
-2.27132222695189));
#50545=CARTESIAN_POINT('Ctrl Pts',(0.32479029738507,0.248650310464616,-2.25145505000875));
#50546=CARTESIAN_POINT('Ctrl Pts',(-0.0331898843649674,0.407693691076853,
-2.23158787306561));
#50547=CARTESIAN_POINT('Ctrl Pts',(-0.360731748929741,0.192842732510204,
-2.21172069612247));
#50548=CARTESIAN_POINT('Ctrl Pts',(-0.357447893502745,-0.198863565287524,
-2.19185351917933));
#50549=CARTESIAN_POINT('Ctrl Pts',(-0.0263499294497031,-0.408192840929575,
-2.17198634223618));
#50550=CARTESIAN_POINT('Ctrl Pts',(0.328913455051278,-0.243170008953405,
-2.15211916529305));
#50551=CARTESIAN_POINT('Ctrl Pts',(0.382531556303331,0.144863116770228,
-2.13225198834991));
#50552=CARTESIAN_POINT('Ctrl Pts',(0.0853314168272379,0.400042827045369,
-2.11238481140676));
#50553=CARTESIAN_POINT('Ctrl Pts',(-0.290125841667811,0.288344776551862,
-2.09251763446363));
#50554=CARTESIAN_POINT('Ctrl Pts',(-0.39950979016666,-0.0877931758691862,
-2.07265045752048));
#50555=CARTESIAN_POINT('Ctrl Pts',(-0.142504823998407,-0.38341633938238,
-2.05278328057734));
#50556=CARTESIAN_POINT('Ctrl Pts',(0.245190776253722,-0.32740983095854,
-2.03291610363419));
#50557=CARTESIAN_POINT('Ctrl Pts',(0.408022844724805,0.0288629927568269,
-2.01304892669106));
#50558=CARTESIAN_POINT('Ctrl Pts',(0.196658708452732,0.358665675187779,
-1.99318174974791));
#50559=CARTESIAN_POINT('Ctrl Pts',(-0.195060384126591,0.359537426024871,
-1.97331457280478));
#50560=CARTESIAN_POINT('Ctrl Pts',(-0.407890337581508,0.0306787658787993,
-1.95344739586163));
#50561=CARTESIAN_POINT('Ctrl Pts',(-0.246645608092269,-0.326315274201189,
-1.93358021891849));
#50562=CARTESIAN_POINT('Ctrl Pts',(0.140796873944239,-0.384046812844128,
-1.91371304197535));
#50563=CARTESIAN_POINT('Ctrl Pts',(0.399115076419467,-0.0895704747273649,
-1.89384586503221));
#50564=CARTESIAN_POINT('Ctrl Pts',(0.29140635470944,0.287050606345219,-1.87397868808907));
#50565=CARTESIAN_POINT('Ctrl Pts',(-0.0835500306549455,0.400418664082683,
-1.85411151114593));
#50566=CARTESIAN_POINT('Ctrl Pts',(-0.381882999508571,0.146564282328745,
-1.83424433420279));
#50567=CARTESIAN_POINT('Ctrl Pts',(-0.329992516613019,-0.241703647360996,
-1.81437715725964));
#50568=CARTESIAN_POINT('Ctrl Pts',(0.0245328528009995,-0.408306077963147,
-1.7945099803165));
#50569=CARTESIAN_POINT('Ctrl Pts',(0.356559235875546,-0.200452551692539,
-1.77464280337336));
#50570=CARTESIAN_POINT('Ctrl Pts',(0.361586494867377,0.191235250144231,
-1.75477562643022));
#50571=CARTESIAN_POINT('Ctrl Pts',(0.0350041496052865,0.407541928736926,
-1.73490844948708));
#50572=CARTESIAN_POINT('Ctrl Pts',(-0.323680368615757,0.250093448816577,
-1.71504127254394));
#50573=CARTESIAN_POINT('Ctrl Pts',(-0.385518847327489,-0.13671478531412,
-1.6951740956008));
#50574=CARTESIAN_POINT('Ctrl Pts',(-0.0937994520329311,-0.398142407897633,
-1.67530691865766));
#50575=CARTESIAN_POINT('Ctrl Pts',(0.28394306527918,-0.294435136911452,
-1.65543974171452));
#50576=CARTESIAN_POINT('Ctrl Pts',(0.401282473392177,0.0792974824093426,
-1.63557256477137));
#50577=CARTESIAN_POINT('Ctrl Pts',(0.150607245769338,0.380306681100895,
-1.61570538782823));
#50578=CARTESIAN_POINT('Ctrl Pts',(-0.238189316240343,0.332538063681678,
-1.59583821088509));
#50579=CARTESIAN_POINT('Ctrl Pts',(-0.408543358916046,-0.0201999518266245,
-1.57597103394195));
#50580=CARTESIAN_POINT('Ctrl Pts',(-0.204223835256235,-0.354412668060041,
-1.55610385699881));
#50581=CARTESIAN_POINT('Ctrl Pts',(0.187388593835173,-0.363594869420182,
-1.53623668005567));
#50582=CARTESIAN_POINT('Ctrl Pts',(0.407147653607099,-0.0393255938345184,
-1.51636950311253));
#50583=CARTESIAN_POINT('Ctrl Pts',(0.253513143093484,0.321009034837128,
-1.49650232616938));
#50584=CARTESIAN_POINT('Ctrl Pts',(-0.132617310293307,0.386947494085143,
-1.47663514922625));
#50585=CARTESIAN_POINT('Ctrl Pts',(-0.397124930947607,0.0980178727991059,
-1.4567679722831));
#50586=CARTESIAN_POINT('Ctrl Pts',(-0.297430782287474,-0.280803568203938,
-1.43690079533996));
#50587=CARTESIAN_POINT('Ctrl Pts',(0.0750360097299817,-0.402101120878822,
-1.41703361839682));
#50588=CARTESIAN_POINT('Ctrl Pts',(0.378687561564093,-0.154633259310036,
-1.39716644145368));
#50589=CARTESIAN_POINT('Ctrl Pts',(0.335046185679176,0.234648178407669,
-1.37729926451054));
#50590=CARTESIAN_POINT('Ctrl Pts',(-0.015864777474503,0.408734660879019,
-1.3574320875674));
#50591=CARTESIAN_POINT('Ctrl Pts',(-0.352226213323998,0.207972134709531,
-1.33756491062425));
#50592=CARTESIAN_POINT('Ctrl Pts',(-0.365562323653335,-0.183520848116438,
-1.31769773368112));
#50593=CARTESIAN_POINT('Ctrl Pts',(-0.0436426122150763,-0.406707556565216,
-1.29783055673797));
#50594=CARTESIAN_POINT('Ctrl Pts',(0.318301573507149,-0.256904306057869,
-1.27796337979483));
#50595=CARTESIAN_POINT('Ctrl Pts',(0.388332592331863,0.128504910026883,
-1.25809620285169));
#50596=CARTESIAN_POINT('Ctrl Pts',(0.102225262269124,0.396062760080031,
-1.23822902590855));
#50597=CARTESIAN_POINT('Ctrl Pts',(-0.277632468450175,0.300392953696429,
-1.21836184896541));
#50598=CARTESIAN_POINT('Ctrl Pts',(-0.402874514408985,-0.0707660922188523,
-1.19849467202227));
#50599=CARTESIAN_POINT('Ctrl Pts',(-0.158641869848295,-0.377025823119903,
-1.17862749507913));
#50600=CARTESIAN_POINT('Ctrl Pts',(0.231080632395799,-0.337516600332132,
-1.15876031813598));
#50601=CARTESIAN_POINT('Ctrl Pts',(0.408879962322234,0.0115278176412847,
-1.13889314119284));
#50602=CARTESIAN_POINT('Ctrl Pts',(0.211697028204861,0.350000117739169,
-1.1190259642497));
#50603=CARTESIAN_POINT('Ctrl Pts',(-0.179632448278519,0.367488636142218,
-1.09915878730656));
#50604=CARTESIAN_POINT('Ctrl Pts',(-0.406221687141436,0.0479547188936482,
-1.07929161036342));
#50605=CARTESIAN_POINT('Ctrl Pts',(-0.260266556055632,-0.315558289333592,
-1.05942443342028));
#50606=CARTESIAN_POINT('Ctrl Pts',(0.12437804733968,-0.389673986183541,
-1.03955725647714));
#50607=CARTESIAN_POINT('Ctrl Pts',(0.394956014835567,-0.106421146927716,
-1.019690079534));
#50608=CARTESIAN_POINT('Ctrl Pts',(0.303321317764523,0.274430122905259,
-0.999822902590855));
#50609=CARTESIAN_POINT('Ctrl Pts',(-0.0664882104283629,0.40360256694208,
-0.979955725647714));
#50610=CARTESIAN_POINT('Ctrl Pts',(-0.375321652786552,0.162632626240169,
-0.960088548704573));
#50611=CARTESIAN_POINT('Ctrl Pts',(-0.339949029610886,-0.227487079709639,
-0.94022137176143));
#50612=CARTESIAN_POINT('Ctrl Pts',(0.00718956042457087,-0.408979246892924,
-0.920354194818291));
#50613=CARTESIAN_POINT('Ctrl Pts',(0.347734631838634,-0.215398096528849,
-0.900487017875149));
#50614=CARTESIAN_POINT('Ctrl Pts',(0.369373590092455,0.175723831936406,
-0.880619840932009));
#50615=CARTESIAN_POINT('Ctrl Pts',(0.0522614285697006,0.405690100017313,
-0.860752663988866));
#50616=CARTESIAN_POINT('Ctrl Pts',(-0.312779491055863,0.263599514686647,
-0.840885487045725));
#50617=CARTESIAN_POINT('Ctrl Pts',(-0.390971524674726,-0.120237186684183,
-0.821018310102585));
#50618=CARTESIAN_POINT('Ctrl Pts',(-0.110605054554397,-0.393804819771442,
-0.801151133159443));
#50619=CARTESIAN_POINT('Ctrl Pts',(0.271196891973055,-0.306215544922771,
-0.781283956216301));
#50620=CARTESIAN_POINT('Ctrl Pts',(0.404285196540403,0.0622028458072574,
-0.761416779273161));
#50621=CARTESIAN_POINT('Ctrl Pts',(0.166605079351009,0.373575242357697,
-0.741549602330019));
#50622=CARTESIAN_POINT('Ctrl Pts',(-0.223867924780845,0.342343199760824,
-0.721682425386878));
#50623=CARTESIAN_POINT('Ctrl Pts',(-0.409032503417495,-0.00285049406802788,
-0.701815248443737));
#50624=CARTESIAN_POINT('Ctrl Pts',(-0.219074923148997,-0.345430010588501,
-0.681948071500596));
#50625=CARTESIAN_POINT('Ctrl Pts',(0.171795438979374,-0.371216973364516,
-0.662080894557454));
#50626=CARTESIAN_POINT('Ctrl Pts',(0.40511285502146,-0.0565622565497122,
-0.642213717614313));
#50627=CARTESIAN_POINT('Ctrl Pts',(0.266902806843863,0.30996549140952,-0.622346540671173));
#50628=CARTESIAN_POINT('Ctrl Pts',(-0.116082794081587,0.392225061777027,
-0.60247936372803));
#50629=CARTESIAN_POINT('Ctrl Pts',(-0.392609304460204,0.114776514273916,
-0.58261218678489));
#50630=CARTESIAN_POINT('Ctrl Pts',(-0.309075309419628,-0.267933139528199,
-0.562745009841748));
#50631=CARTESIAN_POINT('Ctrl Pts',(0.0579104805996126,-0.404922326388242,
-0.542877832898608));
#50632=CARTESIAN_POINT('Ctrl Pts',(0.371786788470466,-0.170558782087086,
-0.523010655955466));
#50633=CARTESIAN_POINT('Ctrl Pts',(0.344698841161608,0.220223574886063,
-0.503143479012324));
#50634=CARTESIAN_POINT('Ctrl Pts',(0.00148889342201763,0.409039725972165,
-0.483276302069184));
#50635=CARTESIAN_POINT('Ctrl Pts',(-0.343086513987988,0.222727094127726,
-0.463409125126042));
#50636=CARTESIAN_POINT('Ctrl Pts',(-0.373018577293906,-0.167847711267199,
-0.443541948182901));
#50637=CARTESIAN_POINT('Ctrl Pts',(-0.0608567211059766,-0.404490017609605,
-0.42367477123976));
#50638=CARTESIAN_POINT('Ctrl Pts',(0.307116611502172,-0.270176059823644,
-0.403807594296618));
#50639=CARTESIAN_POINT('Ctrl Pts',(0.393434447971258,0.111915335285443,
-0.383940417353478));
#50640=CARTESIAN_POINT('Ctrl Pts',(0.118935072774395,0.391369606890128,
-0.364073240410336));
#50641=CARTESIAN_POINT('Ctrl Pts',(-0.264639263820565,0.311900282820246,
-0.344206063467195));
#50642=CARTESIAN_POINT('Ctrl Pts',(-0.405513825560816,-0.0536115852758187,
-0.324338886524054));
#50643=CARTESIAN_POINT('Ctrl Pts',(-0.174493402850188,-0.36995651654067,
-0.304471709580912));
#50644=CARTESIAN_POINT('Ctrl Pts',(0.216554657194204,-0.347015642495281,
-0.284604532637771));
#50645=CARTESIAN_POINT('Ctrl Pts',(0.409000498296016,-0.00582820212690324,
-0.26473735569463));
#50646=CARTESIAN_POINT('Ctrl Pts',(0.226354993740378,0.340704575109441,
-0.244870178751488));
#50647=CARTESIAN_POINT('Ctrl Pts',(-0.163882615565881,0.374777874974771,
-0.225003001808348));
#50648=CARTESIAN_POINT('Ctrl Pts',(-0.40381874336121,0.0651449594467487,
-0.205135824865206));
#50649=CARTESIAN_POINT('Ctrl Pts',(-0.273424484594403,-0.304234359842993,
-0.185268647922065));
#50650=CARTESIAN_POINT('Ctrl Pts',(0.107745960108261,-0.394597273145052,
-0.165401470978924));
#50651=CARTESIAN_POINT('Ctrl Pts',(0.390065419355187,-0.123084615224664,
-0.145534294035782));
#50652=CARTESIAN_POINT('Ctrl Pts',(0.314729296016912,0.261323968969618,
-0.125667117092642));
#50653=CARTESIAN_POINT('Ctrl Pts',(-0.0493816423515566,0.406043674773425,
-0.1057999401495));
#50654=CARTESIAN_POINT('Ctrl Pts',(-0.367940565682151,0.178439035942154,
-0.0859327632063587));
#50655=CARTESIAN_POINT('Ctrl Pts',(-0.349573585103351,-0.212920028612885,
-0.0660655862632184));
#50656=CARTESIAN_POINT('Ctrl Pts',(-0.00959055187609898,-0.408802985934812,
-0.0461984093200761));
#50657=CARTESIAN_POINT('Ctrl Pts',(0.221365385617334,-0.289724656663478,
-0.0329536246913161));
#50658=CARTESIAN_POINT('Ctrl Pts',(0.286105602751133,-0.194486468872287,
-0.0263312323769356));
#50659=CARTESIAN_POINT('Ctrl Pts',(0.163798559614405,0.331349773642968,
-2.85366876762306));
#50660=CARTESIAN_POINT('Ctrl Pts',(0.0534995942557033,0.385874668753298,
-2.84704637530868));
#50661=CARTESIAN_POINT('Ctrl Pts',(-0.223922519354131,0.375153132713966,
-2.83380159067992));
#50662=CARTESIAN_POINT('Ctrl Pts',(-0.437093993129047,0.0141686599432813,
-2.81393441373678));
#50663=CARTESIAN_POINT('Ctrl Pts',(-0.248347023898443,-0.359464979005196,
-2.79406723679364));
#50664=CARTESIAN_POINT('Ctrl Pts',(0.167625672976521,-0.403602338447458,
-2.7742000598505));
#50665=CARTESIAN_POINT('Ctrl Pts',(0.430145161828992,-0.0775113179514932,
-2.75433288290736));
#50666=CARTESIAN_POINT('Ctrl Pts',(0.298036425457382,0.31962016203787,-2.73446570596421));
#50667=CARTESIAN_POINT('Ctrl Pts',(-0.107325337794352,0.423652627786286,
-2.71459852902108));
#50668=CARTESIAN_POINT('Ctrl Pts',(-0.41429864119147,0.139142639115794,
-2.69473135207794));
#50669=CARTESIAN_POINT('Ctrl Pts',(-0.34129975352366,-0.272968145636686,
-2.67486417513479));
#50670=CARTESIAN_POINT('Ctrl Pts',(0.0446931480429821,-0.434744216882207,
-2.65499699819165));
#50671=CARTESIAN_POINT('Ctrl Pts',(0.389703720618882,-0.197816270298359,
-2.63512982124851));
#50672=CARTESIAN_POINT('Ctrl Pts',(0.377315568859134,0.220527317183318,
-2.61526264430537));
#50673=CARTESIAN_POINT('Ctrl Pts',(0.0188942634508897,0.43662661361854,
-2.59539546736223));
#50674=CARTESIAN_POINT('Ctrl Pts',(-0.356855695868948,0.252297048660129,
-2.57552829041909));
#50675=CARTESIAN_POINT('Ctrl Pts',(-0.405334232697688,-0.163413053718083,
-2.55566111347595));
#50676=CARTESIAN_POINT('Ctrl Pts',(-0.0820824980312227,-0.42925773159985,
-2.5357939365328));
#50677=CARTESIAN_POINT('Ctrl Pts',(0.316446898074251,-0.301431735017504,
-2.51592675958967));
#50678=CARTESIAN_POINT('Ctrl Pts',(0.424763983784919,0.102836144999376,
-2.49605958264652));
#50679=CARTESIAN_POINT('Ctrl Pts',(0.14353166054043,0.412793395792026,-2.47619240570339));
#50680=CARTESIAN_POINT('Ctrl Pts',(-0.269333020873544,0.344179382484156,
-2.45632522876024));
#50681=CARTESIAN_POINT('Ctrl Pts',(-0.43519340099566,-0.0400802356346113,
-2.4364580518171));
#50682=CARTESIAN_POINT('Ctrl Pts',(-0.201939566594445,-0.387582422910473,
-2.41659087487396));
#50683=CARTESIAN_POINT('Ctrl Pts',(0.216512281411541,-0.379634238112561,
-2.39672369793082));
#50684=CARTESIAN_POINT('Ctrl Pts',(0.436401535377412,-0.0235249324964524,
-2.37685652098768));
#50685=CARTESIAN_POINT('Ctrl Pts',(0.256068595569802,0.354158999763693,
-2.35698934404454));
#50686=CARTESIAN_POINT('Ctrl Pts',(-0.159103883222276,0.407045055281267,
-2.33712216710139));
#50687=CARTESIAN_POINT('Ctrl Pts',(-0.428362793444638,0.0866316331027495,
-2.31725499015825));
#50688=CARTESIAN_POINT('Ctrl Pts',(-0.304771809118433,-0.31323133154205,
-2.29738781321512));
#50689=CARTESIAN_POINT('Ctrl Pts',(0.0983242465006967,-0.425831028967825,
-2.27752063627196));
#50690=CARTESIAN_POINT('Ctrl Pts',(0.41124750821757,-0.147902703370805,
-2.25765345932883));
#50691=CARTESIAN_POINT('Ctrl Pts',(0.347017238534345,0.265666631031894,
-2.23778628238569));
#50692=CARTESIAN_POINT('Ctrl Pts',(-0.0354612256349216,0.435594104825211,
-2.21791910544254));
#50693=CARTESIAN_POINT('Ctrl Pts',(-0.385418334147002,0.206039875716387,
-2.19805192849941));
#50694=CARTESIAN_POINT('Ctrl Pts',(-0.381909748911555,-0.21247274264894,
-2.17818475155626));
#50695=CARTESIAN_POINT('Ctrl Pts',(-0.0281531801498664,-0.436127413870774,
-2.15831757461312));
#50696=CARTESIAN_POINT('Ctrl Pts',(0.351422563443643,-0.259811286484759,
-2.13845039766998));
#50697=CARTESIAN_POINT('Ctrl Pts',(0.40871000577719,0.15477678721259,-2.11858322072684));
#50698=CARTESIAN_POINT('Ctrl Pts',(0.0911710505702201,0.427419655865427,
-2.0987160437837));
#50699=CARTESIAN_POINT('Ctrl Pts',(-0.309980529632792,0.308077577779974,
-2.07884886684056));
#50700=CARTESIAN_POINT('Ctrl Pts',(-0.4268501407439,-0.0938012794642228,
-2.05898168989742));
#50701=CARTESIAN_POINT('Ctrl Pts',(-0.152257105276517,-0.409655338760549,
-2.03911451295427));
#50702=CARTESIAN_POINT('Ctrl Pts',(0.261970344479786,-0.349816039219687,
-2.01924733601114));
#50703=CARTESIAN_POINT('Ctrl Pts',(0.435945784019096,0.0308382243033446,
-1.99938015906799));
#50704=CARTESIAN_POINT('Ctrl Pts',(0.210116996999107,0.383210869175555,
-1.97951298212485));
#50705=CARTESIAN_POINT('Ctrl Pts',(-0.20840929175543,0.384142278058803,
-1.95964580518171));
#50706=CARTESIAN_POINT('Ctrl Pts',(-0.435804208783249,0.0327782593957259,
-1.93977862823857));
#50707=CARTESIAN_POINT('Ctrl Pts',(-0.263524737364084,-0.348646576749862,
-1.91991145129543));
#50708=CARTESIAN_POINT('Ctrl Pts',(0.150432272096081,-0.410328958512822,
-1.90004427435229));
#50709=CARTESIAN_POINT('Ctrl Pts',(0.426428414862106,-0.0957002073163822,
-1.88017709740915));
#50710=CARTESIAN_POINT('Ctrl Pts',(0.311348674257774,0.306694841365375,
-1.860309920466));
#50711=CARTESIAN_POINT('Ctrl Pts',(-0.0892677556896494,0.427821213214516,
-1.84044274352286));
#50712=CARTESIAN_POINT('Ctrl Pts',(-0.408017065163623,0.156594371602146,
-1.82057556657972));
#50713=CARTESIAN_POINT('Ctrl Pts',(-0.3525754703081,-0.258244574810834,
-1.80070838963658));
#50714=CARTESIAN_POINT('Ctrl Pts',(0.026211752324236,-0.436248400251852,
-1.78084121269344));
#50715=CARTESIAN_POINT('Ctrl Pts',(0.380960276226329,-0.214170470933241,
-1.7609740357503));
#50716=CARTESIAN_POINT('Ctrl Pts',(0.38633157440484,0.204322385704759,-1.74110685880715));
#50717=CARTESIAN_POINT('Ctrl Pts',(0.0373996496541524,0.435431956668264,
-1.72123968186402));
#50718=CARTESIAN_POINT('Ctrl Pts',(-0.34583135207284,0.267208530188836,
-1.70137250492087));
#50719=CARTESIAN_POINT('Ctrl Pts',(-0.411901731300545,-0.14607082677188,
-1.68150532797773));
#50720=CARTESIAN_POINT('Ctrl Pts',(-0.100218593605065,-0.425389182018102,
-1.66163815103459));
#50721=CARTESIAN_POINT('Ctrl Pts',(0.303374636519199,-0.314584730397155,
-1.64177097409145));
#50722=CARTESIAN_POINT('Ctrl Pts',(0.428744137093751,0.0847241853896615,
-1.62190379714831));
#50723=CARTESIAN_POINT('Ctrl Pts',(0.160914014214458,0.406332871807828,
-1.60203662020517));
#50724=CARTESIAN_POINT('Ctrl Pts',(-0.254489741336427,0.355295221241048,
-1.58216944326203));
#50725=CARTESIAN_POINT('Ctrl Pts',(-0.436501919466233,-0.0215823303769795,
-1.56230226631889));
#50726=CARTESIAN_POINT('Ctrl Pts',(-0.218199841325584,-0.378666808589948,
-1.54243508937574));
#50727=CARTESIAN_POINT('Ctrl Pts',(0.200212484452452,-0.38847739155784,
-1.5225679124326));
#50728=CARTESIAN_POINT('Ctrl Pts',(0.435010699420506,-0.0420168308168348,
-1.50270073548946));
#50729=CARTESIAN_POINT('Ctrl Pts',(0.270862250371236,0.342977206248515,
-1.48283355854632));
#50730=CARTESIAN_POINT('Ctrl Pts',(-0.14169294209326,0.413428147134617,
-1.46296638160318));
#50731=CARTESIAN_POINT('Ctrl Pts',(-0.424302074292555,0.104725700920277,
-1.44309920466004));
#50732=CARTESIAN_POINT('Ctrl Pts',(-0.317785382000311,-0.300020288762482,
-1.4232320277169));
#50733=CARTESIAN_POINT('Ctrl Pts',(0.0801710799145669,-0.429618808512312,
-1.40336485077376));
#50734=CARTESIAN_POINT('Ctrl Pts',(0.404602948238555,-0.165215546964798,
-1.38349767383061));
#50735=CARTESIAN_POINT('Ctrl Pts',(0.357974985927635,0.250706266639499,
-1.36363049688747));
#50736=CARTESIAN_POINT('Ctrl Pts',(-0.0169504794739499,0.436706313130243,
-1.34376331994433));
#50737=CARTESIAN_POINT('Ctrl Pts',(-0.376330724381798,0.222204654695795,
-1.32389614300119));
#50738=CARTESIAN_POINT('Ctrl Pts',(-0.390579488019552,-0.196080050542096,
-1.30402896605805));
#50739=CARTESIAN_POINT('Ctrl Pts',(-0.0466292832490179,-0.434540484449828,
-1.28416178911491));
#50740=CARTESIAN_POINT('Ctrl Pts',(0.340084460493077,-0.274485486708021,
-1.26429461217177));
#50741=CARTESIAN_POINT('Ctrl Pts',(0.414908034226521,0.137299110763656,
-1.24442743522863));
#50742=CARTESIAN_POINT('Ctrl Pts',(0.109221022015393,0.42316721403261,-1.22456025828548));
#50743=CARTESIAN_POINT('Ctrl Pts',(-0.296632175606001,0.320950268854004,
-1.20469308134235));
#50744=CARTESIAN_POINT('Ctrl Pts',(-0.430445129031423,-0.0756089516877968,
-1.1848259043992));
#50745=CARTESIAN_POINT('Ctrl Pts',(-0.169498485742669,-0.402827489147836,
-1.16495872745606));
#50746=CARTESIAN_POINT('Ctrl Pts',(0.246894576526369,-0.360614462777177,
-1.14509155051292));
#50747=CARTESIAN_POINT('Ctrl Pts',(0.436861558240658,0.0123167209008815,
-1.12522437356978));
#50748=CARTESIAN_POINT('Ctrl Pts',(0.226184460327279,0.373952286513485,
-1.10535719662664));
#50749=CARTESIAN_POINT('Ctrl Pts',(-0.19192554905318,0.39263762721222,-1.0854900196835));
#50750=CARTESIAN_POINT('Ctrl Pts',(-0.434021364675974,0.051236487848142,
-1.06562284274036));
#50751=CARTESIAN_POINT('Ctrl Pts',(-0.278077831426689,-0.337153440366899,
-1.04575566579721));
#50752=CARTESIAN_POINT('Ctrl Pts',(0.132889827281194,-0.416341226024256,
-1.02588848885407));
#50753=CARTESIAN_POINT('Ctrl Pts',(0.421984728959667,-0.113704050970247,
-1.00602131191093));
#50754=CARTESIAN_POINT('Ctrl Pts',(0.324079034770088,0.293210678360619,
-0.986154134967789));
#50755=CARTESIAN_POINT('Ctrl Pts',(-0.0710383141482399,0.431223005653899,
-0.966286958024651));
#50756=CARTESIAN_POINT('Ctrl Pts',(-0.401006694352448,0.173762348530199,
-0.946419781081507));
#50757=CARTESIAN_POINT('Ctrl Pts',(-0.363213354733123,-0.243055099978827,
-0.926552604138367));
#50758=CARTESIAN_POINT('Ctrl Pts',(0.00768157615820771,-0.436967637325617,
-0.906685427195226));
#50759=CARTESIAN_POINT('Ctrl Pts',(0.371531762663261,-0.230138810317896,
-0.886818250252084));
#50760=CARTESIAN_POINT('Ctrl Pts',(0.394651577505199,0.187749447548761,
-0.866951073308945));
#50761=CARTESIAN_POINT('Ctrl Pts',(0.0558379261022568,0.433453398522617,
-0.847083896365802));
#50762=CARTESIAN_POINT('Ctrl Pts',(-0.334184475737891,0.281638880231398,
-0.82721671942266));
#50763=CARTESIAN_POINT('Ctrl Pts',(-0.41772756123109,-0.128465587883049,
-0.80734954247952));
#50764=CARTESIAN_POINT('Ctrl Pts',(-0.118174283248069,-0.420754752154992,
-0.787482365536378));
#50765=CARTESIAN_POINT('Ctrl Pts',(0.289756182094351,-0.327171327625608,
-0.767615188593237));
#50766=CARTESIAN_POINT('Ctrl Pts',(0.431952350834647,0.0664596816924623,
-0.747748011650097));
#50767=CARTESIAN_POINT('Ctrl Pts',(0.178006655456329,0.399140768771395,
-0.727880834706954));
#50768=CARTESIAN_POINT('Ctrl Pts',(-0.239188269105709,0.365771369306532,
-0.708013657763814));
#50769=CARTESIAN_POINT('Ctrl Pts',(-0.437024538446861,-0.00304556690242747,
-0.688146480820672));
#50770=CARTESIAN_POINT('Ctrl Pts',(-0.234067259629854,-0.369069425245772,
-0.668279303877532));
#50771=CARTESIAN_POINT('Ctrl Pts',(0.183552216021828,-0.396621112241247,
-0.64841212693439));
#50772=CARTESIAN_POINT('Ctrl Pts',(0.432836649912724,-0.0604330801479618,
-0.628544949991249));
#50773=CARTESIAN_POINT('Ctrl Pts',(0.28516823234474,0.331177900743587,-0.608677773048107));
#50774=CARTESIAN_POINT('Ctrl Pts',(-0.124026890482458,0.419066883825217,
-0.588810596104966));
#50775=CARTESIAN_POINT('Ctrl Pts',(-0.419477422058399,0.122631215749375,
-0.568943419161825));
#50776=CARTESIAN_POINT('Ctrl Pts',(-0.330226799376297,-0.286269075583497,
-0.549076242218684));
#50777=CARTESIAN_POINT('Ctrl Pts',(0.0618735695667918,-0.432633082501095,
-0.529209065275543));
#50778=CARTESIAN_POINT('Ctrl Pts',(0.397229922498616,-0.18223092883058,
-0.509341888332401));
#50779=CARTESIAN_POINT('Ctrl Pts',(0.368288218425666,0.235294519055531,
-0.489474711389261));
#50780=CARTESIAN_POINT('Ctrl Pts',(0.0015907854635455,0.437032255275218,
-0.469607534446119));
#50781=CARTESIAN_POINT('Ctrl Pts',(-0.366565552053217,0.237969365997863,
-0.449740357502978));
#50782=CARTESIAN_POINT('Ctrl Pts',(-0.398546008475964,-0.179334326570714,
-0.429873180559836));
#50783=CARTESIAN_POINT('Ctrl Pts',(-0.0650214352906394,-0.432171188781472,
-0.410006003616696));
#50784=CARTESIAN_POINT('Ctrl Pts',(0.328134058466513,-0.288665489557203,
-0.390138826673554));
#50785=CARTESIAN_POINT('Ctrl Pts',(0.420359034055142,0.119574232706697,
-0.370271649730413));
#50786=CARTESIAN_POINT('Ctrl Pts',(0.127074364140008,0.418152886101354,
-0.350404472787272));
#50787=CARTESIAN_POINT('Ctrl Pts',(-0.28274978433206,0.33324509911095,-0.33053729584413));
#50788=CARTESIAN_POINT('Ctrl Pts',(-0.433265060768657,-0.0572804804381396,
-0.31067011890099));
#50789=CARTESIAN_POINT('Ctrl Pts',(-0.186434814361904,-0.395274396376197,
-0.290802941957848));
#50790=CARTESIAN_POINT('Ctrl Pts',(0.231374519917352,-0.370763569467605,
-0.270935765014707));
#50791=CARTESIAN_POINT('Ctrl Pts',(0.436990343063058,-0.00622705365271487,
-0.251068588071566));
#50792=CARTESIAN_POINT('Ctrl Pts',(0.241845539995049,0.364020605795136,
-0.231201411128424));
#50793=CARTESIAN_POINT('Ctrl Pts',(-0.17509788055655,0.400425703244833,
-0.211334234185283));
#50794=CARTESIAN_POINT('Ctrl Pts',(-0.431453976051128,0.0696031381283553,
-0.191467057242142));
#50795=CARTESIAN_POINT('Ctrl Pts',(-0.292136219448492,-0.325054560650286,
-0.171599880299));
#50796=CARTESIAN_POINT('Ctrl Pts',(0.11511952740285,-0.421601436873074,
-0.15173270335586));
#50797=CARTESIAN_POINT('Ctrl Pts',(0.416759446825152,-0.131507879469335,
-0.131865526412718));
#50798=CARTESIAN_POINT('Ctrl Pts',(0.336267715104065,0.279207608123703,
-0.111998349469577));
#50799=CARTESIAN_POINT('Ctrl Pts',(-0.0527610624488913,0.433831170076969,
-0.0921311725264359));
#50800=CARTESIAN_POINT('Ctrl Pts',(-0.393120484434934,0.190650465848009,
-0.0722639955832943));
#50801=CARTESIAN_POINT('Ctrl Pts',(-0.373496564225541,-0.227491156456244,
-0.052396818640154));
#50802=CARTESIAN_POINT('Ctrl Pts',(-0.0102468788472413,-0.436779313993799,
-0.0325296416970117));
#50803=CARTESIAN_POINT('Ctrl Pts',(0.236514469312927,-0.309551889635029,
-0.0192848570682517));
#50804=CARTESIAN_POINT('Ctrl Pts',(0.305685166691393,-0.207796100757101,
-0.0126624647538713));
#50805=CARTESIAN_POINT('Ctrl Pts',(0.174290087240704,0.352573191677455,
-2.84));
#50806=CARTESIAN_POINT('Ctrl Pts',(0.0569263183517569,0.410590482842535,
-2.83337760768562));
#50807=CARTESIAN_POINT('Ctrl Pts',(-0.238265070982699,0.399182217372751,
-2.82013282305686));
#50808=CARTESIAN_POINT('Ctrl Pts',(-0.465090476828282,0.0150761824976466,
-2.80026564611372));
#50809=CARTESIAN_POINT('Ctrl Pts',(-0.264253999321632,-0.382489215401403,
-2.78039846917058));
#50810=CARTESIAN_POINT('Ctrl Pts',(0.178362332584825,-0.429453634660495,
-2.76053129222743));
#50811=CARTESIAN_POINT('Ctrl Pts',(0.457696563131125,-0.0824760266495024,
-2.74066411528429));
#50812=CARTESIAN_POINT('Ctrl Pts',(0.317126076786983,0.340092281987134,
-2.72079693834115));
#50813=CARTESIAN_POINT('Ctrl Pts',(-0.114199676305766,0.450788173171041,
-2.70092976139801));
#50814=CARTESIAN_POINT('Ctrl Pts',(-0.440835050606981,0.14805492043082,
-2.68106258445487));
#50815=CARTESIAN_POINT('Ctrl Pts',(-0.363160481733799,-0.290452138461707,
-2.66119540751173));
#50816=CARTESIAN_POINT('Ctrl Pts',(0.0475558068997083,-0.462590194115042,
-2.64132823056859));
#50817=CARTESIAN_POINT('Ctrl Pts',(0.414664790853991,-0.210486680036103,
-2.62146105362544));
#50818=CARTESIAN_POINT('Ctrl Pts',(0.401483160587886,0.234652401347849,
-2.60159387668231));
#50819=CARTESIAN_POINT('Ctrl Pts',(0.0201044675420631,0.464593161004185,
-2.58172669973916));
#50820=CARTESIAN_POINT('Ctrl Pts',(-0.379712804018282,0.268457028712963,
-2.56185952279602));
#50821=CARTESIAN_POINT('Ctrl Pts',(-0.431296459168077,-0.173879889150686,
-2.54199234585288));
#50822=CARTESIAN_POINT('Ctrl Pts',(-0.0873399972287587,-0.456752291750344,
-2.52212516890974));
#50823=CARTESIAN_POINT('Ctrl Pts',(0.336715766013129,-0.320738860689576,
-2.5022579919666));
#50824=CARTESIAN_POINT('Ctrl Pts',(0.451970713081119,0.109422944411916,
-2.48239081502346));
#50825=CARTESIAN_POINT('Ctrl Pts',(0.152725064837474,0.439233392127166,
-2.46252363808032));
#50826=CARTESIAN_POINT('Ctrl Pts',(-0.286584178855772,0.366224554970629,
-2.44265646113718));
#50827=CARTESIAN_POINT('Ctrl Pts',(-0.463068149101368,-0.0426474309775924,
-2.42278928419403));
#50828=CARTESIAN_POINT('Ctrl Pts',(-0.214874079246792,-0.412407621050223,
-2.40292210725089));
#50829=CARTESIAN_POINT('Ctrl Pts',(0.230380196899991,-0.40395034386113,
-2.38305493030775));
#50830=CARTESIAN_POINT('Ctrl Pts',(0.464353666185826,-0.0250317374389039,
-2.36318775336461));
#50831=CARTESIAN_POINT('Ctrl Pts',(0.272470148495376,0.376843380742809,
-2.34332057642147));
#50832=CARTESIAN_POINT('Ctrl Pts',(-0.169294710236919,0.433116862339188,
-2.32345339947833));
#50833=CARTESIAN_POINT('Ctrl Pts',(-0.45580003155029,0.092180510786098,
-2.30358622253519));
#50834=CARTESIAN_POINT('Ctrl Pts',(-0.324292871224294,-0.333294237931656,
-2.28371904559205));
#50835=CARTESIAN_POINT('Ctrl Pts',(0.104622052482175,-0.453106104005534,
-2.2638518686489));
#50836=CARTESIAN_POINT('Ctrl Pts',(0.437588488283992,-0.157376079095672,
-2.24398469170577));
#50837=CARTESIAN_POINT('Ctrl Pts',(0.369244179683619,0.282682951599172,
-2.22411751476262));
#50838=CARTESIAN_POINT('Ctrl Pts',(-0.0377325669048753,0.463494518573569,
-2.20425033781949));
#50839=CARTESIAN_POINT('Ctrl Pts',(-0.410104919364264,0.21923701892257,
-2.18438316087634));
#50840=CARTESIAN_POINT('Ctrl Pts',(-0.406371604320363,-0.226081920010357,
-2.1645159839332));
#50841=CARTESIAN_POINT('Ctrl Pts',(-0.0299564308500308,-0.464061986811973,
-2.14464880699006));
#50842=CARTESIAN_POINT('Ctrl Pts',(0.373931671836009,-0.276452564016112,
-2.12478163004692));
#50843=CARTESIAN_POINT('Ctrl Pts',(0.434888455251049,0.164690457654952,
-2.10491445310378));
#50844=CARTESIAN_POINT('Ctrl Pts',(0.0970106843132033,0.454796484685485,
-2.08504727616063));
#50845=CARTESIAN_POINT('Ctrl Pts',(-0.329835217597774,0.327810379008085,
-2.0651800992175));
#50846=CARTESIAN_POINT('Ctrl Pts',(-0.454190491321138,-0.0998093830592591,
-2.04531292227435));
#50847=CARTESIAN_POINT('Ctrl Pts',(-0.162009386554628,-0.43589433813872,
-2.02544574533121));
#50848=CARTESIAN_POINT('Ctrl Pts',(0.27874991270585,-0.372222247480832,
-2.00557856838807));
#50849=CARTESIAN_POINT('Ctrl Pts',(0.463868723313386,0.0328134558498621,
-1.98571139144493));
#50850=CARTESIAN_POINT('Ctrl Pts',(0.223575285545482,0.40775606316333,-1.96584421450179));
#50851=CARTESIAN_POINT('Ctrl Pts',(-0.22175819938427,0.408747130092735,
-1.94597703755865));
#50852=CARTESIAN_POINT('Ctrl Pts',(-0.463718079984989,0.0348777529126524,
-1.9261098606155));
#50853=CARTESIAN_POINT('Ctrl Pts',(-0.2804038666359,-0.370977879298534,
-1.90624268367236));
#50854=CARTESIAN_POINT('Ctrl Pts',(0.160067670247924,-0.436611104181516,
-1.88637550672922));
#50855=CARTESIAN_POINT('Ctrl Pts',(0.453741753304744,-0.101829939905399,
-1.86650832978608));
#50856=CARTESIAN_POINT('Ctrl Pts',(0.331290993806108,0.326339076385531,
-1.84664115284294));
#50857=CARTESIAN_POINT('Ctrl Pts',(-0.0949854807243538,0.455223762346349,
-1.8267739758998));
#50858=CARTESIAN_POINT('Ctrl Pts',(-0.434151130818675,0.166624460875547,
-1.80690679895666));
#50859=CARTESIAN_POINT('Ctrl Pts',(-0.375158424003181,-0.274785502260672,
-1.78703962201352));
#50860=CARTESIAN_POINT('Ctrl Pts',(0.0278906518474728,-0.464190722540557,
-1.76717244507037));
#50861=CARTESIAN_POINT('Ctrl Pts',(0.405361316577113,-0.227888390173943,
-1.74730526812723));
#50862=CARTESIAN_POINT('Ctrl Pts',(0.411076653942302,0.217409521265286,
-1.72743809118409));
#50863=CARTESIAN_POINT('Ctrl Pts',(0.0397951497030185,0.463321984599604,
-1.70757091424095));
#50864=CARTESIAN_POINT('Ctrl Pts',(-0.367982335529924,0.284323611561093,
-1.68770373729781));
#50865=CARTESIAN_POINT('Ctrl Pts',(-0.438284615273599,-0.155426868229639,
-1.66783656035467));
#50866=CARTESIAN_POINT('Ctrl Pts',(-0.106637735177198,-0.452635956138572,
-1.64796938341153));
#50867=CARTESIAN_POINT('Ctrl Pts',(0.322806207759218,-0.334734323882857,
-1.62810220646839));
#50868=CARTESIAN_POINT('Ctrl Pts',(0.456205800795326,0.0901508883699798,
-1.60823502952524));
#50869=CARTESIAN_POINT('Ctrl Pts',(0.171220782659577,0.432359062514762,
-1.5883678525821));
#50870=CARTESIAN_POINT('Ctrl Pts',(-0.27079016643251,0.378052378800417,
-1.56850067563896));
#50871=CARTESIAN_POINT('Ctrl Pts',(-0.464460480016421,-0.0229647089273341,
-1.54863349869582));
#50872=CARTESIAN_POINT('Ctrl Pts',(-0.232175847394933,-0.402920949119856,
-1.52876632175268));
#50873=CARTESIAN_POINT('Ctrl Pts',(0.213036375069731,-0.413359913695497,
-1.50889914480954));
#50874=CARTESIAN_POINT('Ctrl Pts',(0.462873745233912,-0.0447080677991511,
-1.4890319678664));
#50875=CARTESIAN_POINT('Ctrl Pts',(0.288211357648988,0.364945377659901,
-1.46916479092326));
#50876=CARTESIAN_POINT('Ctrl Pts',(-0.150768573893214,0.439908800184091,
-1.44929761398012));
#50877=CARTESIAN_POINT('Ctrl Pts',(-0.451479217637502,0.111433529041447,
-1.42943043703697));
#50878=CARTESIAN_POINT('Ctrl Pts',(-0.338139981713148,-0.319237009321025,
-1.40956326009383));
#50879=CARTESIAN_POINT('Ctrl Pts',(0.0853061500991524,-0.457136496145803,
-1.38969608315069));
#50880=CARTESIAN_POINT('Ctrl Pts',(0.430518334913016,-0.175797834619561,
-1.36982890620755));
#50881=CARTESIAN_POINT('Ctrl Pts',(0.380903786176095,0.266764354871328,
-1.34996172926441));
#50882=CARTESIAN_POINT('Ctrl Pts',(-0.0180361814733977,0.464677965381466,
-1.33009455232127));
#50883=CARTESIAN_POINT('Ctrl Pts',(-0.400435235439597,0.23643717468206,
-1.31022737537813));
#50884=CARTESIAN_POINT('Ctrl Pts',(-0.415596652385769,-0.208639252967755,
-1.29036019843499));
#50885=CARTESIAN_POINT('Ctrl Pts',(-0.0496159542829584,-0.46237341233444,
-1.27049302149184));
#50886=CARTESIAN_POINT('Ctrl Pts',(0.361867347479004,-0.292066667358173,
-1.2506258445487));
#50887=CARTESIAN_POINT('Ctrl Pts',(0.441483476121179,0.146093311500428,
-1.23075866760556));
#50888=CARTESIAN_POINT('Ctrl Pts',(0.116216781761661,0.450271667985189,
-1.21089149066242));
#50889=CARTESIAN_POINT('Ctrl Pts',(-0.315631882761826,0.341507584011579,
-1.19102431371928));
#50890=CARTESIAN_POINT('Ctrl Pts',(-0.458015743653862,-0.0804518111567413,
-1.17115713677614));
#50891=CARTESIAN_POINT('Ctrl Pts',(-0.180355101637042,-0.42862915517577,
-1.151289959833));
#50892=CARTESIAN_POINT('Ctrl Pts',(0.262708520656938,-0.383712325222222,
-1.13142278288986));
#50893=CARTESIAN_POINT('Ctrl Pts',(0.464843154159083,0.0131056241604778,
-1.11155560594671));
#50894=CARTESIAN_POINT('Ctrl Pts',(0.240671892449695,0.397904455287802,
-1.09168842900357));
#50895=CARTESIAN_POINT('Ctrl Pts',(-0.204218649827841,0.417786618282221,
-1.07182125206043));
#50896=CARTESIAN_POINT('Ctrl Pts',(-0.461821042210512,0.054518256802636,
-1.05195407511729));
#50897=CARTESIAN_POINT('Ctrl Pts',(-0.295889106797746,-0.358748591400207,
-1.03208689817415));
#50898=CARTESIAN_POINT('Ctrl Pts',(0.141401607222709,-0.443008465864971,
-1.01221972123101));
#50899=CARTESIAN_POINT('Ctrl Pts',(0.449013443083765,-0.120986955012779,
-0.992352544287866));
#50900=CARTESIAN_POINT('Ctrl Pts',(0.344836751775652,0.31199123381598,-0.972485367344727));
#50901=CARTESIAN_POINT('Ctrl Pts',(-0.0755884178681167,0.458843444365718,
-0.952618190401585));
#50902=CARTESIAN_POINT('Ctrl Pts',(-0.426691735918344,0.184892070820229,
-0.932751013458443));
#50903=CARTESIAN_POINT('Ctrl Pts',(-0.386477679855359,-0.258623120248015,
-0.912883836515303));
#50904=CARTESIAN_POINT('Ctrl Pts',(0.00817359189184459,-0.46495602775831,
-0.893016659572161));
#50905=CARTESIAN_POINT('Ctrl Pts',(0.395328893487888,-0.244879524106942,
-0.87314948262902));
#50906=CARTESIAN_POINT('Ctrl Pts',(0.419929564917943,0.199775063161117,
-0.85328230568588));
#50907=CARTESIAN_POINT('Ctrl Pts',(0.0594144236348126,0.461216697027921,
-0.833415128742737));
#50908=CARTESIAN_POINT('Ctrl Pts',(-0.355589460419919,0.299678245776149,
-0.813547951799597));
#50909=CARTESIAN_POINT('Ctrl Pts',(-0.444483597787454,-0.136693989081916,
-0.793680774856456));
#50910=CARTESIAN_POINT('Ctrl Pts',(-0.125743511941739,-0.447704684538541,
-0.773813597913313));
#50911=CARTESIAN_POINT('Ctrl Pts',(0.308315472215645,-0.348127110328446,
-0.753946420970174));
#50912=CARTESIAN_POINT('Ctrl Pts',(0.459619505128892,0.0707165175776674,
-0.734079244027031));
#50913=CARTESIAN_POINT('Ctrl Pts',(0.189408231561648,0.424706295185092,
-0.714212067083891));
#50914=CARTESIAN_POINT('Ctrl Pts',(-0.254508613430572,0.389199538852239,
-0.694344890140749));
#50915=CARTESIAN_POINT('Ctrl Pts',(-0.465016573476227,-0.00324063973682662,
-0.674477713197608));
#50916=CARTESIAN_POINT('Ctrl Pts',(-0.249059596110711,-0.392708839903043,
-0.654610536254467));
#50917=CARTESIAN_POINT('Ctrl Pts',(0.195308993064281,-0.422025251117977,
-0.634743359311326));
#50918=CARTESIAN_POINT('Ctrl Pts',(0.460560444803989,-0.0643039037462118,
-0.614876182368184));
#50919=CARTESIAN_POINT('Ctrl Pts',(0.303433657845617,0.352390310077654,
-0.595009005425044));
#50920=CARTESIAN_POINT('Ctrl Pts',(-0.13197098688333,0.445908705873406,
-0.575141828481902));
#50921=CARTESIAN_POINT('Ctrl Pts',(-0.446345539656594,0.130485917224834,
-0.555274651538761));
#50922=CARTESIAN_POINT('Ctrl Pts',(-0.351378289332966,-0.304605011638794,
-0.535407474595619));
#50923=CARTESIAN_POINT('Ctrl Pts',(0.0658366585339714,-0.460343838613949,
-0.515540297652478));
#50924=CARTESIAN_POINT('Ctrl Pts',(0.422673056526765,-0.193903075574074,
-0.495673120709337));
#50925=CARTESIAN_POINT('Ctrl Pts',(0.391877595689725,0.250365463225,-0.475805943766196));
#50926=CARTESIAN_POINT('Ctrl Pts',(0.00169267750507216,0.46502478457827,
-0.455938766823055));
#50927=CARTESIAN_POINT('Ctrl Pts',(-0.390044590118444,0.253211637868,-0.436071589879914));
#50928=CARTESIAN_POINT('Ctrl Pts',(-0.424073439658023,-0.190820941874228,
-0.416204412936772));
#50929=CARTESIAN_POINT('Ctrl Pts',(-0.0691861494753018,-0.459852359953339,
-0.396337235993632));
#50930=CARTESIAN_POINT('Ctrl Pts',(0.349151505430854,-0.307154919290763,
-0.376470059050489));
#50931=CARTESIAN_POINT('Ctrl Pts',(0.447283620139026,0.127233130127951,
-0.356602882107349));
#50932=CARTESIAN_POINT('Ctrl Pts',(0.135213655505621,0.44493616531258,-0.336735705164207));
#50933=CARTESIAN_POINT('Ctrl Pts',(-0.300860304843555,0.354589915401655,
-0.316868528221066));
#50934=CARTESIAN_POINT('Ctrl Pts',(-0.461016295976497,-0.0609493756004606,
-0.297001351277925));
#50935=CARTESIAN_POINT('Ctrl Pts',(-0.19837622587362,-0.420592276211723,
-0.277134174334784));
#50936=CARTESIAN_POINT('Ctrl Pts',(0.246194382640499,-0.39451149643993,
-0.257266997391642));
#50937=CARTESIAN_POINT('Ctrl Pts',(0.4649801878301,-0.00662590517852661,
-0.237399820448502));
#50938=CARTESIAN_POINT('Ctrl Pts',(0.25733608624972,0.387336636480831,-0.217532643505359));
#50939=CARTESIAN_POINT('Ctrl Pts',(-0.18631314554722,0.426073531514894,
-0.197665466562219));
#50940=CARTESIAN_POINT('Ctrl Pts',(-0.459089208741044,0.0740613168099621,
-0.177798289619077));
#50941=CARTESIAN_POINT('Ctrl Pts',(-0.310847954302583,-0.345874761457578,
-0.157931112675936));
#50942=CARTESIAN_POINT('Ctrl Pts',(0.122493094697439,-0.448605600601096,
-0.138063935732795));
#50943=CARTESIAN_POINT('Ctrl Pts',(0.443453474295116,-0.139931143714006,
-0.118196758789654));
#50944=CARTESIAN_POINT('Ctrl Pts',(0.357806134191217,0.297091247277788,
-0.0983295818465128));
#50945=CARTESIAN_POINT('Ctrl Pts',(-0.0561404825462262,0.461618665380512,
-0.0784624049033717));
#50946=CARTESIAN_POINT('Ctrl Pts',(-0.418300403187716,0.202861895753863,
-0.0585952279602298));
#50947=CARTESIAN_POINT('Ctrl Pts',(-0.397419543347731,-0.242062284299603,
-0.0387280510170898));
#50948=CARTESIAN_POINT('Ctrl Pts',(-0.010903205818384,-0.464755642052786,
-0.0188608740739473));
#50949=CARTESIAN_POINT('Ctrl Pts',(0.25166355300852,-0.329379122606579,
-0.00561608944518735));
#50950=CARTESIAN_POINT('Ctrl Pts',(0.325264730631653,-0.221105732641915,
0.00100630286919312));
#50951=CARTESIAN_POINT('Ctrl Pts',(-0.39272888104496,9.19390291685468E-5,
-0.0496163522034977));
#50952=CARTESIAN_POINT('Ctrl Pts',(-0.392616526570956,-0.0635210754266735,
-0.0464109014689986));
#50953=CARTESIAN_POINT('Ctrl Pts',(-0.377854412170386,-0.1271963235368,
-0.0432054507344995));
#50954=CARTESIAN_POINT('Ctrl Pts',(-0.348771505299647,-0.183214908972786,
-0.0400000000000003));
#50955=CARTESIAN_POINT('',(-0.322117167679667,-0.010084934854993,-2.84));
#50956=CARTESIAN_POINT('Ctrl Pts',(-0.322665937590337,-0.00999768482676959,
-2.84));
#50957=CARTESIAN_POINT('Ctrl Pts',(-0.323650211264442,-0.00315523629261327,
-2.84));
#50958=CARTESIAN_POINT('Ctrl Pts',(-0.324397225861028,0.00370989634134569,
-2.84));
#50959=CARTESIAN_POINT('Ctrl Pts',(-0.324901721971083,0.0105873702227374,
-2.84));
#50960=CARTESIAN_POINT('Ctrl Pts',(-0.325997667963835,0.0255277033399459,
-2.84));
#50961=CARTESIAN_POINT('Ctrl Pts',(-0.325950748451652,0.0405258873091143,
-2.84));
#50962=CARTESIAN_POINT('Ctrl Pts',(-0.324836924795275,0.0554860263150083,
-2.84));
#50963=CARTESIAN_POINT('Ctrl Pts',(-0.324393308343733,0.0614443876250565,
-2.84));
#50964=CARTESIAN_POINT('Ctrl Pts',(-0.323780197469711,0.0673967849520013,
-2.84));
#50965=CARTESIAN_POINT('Ctrl Pts',(-0.323001415813532,0.0733373463202781,
-2.84));
#50966=CARTESIAN_POINT('Ctrl Pts',(-0.322198157543006,0.0794646157709396,
-2.84));
#50967=CARTESIAN_POINT('Ctrl Pts',(-0.321219769535019,0.0855702854614099,
-2.84));
#50968=CARTESIAN_POINT('Ctrl Pts',(-0.320072263419342,0.09164450471336,
-2.84));
#50969=CARTESIAN_POINT('Ctrl Pts',(-0.317737578918981,0.104002944764868,
-2.84));
#50970=CARTESIAN_POINT('Ctrl Pts',(-0.314702870444172,0.116235555905157,
-2.84));
#50971=CARTESIAN_POINT('Ctrl Pts',(-0.311007712210463,0.128288621791672,
-2.84));
#50972=CARTESIAN_POINT('Ctrl Pts',(-0.30880376108375,0.135477588125667,
-2.84));
#50973=CARTESIAN_POINT('Ctrl Pts',(-0.306364669022593,0.142602716913589,
-2.84));
#50974=CARTESIAN_POINT('Ctrl Pts',(-0.303697238249508,0.149652643556526,
-2.84));
#50975=CARTESIAN_POINT('Ctrl Pts',(-0.301224487679456,0.156188037202371,
-2.84));
#50976=CARTESIAN_POINT('Ctrl Pts',(-0.298553872096886,0.162661690838749,
-2.84));
#50977=CARTESIAN_POINT('Ctrl Pts',(-0.295701310709281,0.169041266471786,
-2.84));
#50978=CARTESIAN_POINT('Ctrl Pts',(-0.287500937396955,0.187380889938761,
-2.84));
#50979=CARTESIAN_POINT('Ctrl Pts',(-0.277787872339422,0.204982261003147,
-2.84));
#50980=CARTESIAN_POINT('Ctrl Pts',(-0.26670532546941,0.221641187990873,
-2.84));
#50981=CARTESIAN_POINT('Ctrl Pts',(-0.259647208511552,0.232250721742538,
-2.84));
#50982=CARTESIAN_POINT('Ctrl Pts',(-0.25203249560377,0.242478100323189,
-2.84));
#50983=CARTESIAN_POINT('Ctrl Pts',(-0.24388759544458,0.252267871100332,
-2.84));
#50984=CARTESIAN_POINT('Ctrl Pts',(-0.239499894383172,0.257541672717328,
-2.84));
#50985=CARTESIAN_POINT('Ctrl Pts',(-0.234958197800991,0.262688420481687,
-2.84));
#50986=CARTESIAN_POINT('Ctrl Pts',(-0.230265756133984,0.267698872564867,
-2.84));
#50987=CARTESIAN_POINT('Ctrl Pts',(-0.226847227029321,0.271349078041964,
-2.84));
#50988=CARTESIAN_POINT('Ctrl Pts',(-0.223349311713903,0.274925985807238,
-2.84));
#50989=CARTESIAN_POINT('Ctrl Pts',(-0.219782826738047,0.278417295395633,
-2.84));
#50990=CARTESIAN_POINT('Ctrl Pts',(-0.208710072844623,0.289256654624611,
-2.84));
#50991=CARTESIAN_POINT('Ctrl Pts',(-0.196955369123494,0.299295600355571,
-2.84));
#50992=CARTESIAN_POINT('Ctrl Pts',(-0.184574140330731,0.308442555718213,
-2.84));
#50993=CARTESIAN_POINT('Ctrl Pts',(-0.172041900670708,0.317701074293621,
-2.84));
#50994=CARTESIAN_POINT('Ctrl Pts',(-0.158867686557205,0.326046279965927,
-2.84));
#50995=CARTESIAN_POINT('Ctrl Pts',(-0.145156625066643,0.333486543488778,
-2.84));
#50996=CARTESIAN_POINT('Ctrl Pts',(-0.138539413076319,0.337077352342525,
-2.84));
#50997=CARTESIAN_POINT('Ctrl Pts',(-0.131796942169486,0.340457166247357,
-2.84));
#50998=CARTESIAN_POINT('Ctrl Pts',(-0.12494001352005,0.343625665611372,
-2.84));
#50999=CARTESIAN_POINT('Ctrl Pts',(-0.117798371987087,0.346925727171306,
-2.84));
#51000=CARTESIAN_POINT('Ctrl Pts',(-0.110525837567219,0.349998768671215,
-2.84));
#51001=CARTESIAN_POINT('Ctrl Pts',(-0.103170100809649,0.352830723345205,
-2.84));
#51002=CARTESIAN_POINT('Ctrl Pts',(-0.0839056785772351,0.360247515487291,
-2.84));
#51003=CARTESIAN_POINT('Ctrl Pts',(-0.0640406356108989,0.366032022011569,
-2.84));
#51004=CARTESIAN_POINT('Ctrl Pts',(-0.0438096601120564,0.37020654613364,
-2.84));
#51005=CARTESIAN_POINT('Ctrl Pts',(-0.0257589803203683,0.373931181073486,
-2.84));
#51006=CARTESIAN_POINT('Ctrl Pts',(-0.00741575563267887,0.376373790742814,
-2.84));
#51007=CARTESIAN_POINT('Ctrl Pts',(0.0110694999116937,0.377521301223216,
-2.84));
#51008=CARTESIAN_POINT('Ctrl Pts',(0.0163026119130628,0.377846157477016,
-2.84));
#51009=CARTESIAN_POINT('Ctrl Pts',(0.0215471587080905,0.37806704191005,
-2.84));
#51010=CARTESIAN_POINT('Ctrl Pts',(0.0267998089378223,0.378183226427262,
-2.84));
#51011=CARTESIAN_POINT('Ctrl Pts',(0.0319645250457776,0.378297465910437,
-2.84));
#51012=CARTESIAN_POINT('Ctrl Pts',(0.03712808659929,0.37831025253997,-2.84));
#51013=CARTESIAN_POINT('Ctrl Pts',(0.0422850648456711,0.378221894196039,
-2.84));
#51014=CARTESIAN_POINT('Ctrl Pts',(0.0648738954569795,0.377834862960147,
-2.84));
#51015=CARTESIAN_POINT('Ctrl Pts',(0.0873477481761387,0.375512022714285,
-2.84));
#51016=CARTESIAN_POINT('Ctrl Pts',(0.10943707149879,0.371248712598134,-2.84));
#51017=CARTESIAN_POINT('Ctrl Pts',(0.130322404520726,0.367217776464374,
-2.84));
#51018=CARTESIAN_POINT('Ctrl Pts',(0.150865606811995,0.361452006559849,
-2.84));
#51019=CARTESIAN_POINT('Ctrl Pts',(0.170841168278706,0.353897569143461,
-2.84));
#51020=CARTESIAN_POINT('Ctrl Pts',(0.171992712390165,0.353462073603737,
-2.84));
#51021=CARTESIAN_POINT('Ctrl Pts',(0.173142366923995,0.353020619647747,
-2.84));
#51022=CARTESIAN_POINT('Ctrl Pts',(0.174290087240704,0.352573191677455,
-2.84));
#51023=CARTESIAN_POINT('Ctrl Pts',(-0.322665937590337,-0.00999768482676161,
-2.84));
#51024=CARTESIAN_POINT('Ctrl Pts',(-0.319085648514224,-0.109944606251347,
-2.83380159067993));
#51025=CARTESIAN_POINT('Ctrl Pts',(-0.208793047698186,-0.314237772328811,
-2.82098078904546));
#51026=CARTESIAN_POINT('Ctrl Pts',(0.146152353759915,-0.351899746021385,
-2.80153759509663));
#51027=CARTESIAN_POINT('Ctrl Pts',(0.375042359224723,-0.0675819005554749,
-2.78167041815349));
#51028=CARTESIAN_POINT('Ctrl Pts',(0.259857122798181,0.278675922139343,
-2.76180324121035));
#51029=CARTESIAN_POINT('Ctrl Pts',(-0.0935766607715254,0.369381537016774,
-2.7419360642672));
#51030=CARTESIAN_POINT('Ctrl Pts',(-0.3009571590477,0.17717647370315,-2.72654253555465));
#51031=CARTESIAN_POINT('Ctrl Pts',(-0.322260534817986,0.0351318319167836,
-2.71777139915648));
#51032=CARTESIAN_POINT('Ctrl Pts',(-0.321998819203686,0.000257793408019166,
-2.71562265507269));
#51033=CARTESIAN_POINT('Origin',(-5.160062080289E-17,2.1385152528819E-17,
-2.84));
#51034=CARTESIAN_POINT('',(-0.0953060101009199,-0.307860260611277,-2.84));
#51035=CARTESIAN_POINT('Ctrl Pts',(0.386886490162194,0.0743511351644874,
-2.84));
#51036=CARTESIAN_POINT('Ctrl Pts',(0.387777631536103,0.0660369131998544,
-2.84));
#51037=CARTESIAN_POINT('Ctrl Pts',(0.388383000500425,0.0577031558050302,
-2.84));
#51038=CARTESIAN_POINT('Ctrl Pts',(0.388693798011576,0.0493601925761383,
-2.84));
#51039=CARTESIAN_POINT('Ctrl Pts',(0.389273718297948,0.0337929713105256,
-2.84));
#51040=CARTESIAN_POINT('Ctrl Pts',(0.388828835948466,0.0181934386380921,
-2.84));
#51041=CARTESIAN_POINT('Ctrl Pts',(0.387402867595623,0.00264531365779935,
-2.84));
#51042=CARTESIAN_POINT('Ctrl Pts',(0.386525710712122,-0.00691881504449793,
-2.84));
#51043=CARTESIAN_POINT('Ctrl Pts',(0.385277044495428,-0.0164634425160969,
-2.84));
#51044=CARTESIAN_POINT('Ctrl Pts',(0.38366467452966,-0.0259680740313437,
-2.84));
#51045=CARTESIAN_POINT('Ctrl Pts',(0.382578597842544,-0.0323703011426751,
-2.84));
#51046=CARTESIAN_POINT('Ctrl Pts',(0.381329136230223,-0.0387444395247865,
-2.84));
#51047=CARTESIAN_POINT('Ctrl Pts',(0.379919987860161,-0.0450834271490292,
-2.84));
#51048=CARTESIAN_POINT('Ctrl Pts',(0.375241205020874,-0.0661307115549059,
-2.84));
#51049=CARTESIAN_POINT('Ctrl Pts',(0.368804611897396,-0.086796661047342,
-2.84));
#51050=CARTESIAN_POINT('Ctrl Pts',(0.36070805921707,-0.106848695813115,
-2.84));
#51051=CARTESIAN_POINT('Ctrl Pts',(0.358523938385156,-0.112257919785758,
-2.84));
#51052=CARTESIAN_POINT('Ctrl Pts',(0.356217849874627,-0.117624328792278,
-2.84));
#51053=CARTESIAN_POINT('Ctrl Pts',(0.353794229194997,-0.122936384035782,
-2.84));
#51054=CARTESIAN_POINT('Ctrl Pts',(0.345055249932482,-0.142090346949399,
-2.84));
#51055=CARTESIAN_POINT('Ctrl Pts',(0.33482754435563,-0.160464142324307,
-2.84));
#51056=CARTESIAN_POINT('Ctrl Pts',(0.323210439908307,-0.177847734349123,
-2.84));
#51057=CARTESIAN_POINT('Ctrl Pts',(0.311907287961945,-0.194761534420477,
-2.84));
#51058=CARTESIAN_POINT('Ctrl Pts',(0.299287886823657,-0.21073895330334,
-2.84));
#51059=CARTESIAN_POINT('Ctrl Pts',(0.285412291186548,-0.225549742408173,
-2.84));
#51060=CARTESIAN_POINT('Ctrl Pts',(0.281533606021401,-0.229689844893676,
-2.84));
#51061=CARTESIAN_POINT('Ctrl Pts',(0.277556615451261,-0.233738512703413,
-2.84));
#51062=CARTESIAN_POINT('Ctrl Pts',(0.273482321259015,-0.237690020765659,
-2.84));
#51063=CARTESIAN_POINT('Ctrl Pts',(0.269826094885338,-0.241236060229495,
-2.84));
#51064=CARTESIAN_POINT('Ctrl Pts',(0.266098715359341,-0.244696844003723,
-2.84));
#51065=CARTESIAN_POINT('Ctrl Pts',(0.262302171233473,-0.248068629162198,
-2.84));
#51066=CARTESIAN_POINT('Ctrl Pts',(0.251922843610169,-0.257286713207833,
-2.84));
#51067=CARTESIAN_POINT('Ctrl Pts',(0.241025467094922,-0.265841912499015,
-2.84));
#51068=CARTESIAN_POINT('Ctrl Pts',(0.229633058917296,-0.273663333948482,
-2.84));
#51069=CARTESIAN_POINT('Ctrl Pts',(0.212684455368641,-0.285299343584647,
-2.84));
#51070=CARTESIAN_POINT('Ctrl Pts',(0.194639964930078,-0.29531383338317,
-2.84));
#51071=CARTESIAN_POINT('Ctrl Pts',(0.175745617012724,-0.303666873318378,
-2.84));
#51072=CARTESIAN_POINT('Ctrl Pts',(0.170555727357543,-0.305961281981682,
-2.84));
#51073=CARTESIAN_POINT('Ctrl Pts',(0.165301681301442,-0.308130013924166,
-2.84));
#51074=CARTESIAN_POINT('Ctrl Pts',(0.159988579735579,-0.310171507406792,
-2.84));
#51075=CARTESIAN_POINT('Ctrl Pts',(0.154889918181581,-0.312130604970348,
-2.84));
#51076=CARTESIAN_POINT('Ctrl Pts',(0.149744225546196,-0.313969589980248,
-2.84));
#51077=CARTESIAN_POINT('Ctrl Pts',(0.144562864921253,-0.315686056767363,
-2.84));
#51078=CARTESIAN_POINT('Ctrl Pts',(0.12515058641648,-0.322116902587143,
-2.84));
#51079=CARTESIAN_POINT('Ctrl Pts',(0.105209092186283,-0.326843744021275,
-2.84));
#51080=CARTESIAN_POINT('Ctrl Pts',(0.0849853735125539,-0.329835823811007,
-2.84));
#51081=CARTESIAN_POINT('Ctrl Pts',(0.0684594127471476,-0.332280823863164,
-2.84));
#51082=CARTESIAN_POINT('Ctrl Pts',(0.0517442313050582,-0.333566343194817,
-2.84));
#51083=CARTESIAN_POINT('Ctrl Pts',(0.0349800186612873,-0.333646455380123,
-2.84));
#51084=CARTESIAN_POINT('Ctrl Pts',(0.0295813726058093,-0.333672254225699,
-2.84));
#51085=CARTESIAN_POINT('Ctrl Pts',(0.0241763134870444,-0.333572565689335,
-2.84));
#51086=CARTESIAN_POINT('Ctrl Pts',(0.0187879591158384,-0.333346693379246,
-2.84));
#51087=CARTESIAN_POINT('Ctrl Pts',(-0.000865993468952917,-0.332522827061838,
-2.84));
#51088=CARTESIAN_POINT('Ctrl Pts',(-0.0203544443771316,-0.330026027060492,
-2.84));
#51089=CARTESIAN_POINT('Ctrl Pts',(-0.0394503020694342,-0.325804718223723,
-2.84));
#51090=CARTESIAN_POINT('Ctrl Pts',(-0.057164691519548,-0.321888795203734,
-2.84));
#51091=CARTESIAN_POINT('Ctrl Pts',(-0.0745422208533479,-0.316488228952411,
-2.84));
#51092=CARTESIAN_POINT('Ctrl Pts',(-0.0913773650560324,-0.30951939268376,
-2.84));
#51093=CARTESIAN_POINT('Ctrl Pts',(-0.0926902647827869,-0.308975923431418,
-2.84));
#51094=CARTESIAN_POINT('Ctrl Pts',(-0.0939998487070982,-0.308422896049449,
-2.84));
#51095=CARTESIAN_POINT('Ctrl Pts',(-0.0953060101009229,-0.307860260611276,
-2.84));
#51096=CARTESIAN_POINT('Origin',(0.,0.,-2.84));
#51097=CARTESIAN_POINT('Origin',(0.,0.,-3.17777734492731));
#51098=CARTESIAN_POINT('Ctrl Pts',(-0.0953060101009229,-0.307860260611276,
-2.84));
#51099=CARTESIAN_POINT('Ctrl Pts',(0.00717381913557572,-0.339585510310479,
-2.83337760768562));
#51100=CARTESIAN_POINT('Ctrl Pts',(0.244531614604281,-0.292083776802967,
-2.82013282305686));
#51101=CARTESIAN_POINT('Ctrl Pts',(0.378255106318521,0.0481000370439281,
-2.80026564611372));
#51102=CARTESIAN_POINT('Ctrl Pts',(0.164216515677071,0.34372885516354,-2.78039846917058));
#51103=CARTESIAN_POINT('Ctrl Pts',(-0.199989402997138,0.324342678219355,
-2.76053129222744));
#51104=CARTESIAN_POINT('Ctrl Pts',(-0.321845227690632,0.110984795593872,
-2.74715758414635));
#51105=CARTESIAN_POINT('Ctrl Pts',(-0.322813262032044,0.00211343905450969,
-2.74040626837964));
#51106=CARTESIAN_POINT('Ctrl Pts',(-0.322809858836148,3.43668072568986E-5,
-2.74027734492731));
#51107=CARTESIAN_POINT('Ctrl Pts',(-0.116310150563007,-0.375708449300798,
-2.88100630286919));
#51108=CARTESIAN_POINT('Ctrl Pts',(0.00875483070676231,-0.414425509906482,
-2.87438391055481));
#51109=CARTESIAN_POINT('Ctrl Pts',(0.298423036300873,-0.356455044346,-2.86113912592605));
#51110=CARTESIAN_POINT('Ctrl Pts',(0.461617355721276,0.0587006270091591,
-2.84127194898291));
#51111=CARTESIAN_POINT('Ctrl Pts',(0.200407588599154,0.419481991267769,
-2.82140477203977));
#51112=CARTESIAN_POINT('Ctrl Pts',(-0.244064330769604,0.395823366204863,
-2.80153759509663));
#51113=CARTESIAN_POINT('Ctrl Pts',(-0.464980723451366,0.00901991303881209,
-2.78167041815349));
#51114=CARTESIAN_POINT('Ctrl Pts',(-0.259321715654258,-0.385984470229777,
-2.76180324121035));
#51115=CARTESIAN_POINT('Ctrl Pts',(0.184085419273639,-0.427041120788341,
-2.7419360642672));
#51116=CARTESIAN_POINT('Ctrl Pts',(0.458707595804344,-0.07644057108933,
-2.72206888732406));
#51117=CARTESIAN_POINT('Ctrl Pts',(0.312630362980567,0.344253201275889,
-2.70220171038092));
#51118=CARTESIAN_POINT('Ctrl Pts',(-0.120148330577789,0.449238960762277,
-2.68233453343778));
#51119=CARTESIAN_POINT('Ctrl Pts',(-0.442745013212915,0.142226606977436,
-2.66246735649464));
#51120=CARTESIAN_POINT('Ctrl Pts',(-0.359299014024003,-0.295219785168938,
-2.6426001795515));
#51121=CARTESIAN_POINT('Ctrl Pts',(0.0536572306457554,-0.461921985183017,
-2.62273300260836));
#51122=CARTESIAN_POINT('Ctrl Pts',(0.417405425637388,-0.204996889107976,
-2.60286582566521));
#51123=CARTESIAN_POINT('Ctrl Pts',(0.398352272201653,0.239929871442676,
-2.58299864872208));
#51124=CARTESIAN_POINT('Ctrl Pts',(0.0139719758106573,0.464817963519448,
-2.56313147177893));
#51125=CARTESIAN_POINT('Ctrl Pts',(-0.383222079658351,0.263423206510685,
-2.5432642948358));
#51126=CARTESIAN_POINT('Ctrl Pts',(-0.42896455902559,-0.179555945670809,
-2.52339711789265));
#51127=CARTESIAN_POINT('Ctrl Pts',(-0.0813052976463755,-0.457865035790148,
-2.50352994094951));
#51128=CARTESIAN_POINT('Ctrl Pts',(0.340918760207331,-0.316267828616965,
-2.48366276400637));
#51129=CARTESIAN_POINT('Ctrl Pts',(0.450487506537335,0.115377401546258,
-2.46379558706323));
#51130=CARTESIAN_POINT('Ctrl Pts',(0.14691587208234,0.441210456141015,-2.44392841012008));
#51131=CARTESIAN_POINT('Ctrl Pts',(-0.291391754232848,0.362411072184382,
-2.42406123317695));
#51132=CARTESIAN_POINT('Ctrl Pts',(-0.462465105737489,-0.0487541321641203,
-2.4041940562338));
#51133=CARTESIAN_POINT('Ctrl Pts',(-0.209413461852369,-0.415207106963557,
-2.38432687929066));
#51134=CARTESIAN_POINT('Ctrl Pts',(0.235690474676962,-0.400875217182329,
-2.36445970234752));
#51135=CARTESIAN_POINT('Ctrl Pts',(0.464643569830363,-0.0189021848768118,
-2.34459252540438));
#51136=CARTESIAN_POINT('Ctrl Pts',(0.26747380789293,0.380405969595911,-2.32472534846124));
#51137=CARTESIAN_POINT('Ctrl Pts',(-0.174995169749528,0.430845250832214,
-2.3048581715181));
#51138=CARTESIAN_POINT('Ctrl Pts',(-0.456976740313732,0.0861579851791214,
-2.28499099457496));
#51139=CARTESIAN_POINT('Ctrl Pts',(-0.31986667400783,-0.337544442202628,
-2.26512381763182));
#51140=CARTESIAN_POINT('Ctrl Pts',(0.110591906940626,-0.451686140721507,
-2.24525664068867));
#51141=CARTESIAN_POINT('Ctrl Pts',(0.439627069105229,-0.151588191197238,
-2.22538946374554));
#51142=CARTESIAN_POINT('Ctrl Pts',(0.365481912109643,0.287530714049526,
-2.20552228680239));
#51143=CARTESIAN_POINT('Ctrl Pts',(-0.043845321532473,0.462956291004388,
-2.18565510985925));
#51144=CARTESIAN_POINT('Ctrl Pts',(-0.412962176943286,0.213806407797088,
-2.16578793291611));
#51145=CARTESIAN_POINT('Ctrl Pts',(-0.403352984750648,-0.231424521807137,
-2.14592075597297));
#51146=CARTESIAN_POINT('Ctrl Pts',(-0.0238302987011413,-0.464416899417628,
-2.12605357902982));
#51147=CARTESIAN_POINT('Ctrl Pts',(0.377547063985032,-0.271494298424763,
-2.10618640208669));
#51148=CARTESIAN_POINT('Ctrl Pts',(0.432677444960194,0.170414694858164,
-2.08631922514354));
#51149=CARTESIAN_POINT('Ctrl Pts',(0.0910009807419794,0.456037017252848,
-2.0664520482004));
#51150=CARTESIAN_POINT('Ctrl Pts',(-0.33413213807732,0.323429519222901,
-2.04658487125727));
#51151=CARTESIAN_POINT('Ctrl Pts',(-0.452833939219847,-0.105793965288736,
-2.02671769431412));
#51152=CARTESIAN_POINT('Ctrl Pts',(-0.15624345066412,-0.437994205127701,
-2.00685051737098));
#51153=CARTESIAN_POINT('Ctrl Pts',(0.283637314429727,-0.368511619170916,
-1.98698334042784));
#51154=CARTESIAN_POINT('Ctrl Pts',(0.463395373269886,0.0389315762966344,
-1.9671161634847));
#51155=CARTESIAN_POINT('Ctrl Pts',(0.2181752912658,0.41067077066911,-1.94724898654156));
#51156=CARTESIAN_POINT('Ctrl Pts',(-0.227132523608876,0.405785357448913,
-1.92738180959842));
#51157=CARTESIAN_POINT('Ctrl Pts',(-0.464137961773493,0.0287557305875891,
-1.90751463265527));
#51158=CARTESIAN_POINT('Ctrl Pts',(-0.275484233991155,-0.374645667829196,
-1.88764745571213));
#51159=CARTESIAN_POINT('Ctrl Pts',(0.165815040869781,-0.434460943954955,
-1.86778027876899));
#51160=CARTESIAN_POINT('Ctrl Pts',(0.455045970085387,-0.0958337347176189,
-1.84791310182585));
#51161=CARTESIAN_POINT('Ctrl Pts',(0.326955964478182,0.330682229478725,
-1.82804592488271));
#51162=CARTESIAN_POINT('Ctrl Pts',(-0.100984117191286,0.453930774101045,
-1.80817874793956));
#51163=CARTESIAN_POINT('Ctrl Pts',(-0.436312047651907,0.160881125911892,
-1.78831157099643));
#51164=CARTESIAN_POINT('Ctrl Pts',(-0.371499852563495,-0.279711993211197,
-1.76844439405328));
#51165=CARTESIAN_POINT('Ctrl Pts',(0.0340134495564639,-0.463782303295574,
-1.74857721711015));
#51166=CARTESIAN_POINT('Ctrl Pts',(0.408333145978101,-0.222519620475373,
-1.728710040167));
#51167=CARTESIAN_POINT('Ctrl Pts',(0.408172061553041,0.222814963071199,
-1.70884286322386));
#51168=CARTESIAN_POINT('Ctrl Pts',(0.0336779261970881,0.463806788315934,
-1.68897568628072));
#51169=CARTESIAN_POINT('Ctrl Pts',(-0.371702107655723,0.279443165536699,
-1.66910850933758));
#51170=CARTESIAN_POINT('Ctrl Pts',(-0.436195547098329,-0.161196725439652,
-1.64924133239443));
#51171=CARTESIAN_POINT('Ctrl Pts',(-0.100655703208124,-0.45400371035109,
-1.6293741554513));
#51172=CARTESIAN_POINT('Ctrl Pts',(0.327195104671456,-0.33044561289252,
-1.60950697850816));
#51173=CARTESIAN_POINT('Ctrl Pts',(0.454976521923715,0.0961629039654941,
-1.58963980156502));
#51174=CARTESIAN_POINT('Ctrl Pts',(0.165500694999069,0.434580785994621,
-1.56977262462187));
#51175=CARTESIAN_POINT('Ctrl Pts',(-0.275755192164056,0.374446275980204,
-1.54990544767873));
#51176=CARTESIAN_POINT('Ctrl Pts',(-0.464117037534976,-0.0290914948161029,
-1.53003827073559));
#51177=CARTESIAN_POINT('Ctrl Pts',(-0.226838906498796,-0.405949565955315,
-1.51017109379245));
#51178=CARTESIAN_POINT('Ctrl Pts',(0.218472326108414,-0.41051282845443,
-1.49030391684931));
#51179=CARTESIAN_POINT('Ctrl Pts',(0.463423416316454,-0.0385963315674505,
-1.47043673990617));
#51180=CARTESIAN_POINT('Ctrl Pts',(0.283370647508505,0.368716714743839,
-1.45056956296303));
#51181=CARTESIAN_POINT('Ctrl Pts',(-0.156560268330182,0.437881059171619,
-1.43070238601989));
#51182=CARTESIAN_POINT('Ctrl Pts',(-0.452910355349746,0.105466343531221,
-1.41083520907674));
#51183=CARTESIAN_POINT('Ctrl Pts',(-0.333898071727896,-0.323671156109517,
-1.3909680321336));
#51184=CARTESIAN_POINT('Ctrl Pts',(0.0913308682086396,-0.455971064995503,
-1.37110085519046));
#51185=CARTESIAN_POINT('Ctrl Pts',(0.432800614998476,-0.17010163802215,
-1.35123367824732));
#51186=CARTESIAN_POINT('Ctrl Pts',(0.377350557819586,0.271767356601424,
-1.33136650130418));
#51187=CARTESIAN_POINT('Ctrl Pts',(-0.0241662660106598,0.464399538315856,
-1.31149932436104));
#51188=CARTESIAN_POINT('Ctrl Pts',(-0.403520298857715,0.231132663227545,
-1.2916321474179));
#51189=CARTESIAN_POINT('Ctrl Pts',(-0.412807394714464,-0.21410510145705,
-1.27176497047476));
#51190=CARTESIAN_POINT('Ctrl Pts',(-0.0435103931630265,-0.462987888921166,
-1.25189779353161));
#51191=CARTESIAN_POINT('Ctrl Pts',(0.365689825080772,-0.28726623789313,
-1.23203061658847));
#51192=CARTESIAN_POINT('Ctrl Pts',(0.439517290481023,0.151906191345506,
-1.21216343964533));
#51193=CARTESIAN_POINT('Ctrl Pts',(0.110265114279544,0.451766028131595,
-1.19229626270219));
#51194=CARTESIAN_POINT('Ctrl Pts',(-0.320110780391191,0.337312952431746,
-1.17242908575905));
#51195=CARTESIAN_POINT('Ctrl Pts',(-0.456914291386833,-0.0864885537360078,
-1.15256190881591));
#51196=CARTESIAN_POINT('Ctrl Pts',(-0.17468343717389,-0.430971735010537,
-1.13269473187277));
#51197=CARTESIAN_POINT('Ctrl Pts',(0.267748935329152,-0.380212371222958,
-1.11282755492963));
#51198=CARTESIAN_POINT('Ctrl Pts',(0.464629773844524,0.0192383174437102,
-1.09296037798648));
#51199=CARTESIAN_POINT('Ctrl Pts',(0.235400407426262,0.401045618084062,
-1.07309320104334));
#51200=CARTESIAN_POINT('Ctrl Pts',(-0.20971378062082,0.415055502094117,
-1.0532260241002));
#51201=CARTESIAN_POINT('Ctrl Pts',(-0.462500255145941,0.0484195579370409,
-1.03335884715706));
#51202=CARTESIAN_POINT('Ctrl Pts',(-0.29112949826634,-0.36262177932395,
-1.01349167021392));
#51203=CARTESIAN_POINT('Ctrl Pts',(0.147235018272768,-0.441104056878981,
-0.993624493270776));
#51204=CARTESIAN_POINT('Ctrl Pts',(0.450570857483482,-0.115051475381576,
-0.97375731632764));
#51205=CARTESIAN_POINT('Ctrl Pts',(0.340689870680686,0.316514378214412,
-0.953890139384495));
#51206=CARTESIAN_POINT('Ctrl Pts',(-0.0816365055196882,0.457806094943495,
-0.934022962441356));
#51207=CARTESIAN_POINT('Ctrl Pts',(-0.429094351859766,0.179245576801561,
-0.914155785498213));
#51208=CARTESIAN_POINT('Ctrl Pts',(-0.383031394111188,-0.263700380595324,
-0.894288608555073));
#51209=CARTESIAN_POINT('Ctrl Pts',(0.0143082037249251,-0.464807718209417,
-0.874421431611931));
#51210=CARTESIAN_POINT('Ctrl Pts',(0.398525802144136,-0.239641658787132,
-0.85455425466879));
#51211=CARTESIAN_POINT('Ctrl Pts',(0.417256897583025,0.205298857815313,
-0.834687077725648));
#51212=CARTESIAN_POINT('Ctrl Pts',(0.0533232733938106,0.461960569870896,
-0.814819900782508));
#51213=CARTESIAN_POINT('Ctrl Pts',(-0.359512922762638,0.294959993842442,
-0.794952723839367));
#51214=CARTESIAN_POINT('Ctrl Pts',(-0.442641179784937,-0.142547274823183,
-0.775085546896225));
#51215=CARTESIAN_POINT('Ctrl Pts',(-0.119824888162353,-0.44932497791433,
-0.755218369953084));
#51216=CARTESIAN_POINT('Ctrl Pts',(0.312882354331519,-0.344028446423828,
-0.735351193009943));
#51217=CARTESIAN_POINT('Ctrl Pts',(0.458646375298876,0.076775269627352,
-0.715484016066801));
#51218=CARTESIAN_POINT('Ctrl Pts',(0.183787543464457,0.42716867683364,-0.69561683912366));
#51219=CARTESIAN_POINT('Ctrl Pts',(-0.259622148038332,0.385807309221348,
-0.67574966218052));
#51220=CARTESIAN_POINT('Ctrl Pts',(-0.464933351385975,-0.00937647970841039,
-0.655882485237378));
#51221=CARTESIAN_POINT('Ctrl Pts',(-0.243855939980186,-0.395961134625949,
-0.636015308294237));
#51222=CARTESIAN_POINT('Ctrl Pts',(0.200860829905182,-0.419411333430728,
-0.616148131351095));
#51223=CARTESIAN_POINT('Ctrl Pts',(0.461368893847993,-0.0582209876456167,
-0.596280954407956));
#51224=CARTESIAN_POINT('Ctrl Pts',(0.298757293496838,0.356363605268922,
-0.576413777464811));
#51225=CARTESIAN_POINT('Ctrl Pts',(-0.13784348852236,0.444128486224894,
-0.556546600521672));
#51226=CARTESIAN_POINT('Ctrl Pts',(-0.44802852973673,0.124584815366827,
-0.53667942357853));
#51227=CARTESIAN_POINT('Ctrl Pts',(-0.347328303740341,-0.30921511743238,
-0.516812246635389));
#51228=CARTESIAN_POINT('Ctrl Pts',(0.071905392806198,-0.459435038021824,
-0.496945069692248));
#51229=CARTESIAN_POINT('Ctrl Pts',(0.425194927333323,-0.1883088257302,-0.477077892749107));
#51230=CARTESIAN_POINT('Ctrl Pts',(0.388539802842457,0.255514696134952,
-0.457210715805966));
#51231=CARTESIAN_POINT('Ctrl Pts',(-0.00444369794125631,0.465006660197467,
-0.437343538862825));
#51232=CARTESIAN_POINT('Ctrl Pts',(-0.393351908929444,0.248042774871675,
-0.417476361919683));
#51233=CARTESIAN_POINT('Ctrl Pts',(-0.421518558049922,-0.196400192834101,
-0.397609184976542));
#51234=CARTESIAN_POINT('Ctrl Pts',(-0.0631121669455817,-0.460725300422581,
-0.377742008033401));
#51235=CARTESIAN_POINT('Ctrl Pts',(0.353174214709179,-0.302520956931872,
-0.35787483109026));
#51236=CARTESIAN_POINT('Ctrl Pts',(0.445565744803263,0.133124163984721,
-0.338007654147118));
#51237=CARTESIAN_POINT('Ctrl Pts',(0.129330843850922,0.446681706278964,
-0.318140477203977));
#51238=CARTESIAN_POINT('Ctrl Pts',(-0.305513314896439,0.350588980455718,
-0.298273300260836));
#51239=CARTESIAN_POINT('Ctrl Pts',(-0.460171545064611,-0.0670272492846139,
-0.278406123317694));
#51240=CARTESIAN_POINT('Ctrl Pts',(-0.192809775000032,-0.423173658350396,
-0.258538946374554));
#51241=CARTESIAN_POINT('Ctrl Pts',(0.251380134241884,-0.391227930132719,
-0.238671769431412));
#51242=CARTESIAN_POINT('Ctrl Pts',(0.465024482747802,-0.000490806679507694,
-0.218804592488271));
#51243=CARTESIAN_POINT('Ctrl Pts',(0.252207730484799,0.39070075510648,-0.19893741554513));
#51244=CARTESIAN_POINT('Ctrl Pts',(-0.191929009959531,0.423573860819181,
-0.179070238601988));
#51245=CARTESIAN_POINT('Ctrl Pts',(-0.460007725025938,0.0680048261882178,
-0.159203061658848));
#51246=CARTESIAN_POINT('Ctrl Pts',(-0.306292952616749,-0.349961511012139,
-0.139335884715706));
#51247=CARTESIAN_POINT('Ctrl Pts',(0.128471060887831,-0.446921381567406,
-0.119468707772565));
#51248=CARTESIAN_POINT('Ctrl Pts',(0.445128579067042,-0.134122670208492,
-0.099601530829424));
#51249=CARTESIAN_POINT('Ctrl Pts',(0.354113939546637,0.301893465535662,
-0.0797343538862821));
#51250=CARTESIAN_POINT('Ctrl Pts',(-0.0627678983065788,0.460626419321466,
-0.0598671769431416));
#51251=CARTESIAN_POINT('Ctrl Pts',(-0.300608260002571,0.285411675199489,
-0.0466223923143805));
#51252=CARTESIAN_POINT('Ctrl Pts',(-0.356151197810523,0.166856867698425,
-0.04));
#51253=CARTESIAN_POINT('Ctrl Pts',(-0.109308770408979,-0.353092386404291,
-2.86733753524613));
#51254=CARTESIAN_POINT('Ctrl Pts',(0.00822782684970018,-0.389478843374481,
-2.86071514293175));
#51255=CARTESIAN_POINT('Ctrl Pts',(0.280459229068676,-0.334997955164989,
-2.84747035830299));
#51256=CARTESIAN_POINT('Ctrl Pts',(0.433829939253691,0.0551670970207491,
-2.82760318135984));
#51257=CARTESIAN_POINT('Ctrl Pts',(0.188343897625126,0.394230945899693,
-2.80773600441671));
#51258=CARTESIAN_POINT('Ctrl Pts',(-0.229372688178782,0.371996470209694,
-2.78786882747356));
#51259=CARTESIAN_POINT('Ctrl Pts',(-0.436990846442185,0.00847695234419238,
-2.76800165053043));
#51260=CARTESIAN_POINT('Ctrl Pts',(-0.243711642890173,-0.362749834245313,
-2.74813447358728));
#51261=CARTESIAN_POINT('Ctrl Pts',(0.173004254002082,-0.401335047727919,
-2.72826729664414));
#51262=CARTESIAN_POINT('Ctrl Pts',(0.431095334602544,-0.0718391713422158,
-2.708400119701));
#51263=CARTESIAN_POINT('Ctrl Pts',(0.293811334647068,0.32353061154742,-2.68853294275786));
#51264=CARTESIAN_POINT('Ctrl Pts',(-0.112915908186665,0.422196671425773,
-2.66866576581472));
#51265=CARTESIAN_POINT('Ctrl Pts',(-0.4160936321099,0.13366516553276,-2.64879858887158));
#51266=CARTESIAN_POINT('Ctrl Pts',(-0.337670729871909,-0.277448800134932,
-2.62893141192843));
#51267=CARTESIAN_POINT('Ctrl Pts',(0.0504272918317754,-0.434116231307584,
-2.6090642349853));
#51268=CARTESIAN_POINT('Ctrl Pts',(0.392279380755707,-0.192656941613362,
-2.58919705804215));
#51269=CARTESIAN_POINT('Ctrl Pts',(0.374373146739222,0.225487105853035,
-2.56932988109901));
#51270=CARTESIAN_POINT('Ctrl Pts',(0.0131309218383279,0.436837883971209,
-2.54946270415587));
#51271=CARTESIAN_POINT('Ctrl Pts',(-0.360153727927074,0.247566241308192,
-2.52959552721272));
#51272=CARTESIAN_POINT('Ctrl Pts',(-0.403142703101535,-0.168747435592608,
-2.50972835026959));
#51273=CARTESIAN_POINT('Ctrl Pts',(-0.0764110618930625,-0.430303493145013,
-2.48986117332644));
#51274=CARTESIAN_POINT('Ctrl Pts',(0.320396889757525,-0.297229840204795,
-2.46999399638331));
#51275=CARTESIAN_POINT('Ctrl Pts',(0.423370060014906,0.108432168946187,
-2.45012681944016));
#51276=CARTESIAN_POINT('Ctrl Pts',(0.138072156670315,0.414651448896828,
-2.43025964249702));
#51277=CARTESIAN_POINT('Ctrl Pts',(-0.273851200504237,0.340595455266087,
-2.41039246555388));
#51278=CARTESIAN_POINT('Ctrl Pts',(-0.434626658297024,-0.0458193391842438,
-2.39052528861074));
#51279=CARTESIAN_POINT('Ctrl Pts',(-0.196807655319557,-0.390213391587604,
-2.37065811166759));
#51280=CARTESIAN_POINT('Ctrl Pts',(0.22150290287941,-0.376744221080646,
-2.35079093472446));
#51281=CARTESIAN_POINT('Ctrl Pts',(0.436673988046143,-0.0177643531276166,
-2.33092375778131));
#51282=CARTESIAN_POINT('Ctrl Pts',(0.251373013583586,0.357507135804446,
-2.31105658083818));
#51283=CARTESIAN_POINT('Ctrl Pts',(-0.164461199132137,0.40491018519923,
-2.29118940389503));
#51284=CARTESIAN_POINT('Ctrl Pts',(-0.429468669307051,0.0809716381180591,
-2.27132222695189));
#51285=CARTESIAN_POINT('Ctrl Pts',(-0.300612050292764,-0.317225691454733,
-2.25145505000875));
#51286=CARTESIAN_POINT('Ctrl Pts',(0.103934740917693,-0.424496541480263,
-2.23158787306561));
#51287=CARTESIAN_POINT('Ctrl Pts',(0.413163375077601,-0.142463221894937,
-2.21172069612247));
#51288=CARTESIAN_POINT('Ctrl Pts',(0.343481443588932,0.270222578643672,
-2.19185351917933));
#51289=CARTESIAN_POINT('Ctrl Pts',(-0.0412060182340209,0.435088276283999,
-2.17198634223619));
#51290=CARTESIAN_POINT('Ctrl Pts',(-0.388103596879385,0.200936164459697,
-2.15211916529305));
#51291=CARTESIAN_POINT('Ctrl Pts',(-0.379072837499258,-0.217493742367056,
-2.1322519883499));
#51292=CARTESIAN_POINT('Ctrl Pts',(-0.0223958152997948,-0.436460962235547,
-2.11238481140677));
#51293=CARTESIAN_POINT('Ctrl Pts',(0.354820324244769,-0.255151487554673,
-2.09251763446362));
#51294=CARTESIAN_POINT('Ctrl Pts',(0.406632088973841,0.160156449496438,
-2.07265045752049));
#51295=CARTESIAN_POINT('Ctrl Pts',(0.0855231057888487,0.428585513608147,
-2.05278328057734));
#51296=CARTESIAN_POINT('Ctrl Pts',(-0.314018793635468,0.303960427263576,
-2.0329161036342));
#51297=CARTESIAN_POINT('Ctrl Pts',(-0.425575247353511,-0.0994256151025911,
-2.01304892669105));
#51298=CARTESIAN_POINT('Ctrl Pts',(-0.146838254390352,-0.411628802619697,
-1.99318174974792));
#51299=CARTESIAN_POINT('Ctrl Pts',(0.266563545248126,-0.34632877507259,
-1.97331457280477));
#51300=CARTESIAN_POINT('Ctrl Pts',(0.435500927650348,0.0365880597219514,
-1.95344739586163));
#51301=CARTESIAN_POINT('Ctrl Pts',(0.205042059583323,0.385950123591584,
-1.93358021891849));
#51302=CARTESIAN_POINT('Ctrl Pts',(-0.213460104345107,0.381358791627395,
-1.91371304197535));
#51303=CARTESIAN_POINT('Ctrl Pts',(-0.436198815460278,0.0270247569754325,
-1.89384586503221));
#51304=CARTESIAN_POINT('Ctrl Pts',(-0.258901245840276,-0.3520935798916,
-1.87397868808907));
#51305=CARTESIAN_POINT('Ctrl Pts',(0.15583367526441,-0.408308228856726,
-1.85411151114593));
#51306=CARTESIAN_POINT('Ctrl Pts',(0.427654123297258,-0.090064948372743,
-1.83424433420278));
#51307=CARTESIAN_POINT('Ctrl Pts',(0.307274595398546,0.310776554973491,
-1.81437715725965));
#51308=CARTESIAN_POINT('Ctrl Pts',(-0.0949052995596975,0.426606057404268,
-1.7945099803165));
#51309=CARTESIAN_POINT('Ctrl Pts',(-0.410047903924069,0.151196761162428,
-1.77464280337336));
#51310=CARTESIAN_POINT('Ctrl Pts',(-0.349137129427362,-0.262874511799361,
-1.75477562643022));
#51311=CARTESIAN_POINT('Ctrl Pts',(0.0319659834536178,-0.435864566121603,
-1.73490844948708));
#51312=CARTESIAN_POINT('Ctrl Pts',(0.383753214040569,-0.209124878510576,
-1.71504127254394));
#51313=CARTESIAN_POINT('Ctrl Pts',(0.383601826218008,0.209402442728685,
-1.6951740956008));
#51314=CARTESIAN_POINT('Ctrl Pts',(0.0316506571843346,0.435887577247082,
-1.67530691865766));
#51315=CARTESIAN_POINT('Ctrl Pts',(-0.349327209616696,0.262621866416228,
-1.65543974171451));
#51316=CARTESIAN_POINT('Ctrl Pts',(-0.409938416212103,-0.151493362930668,
-1.63557256477137));
#51317=CARTESIAN_POINT('Ctrl Pts',(-0.0945966547121861,-0.426674603199902,
-1.61570538782823));
#51318=CARTESIAN_POINT('Ctrl Pts',(0.307499340361523,-0.310554181707088,
-1.59583821088509));
#51319=CARTESIAN_POINT('Ctrl Pts',(0.427588855621798,0.0903743030212203,
-1.57597103394195));
#51320=CARTESIAN_POINT('Ctrl Pts',(0.155538251688356,0.408420856911421,
-1.55610385699881));
#51321=CARTESIAN_POINT('Ctrl Pts',(-0.259155893474801,0.351906190590346,
-1.53623668005567));
#51322=CARTESIAN_POINT('Ctrl Pts',(-0.436179150772605,-0.0273403096145494,
-1.51636950311253));
#51323=CARTESIAN_POINT('Ctrl Pts',(-0.213184161745785,-0.381513115474785,
-1.49650232616938));
#51324=CARTESIAN_POINT('Ctrl Pts',(0.205321214182107,-0.385801688831601,
-1.47663514922625));
#51325=CARTESIAN_POINT('Ctrl Pts',(0.435527282623873,-0.0362729953104975,
-1.4567679722831));
#51326=CARTESIAN_POINT('Ctrl Pts',(0.266312930550041,0.346521524757669,
-1.43690079533996));
#51327=CARTESIAN_POINT('Ctrl Pts',(-0.147136000970108,0.411522467572615,
-1.41703361839682));
#51328=CARTESIAN_POINT('Ctrl Pts',(-0.425647063554919,0.0991177147920855,
-1.39716644145368));
#51329=CARTESIAN_POINT('Ctrl Pts',(-0.313798817092356,-0.304187518629494,
-1.37729926451054));
#51330=CARTESIAN_POINT('Ctrl Pts',(0.085833135422371,-0.42852353139833,
-1.3574320875674));
#51331=CARTESIAN_POINT('Ctrl Pts',(0.406747844695681,-0.159862237360634,
-1.33756491062426));
#51332=CARTESIAN_POINT('Ctrl Pts',(0.35463564692109,0.255408108781595,-1.31769773368111));
#51333=CARTESIAN_POINT('Ctrl Pts',(-0.0227115587952971,0.436444646198827,
-1.29783055673797));
#51334=CARTESIAN_POINT('Ctrl Pts',(-0.379230080003261,0.217219452442108,
-1.27796337979483));
#51335=CARTESIAN_POINT('Ctrl Pts',(-0.38795813188745,-0.201216878022024,
-1.25809620285169));
#51336=CARTESIAN_POINT('Ctrl Pts',(-0.0408912511387834,-0.435117972139552,
-1.23822902590855));
#51337=CARTESIAN_POINT('Ctrl Pts',(0.343676841076736,-0.269974022835617,
-1.21836184896541));
#51338=CARTESIAN_POINT('Ctrl Pts',(0.41306020466323,0.142762079776462,-1.19849467202227));
#51339=CARTESIAN_POINT('Ctrl Pts',(0.103627619795515,0.424571620005444,
-1.17862749507913));
#51340=CARTESIAN_POINT('Ctrl Pts',(-0.300841462502146,0.317008136391009,
-1.15876031813598));
#51341=CARTESIAN_POINT('Ctrl Pts',(-0.429409979541973,-0.0812823078430504,
-1.13889314119285));
#51342=CARTESIAN_POINT('Ctrl Pts',(-0.164168231541823,-0.40502905556387,
-1.1190259642497));
#51343=CARTESIAN_POINT('Ctrl Pts',(0.251631579509376,-0.357325191236424,
-1.09915878730656));
#51344=CARTESIAN_POINT('Ctrl Pts',(0.436661022520423,0.0180802519327009,
-1.07929161036342));
#51345=CARTESIAN_POINT('Ctrl Pts',(0.221230296452916,0.376904364567306,
-1.05942443342028));
#51346=CARTESIAN_POINT('Ctrl Pts',(-0.197089896165702,0.390070912691426,
-1.03955725647714));
#51347=CARTESIAN_POINT('Ctrl Pts',(-0.434659691859441,0.0455049049134983,
-1.019690079534));
#51348=CARTESIAN_POINT('Ctrl Pts',(-0.27360473124001,-0.340793478725185,
-0.999822902590856));
#51349=CARTESIAN_POINT('Ctrl Pts',(0.138372091607098,-0.414551454421289,
-0.979955725647713));
#51350=CARTESIAN_POINT('Ctrl Pts',(0.423448393585894,-0.108125862160985,
-0.960088548704574));
#51351=CARTESIAN_POINT('Ctrl Pts',(0.320181778414311,0.297461548557087,
-0.940221371761431));
#51352=CARTESIAN_POINT('Ctrl Pts',(-0.0767223324503298,0.430248100288556,
-0.920354194818291));
#51353=CARTESIAN_POINT('Ctrl Pts',(-0.40326468295491,0.168455749619316,
-0.900487017875149));
#51354=CARTESIAN_POINT('Ctrl Pts',(-0.359974520845024,-0.247826730682804,
-0.880619840932009));
#51355=CARTESIAN_POINT('Ctrl Pts',(0.0134469102512725,-0.436828255385598,
-0.860752663988866));
#51356=CARTESIAN_POINT('Ctrl Pts',(0.374536230911585,-0.225216242382897,
-0.840885487045726));
#51357=CARTESIAN_POINT('Ctrl Pts',(0.392139793463325,0.192940733079036,
-0.821018310102584));
#51358=CARTESIAN_POINT('Ctrl Pts',(0.0501134373968655,0.434152493360106,
-0.801151133159443));
#51359=CARTESIAN_POINT('Ctrl Pts',(-0.337871762207323,0.277204647149791,
-0.781283956216302));
#51360=CARTESIAN_POINT('Ctrl Pts',(-0.415996049016037,-0.133966530527635,
-0.76141677927316));
#51361=CARTESIAN_POINT('Ctrl Pts',(-0.112611935639486,-0.422277510708325,
-0.74154960233002));
#51362=CARTESIAN_POINT('Ctrl Pts',(0.294048157182272,-0.323319385988831,
-0.721682425386878));
#51363=CARTESIAN_POINT('Ctrl Pts',(0.431037799313113,0.0721537224409103,
-0.701815248443737));
#51364=CARTESIAN_POINT('Ctrl Pts',(0.172724309059369,0.401454925437667,
-0.681948071500596));
#51365=CARTESIAN_POINT('Ctrl Pts',(-0.243993990512759,0.362583337581848,
-0.662080894557455));
#51366=CARTESIAN_POINT('Ctrl Pts',(-0.436946325975187,-0.00881205520524107,
-0.642213717614313));
#51367=CARTESIAN_POINT('Ctrl Pts',(-0.229176841635333,-0.372125945553308,
-0.622346540671172));
#51368=CARTESIAN_POINT('Ctrl Pts',(0.188769855717525,-0.394164541366216,
-0.602479363728031));
#51369=CARTESIAN_POINT('Ctrl Pts',(0.433596433736497,-0.0547163299224792,
-0.58261218678489));
#51370=CARTESIAN_POINT('Ctrl Pts',(0.280773365392242,0.334912020334415,
-0.562745009841748));
#51371=CARTESIAN_POINT('Ctrl Pts',(-0.129545892308867,0.417393825885778,
-0.542877832898608));
#51372=CARTESIAN_POINT('Ctrl Pts',(-0.421059103239103,0.117085335316459,
-0.523010655955466));
#51373=CARTESIAN_POINT('Ctrl Pts',(-0.326420605822587,-0.290601672466167,
-0.503143479012325));
#51374=CARTESIAN_POINT('Ctrl Pts',(0.0675769916501168,-0.431778987868845,
-0.483276302069183));
#51375=CARTESIAN_POINT('Ctrl Pts',(0.39959998732667,-0.176973429215675,
-0.463409125126043));
#51376=CARTESIAN_POINT('Ctrl Pts',(0.365151346619992,0.240133789877654,
-0.443541948182901));
#51377=CARTESIAN_POINT('Ctrl Pts',(-0.00417620608069359,0.437015221905641,
-0.42367477123976));
#51378=CARTESIAN_POINT('Ctrl Pts',(-0.369673784230984,0.233111646737714,
-0.403807594296618));
#51379=CARTESIAN_POINT('Ctrl Pts',(-0.39614491995729,-0.184577730171128,
-0.383940417353478));
#51380=CARTESIAN_POINT('Ctrl Pts',(-0.0593130808727705,-0.432991581918882,
-0.364073240410336));
#51381=CARTESIAN_POINT('Ctrl Pts',(0.331914617624918,-0.284310472173769,
-0.344206063467196));
#51382=CARTESIAN_POINT('Ctrl Pts',(0.418744567563962,0.125110651189557,
-0.324338886524053));
#51383=CARTESIAN_POINT('Ctrl Pts',(0.121545672917358,0.41979335286896,-0.304471709580913));
#51384=CARTESIAN_POINT('Ctrl Pts',(-0.287122702818704,0.329485003562026,
-0.284604532637771));
#51385=CARTESIAN_POINT('Ctrl Pts',(-0.43247116029623,-0.0629924917793682,
-0.26473735569463));
#51386=CARTESIAN_POINT('Ctrl Pts',(-0.181203440336604,-0.397700390205352,
-0.244870178751489));
#51387=CARTESIAN_POINT('Ctrl Pts',(0.236248111159817,-0.367677659993151,
-0.225003001808348));
#51388=CARTESIAN_POINT('Ctrl Pts',(0.43703197161367,-0.00046126218894694,
-0.205135824865206));
#51389=CARTESIAN_POINT('Ctrl Pts',(0.237025889601942,0.367182218678445,
-0.185268647922066));
#51390=CARTESIAN_POINT('Ctrl Pts',(-0.1803756936341,0.398076502174651,-0.165401470978924));
#51391=CARTESIAN_POINT('Ctrl Pts',(-0.432317201532449,0.0639112226794298,
-0.145534294035783));
#51392=CARTESIAN_POINT('Ctrl Pts',(-0.287855409638866,-0.328895305130591,
-0.125667117092642));
#51393=CARTESIAN_POINT('Ctrl Pts',(0.120737645259763,-0.420018600716635,
-0.1057999401495));
#51394=CARTESIAN_POINT('Ctrl Pts',(0.418333717359917,-0.126049051553048,
-0.0859327632063595));
#51395=CARTESIAN_POINT('Ctrl Pts',(0.332797774993454,0.28372075311116,-0.0660655862632178));
#51396=CARTESIAN_POINT('Ctrl Pts',(-0.0589895357527821,0.432898653042708,
-0.0461984093200771));
#51397=CARTESIAN_POINT('Ctrl Pts',(-0.282512911526698,0.268231096988586,
-0.0329536246913161));
#51398=CARTESIAN_POINT('Ctrl Pts',(-0.334712398908504,0.156812788515205,
-0.0263312323769356));
#51399=CARTESIAN_POINT('Ctrl Pts',(-0.102307390254951,-0.330476323507783,
-2.85366876762306));
#51400=CARTESIAN_POINT('Ctrl Pts',(0.0077008229926378,-0.36453217684248,
-2.84704637530868));
#51401=CARTESIAN_POINT('Ctrl Pts',(0.262495421836479,-0.313540865983978,
-2.83380159067992));
#51402=CARTESIAN_POINT('Ctrl Pts',(0.406042522786106,0.0516335670323386,
-2.81393441373678));
#51403=CARTESIAN_POINT('Ctrl Pts',(0.176280206651099,0.368979900531617,
-2.79406723679364));
#51404=CARTESIAN_POINT('Ctrl Pts',(-0.21468104558796,0.348169574214524,
-2.7742000598505));
#51405=CARTESIAN_POINT('Ctrl Pts',(-0.409000969433003,0.00793399164957273,
-2.75433288290736));
#51406=CARTESIAN_POINT('Ctrl Pts',(-0.228101570126088,-0.339515198260848,
-2.73446570596422));
#51407=CARTESIAN_POINT('Ctrl Pts',(0.161923088730525,-0.375628974667497,
-2.71459852902108));
#51408=CARTESIAN_POINT('Ctrl Pts',(0.403483073400745,-0.0672377715951021,
-2.69473135207793));
#51409=CARTESIAN_POINT('Ctrl Pts',(0.27499230631357,0.302808021818952,-2.6748641751348));
#51410=CARTESIAN_POINT('Ctrl Pts',(-0.105683485795541,0.395154382089269,
-2.65499699819165));
#51411=CARTESIAN_POINT('Ctrl Pts',(-0.389442251006885,0.125103724088085,
-2.63512982124851));
#51412=CARTESIAN_POINT('Ctrl Pts',(-0.316042445719816,-0.259677815100926,
-2.61526264430537));
#51413=CARTESIAN_POINT('Ctrl Pts',(0.0471973530177957,-0.406310477432151,
-2.59539546736223));
#51414=CARTESIAN_POINT('Ctrl Pts',(0.367153335874026,-0.180316994118749,
-2.57552829041909));
#51415=CARTESIAN_POINT('Ctrl Pts',(0.350394021276791,0.211044340263396,
-2.55566111347595));
#51416=CARTESIAN_POINT('Ctrl Pts',(0.0122898678659977,0.408857804422968,
-2.5357939365328));
#51417=CARTESIAN_POINT('Ctrl Pts',(-0.337085376195796,0.231709276105699,
-2.51592675958967));
#51418=CARTESIAN_POINT('Ctrl Pts',(-0.37732084717748,-0.157938925514407,
-2.49605958264652));
#51419=CARTESIAN_POINT('Ctrl Pts',(-0.0715168261397497,-0.402741950499878,
-2.47619240570338));
#51420=CARTESIAN_POINT('Ctrl Pts',(0.29987501930772,-0.278191851792624,
-2.45632522876024));
#51421=CARTESIAN_POINT('Ctrl Pts',(0.396252613492476,0.101486936346117,
-2.4364580518171));
#51422=CARTESIAN_POINT('Ctrl Pts',(0.12922844125829,0.388092441652642,-2.41659087487395));
#51423=CARTESIAN_POINT('Ctrl Pts',(-0.256310646775627,0.318779838347793,
-2.39672369793082));
#51424=CARTESIAN_POINT('Ctrl Pts',(-0.406788210856558,-0.042884546204367,
-2.37685652098767));
#51425=CARTESIAN_POINT('Ctrl Pts',(-0.184201848786746,-0.365219676211651,
-2.35698934404454));
#51426=CARTESIAN_POINT('Ctrl Pts',(0.207315331081859,-0.352613224978964,
-2.33712216710139));
#51427=CARTESIAN_POINT('Ctrl Pts',(0.408704406261923,-0.016626521378421,
-2.31725499015826));
#51428=CARTESIAN_POINT('Ctrl Pts',(0.235272219274242,0.334608302012981,
-2.29738781321511));
#51429=CARTESIAN_POINT('Ctrl Pts',(-0.153927228514745,0.378975119566246,
-2.27752063627197));
#51430=CARTESIAN_POINT('Ctrl Pts',(-0.40196059830037,0.0757852910569974,
-2.25765345932882));
#51431=CARTESIAN_POINT('Ctrl Pts',(-0.281357426577698,-0.296906940706838,
-2.23778628238569));
#51432=CARTESIAN_POINT('Ctrl Pts',(0.0972775748947614,-0.397306942239017,
-2.21791910544254));
#51433=CARTESIAN_POINT('Ctrl Pts',(0.386699681049972,-0.133338252592638,
-2.19805192849941));
#51434=CARTESIAN_POINT('Ctrl Pts',(0.32148097506822,0.252914443237818,-2.17818475155626));
#51435=CARTESIAN_POINT('Ctrl Pts',(-0.038566714935569,0.40722026156361,
-2.15831757461312));
#51436=CARTESIAN_POINT('Ctrl Pts',(-0.363245016815483,0.188065921122305,
-2.13845039766998));
#51437=CARTESIAN_POINT('Ctrl Pts',(-0.354792690247869,-0.203562962926974,
-2.11858322072684));
#51438=CARTESIAN_POINT('Ctrl Pts',(-0.0209613318984479,-0.408505025053466,
-2.0987160437837));
#51439=CARTESIAN_POINT('Ctrl Pts',(0.332093584504505,-0.238808676684583,
-2.07884886684056));
#51440=CARTESIAN_POINT('Ctrl Pts',(0.380586732987488,0.149898204134711,
-2.05898168989742));
#51441=CARTESIAN_POINT('Ctrl Pts',(0.0800452308357175,0.401134009963445,
-2.03911451295428));
#51442=CARTESIAN_POINT('Ctrl Pts',(-0.293905449193615,0.284491335304253,
-2.01924733601113));
#51443=CARTESIAN_POINT('Ctrl Pts',(-0.398316555487175,-0.0930572649164465,
-1.99938015906799));
#51444=CARTESIAN_POINT('Ctrl Pts',(-0.137433058116583,-0.385263400111692,
-1.97951298212485));
#51445=CARTESIAN_POINT('Ctrl Pts',(0.249489776066525,-0.324145930974265,
-1.95964580518171));
#51446=CARTESIAN_POINT('Ctrl Pts',(0.407606482030808,0.0342445431472686,
-1.93977862823857));
#51447=CARTESIAN_POINT('Ctrl Pts',(0.191908827900848,0.361229476514057,
-1.91991145129543));
#51448=CARTESIAN_POINT('Ctrl Pts',(-0.199787685081339,0.356932225805877,
-1.90004427435229));
#51449=CARTESIAN_POINT('Ctrl Pts',(-0.408259669147063,0.025293783363276,
-1.88017709740914));
#51450=CARTESIAN_POINT('Ctrl Pts',(-0.242318257689397,-0.329541491954005,
-1.860309920466));
#51451=CARTESIAN_POINT('Ctrl Pts',(0.14585230965904,-0.382155513758496,
-1.84044274352286));
#51452=CARTESIAN_POINT('Ctrl Pts',(0.400262276509128,-0.0842961620278672,
-1.82057556657972));
#51453=CARTESIAN_POINT('Ctrl Pts',(0.287593226318909,0.290870880468256,
-1.80070838963658));
#51454=CARTESIAN_POINT('Ctrl Pts',(-0.0888264819281091,0.399281340707492,
-1.78084121269344));
#51455=CARTESIAN_POINT('Ctrl Pts',(-0.38378376019623,0.141512396412965,
-1.7609740357503));
#51456=CARTESIAN_POINT('Ctrl Pts',(-0.32677440629123,-0.246037030387525,
-1.74110685880716));
#51457=CARTESIAN_POINT('Ctrl Pts',(0.0299185173507721,-0.407946828947632,
-1.72123968186402));
#51458=CARTESIAN_POINT('Ctrl Pts',(0.359173282103036,-0.19573013654578,
-1.70137250492087));
#51459=CARTESIAN_POINT('Ctrl Pts',(0.359031590882975,0.195989922386171,
-1.68150532797773));
#51460=CARTESIAN_POINT('Ctrl Pts',(0.0296233881715808,0.407968366178229,
-1.66163815103459));
#51461=CARTESIAN_POINT('Ctrl Pts',(-0.326952311577669,0.245800567295756,
-1.64177097409145));
#51462=CARTESIAN_POINT('Ctrl Pts',(-0.383681285325876,-0.141790000421682,
-1.62190379714831));
#51463=CARTESIAN_POINT('Ctrl Pts',(-0.0885376062162486,-0.399345496048715,
-1.60203662020517));
#51464=CARTESIAN_POINT('Ctrl Pts',(0.28780357605159,-0.290662750521656,
-1.58216944326203));
#51465=CARTESIAN_POINT('Ctrl Pts',(0.400201189319881,0.0845857020769455,
-1.56230226631889));
#51466=CARTESIAN_POINT('Ctrl Pts',(0.145575808377645,0.382260927828221,
-1.54243508937574));
#51467=CARTESIAN_POINT('Ctrl Pts',(-0.242556594785546,0.329366105200487,
-1.5225679124326));
#51468=CARTESIAN_POINT('Ctrl Pts',(-0.408241264010235,-0.0255891244129948,
-1.50270073548946));
#51469=CARTESIAN_POINT('Ctrl Pts',(-0.199529416992774,-0.357076664994257,
-1.48283355854632));
#51470=CARTESIAN_POINT('Ctrl Pts',(0.192170102255799,-0.361090549208772,
-1.46296638160318));
#51471=CARTESIAN_POINT('Ctrl Pts',(0.407631148931293,-0.0339496590535454,
-1.44309920466004));
#51472=CARTESIAN_POINT('Ctrl Pts',(0.249255213591577,0.3243263347715,-1.4232320277169));
#51473=CARTESIAN_POINT('Ctrl Pts',(-0.137711733610034,0.385163875973612,
-1.40336485077376));
#51474=CARTESIAN_POINT('Ctrl Pts',(-0.398383771760093,0.092769086052951,
-1.38349767383061));
#51475=CARTESIAN_POINT('Ctrl Pts',(-0.293699562456816,-0.284703881149472,
-1.36363049688748));
#51476=CARTESIAN_POINT('Ctrl Pts',(0.0803354026361021,-0.401075997801155,
-1.34376331994433));
#51477=CARTESIAN_POINT('Ctrl Pts',(0.380695074392888,-0.149622836699118,
-1.32389614300119));
#51478=CARTESIAN_POINT('Ctrl Pts',(0.331920736022593,0.239048860961766,
-1.30402896605805));
#51479=CARTESIAN_POINT('Ctrl Pts',(-0.0212568515799336,0.408489754081796,
-1.28416178911491));
#51480=CARTESIAN_POINT('Ctrl Pts',(-0.354939861148809,0.203306241656672,
-1.26429461217177));
#51481=CARTESIAN_POINT('Ctrl Pts',(-0.363108869060434,-0.188328654586999,
-1.24442743522863));
#51482=CARTESIAN_POINT('Ctrl Pts',(-0.0382721091145412,-0.407248055357939,
-1.22456025828549));
#51483=CARTESIAN_POINT('Ctrl Pts',(0.321663857072701,-0.252681807778104,
-1.20469308134234));
#51484=CARTESIAN_POINT('Ctrl Pts',(0.386603118845436,0.133617968207419,
-1.1848259043992));
#51485=CARTESIAN_POINT('Ctrl Pts',(0.0969901253114878,0.397377211879292,
-1.16495872745606));
#51486=CARTESIAN_POINT('Ctrl Pts',(-0.281572144613101,0.296703320350273,
-1.14509155051292));
#51487=CARTESIAN_POINT('Ctrl Pts',(-0.401905667697113,-0.0760760619500936,
-1.12522437356978));
#51488=CARTESIAN_POINT('Ctrl Pts',(-0.153653025909756,-0.379086376117202,
-1.10535719662664));
#51489=CARTESIAN_POINT('Ctrl Pts',(0.235514223689601,-0.334438011249891,
-1.0854900196835));
#51490=CARTESIAN_POINT('Ctrl Pts',(0.408692271196321,0.0169221864216921,
-1.06562284274035));
#51491=CARTESIAN_POINT('Ctrl Pts',(0.207060185479571,0.35276311105055,-1.04575566579722));
#51492=CARTESIAN_POINT('Ctrl Pts',(-0.184466011710584,0.365086323288736,
-1.02588848885407));
#51493=CARTESIAN_POINT('Ctrl Pts',(-0.406819128572942,0.0425902518899552,
-1.00602131191093));
#51494=CARTESIAN_POINT('Ctrl Pts',(-0.25607996421368,-0.31896517812642,
-0.986154134967791));
#51495=CARTESIAN_POINT('Ctrl Pts',(0.129509164941429,-0.387998851963599,
-0.966286958024649));
#51496=CARTESIAN_POINT('Ctrl Pts',(0.396325929688306,-0.101200248940393,
-0.946419781081509));
#51497=CARTESIAN_POINT('Ctrl Pts',(0.299673686147936,0.278408718899761,
-0.926552604138367));
#51498=CARTESIAN_POINT('Ctrl Pts',(-0.0718081593809718,0.402690105633617,
-0.906685427195226));
#51499=CARTESIAN_POINT('Ctrl Pts',(-0.377435014050053,0.157665922437071,
-0.886818250252085));
#51500=CARTESIAN_POINT('Ctrl Pts',(-0.33691764757886,-0.231953080770283,
-0.866951073308944));
#51501=CARTESIAN_POINT('Ctrl Pts',(0.0125856167776199,-0.408848792561779,
-0.847083896365802));
#51502=CARTESIAN_POINT('Ctrl Pts',(0.350546659679034,-0.210790825978663,
-0.827216719422662));
#51503=CARTESIAN_POINT('Ctrl Pts',(0.367022689343624,0.18058260834276,-0.80734954247952));
#51504=CARTESIAN_POINT('Ctrl Pts',(0.0469036013999205,0.406344416849317,
-0.787482365536379));
#51505=CARTESIAN_POINT('Ctrl Pts',(-0.316230601652008,0.259449300457139,
-0.767615188593238));
#51506=CARTESIAN_POINT('Ctrl Pts',(-0.389350918247137,-0.125385786232088,
-0.747748011650096));
#51507=CARTESIAN_POINT('Ctrl Pts',(-0.105398983116618,-0.39523004350232,
-0.727880834706955));
#51508=CARTESIAN_POINT('Ctrl Pts',(0.275213960033025,-0.302610325553834,
-0.708013657763814));
#51509=CARTESIAN_POINT('Ctrl Pts',(0.403429223327349,0.0675321752544685,
-0.688146480820672));
#51510=CARTESIAN_POINT('Ctrl Pts',(0.161661074654281,0.375741174041693,
-0.668279303877532));
#51511=CARTESIAN_POINT('Ctrl Pts',(-0.228365832987187,0.339359365942348,
-0.64841212693439));
#51512=CARTESIAN_POINT('Ctrl Pts',(-0.408959300564399,-0.00824763070207162,
-0.628544949991249));
#51513=CARTESIAN_POINT('Ctrl Pts',(-0.214497743290479,-0.348290756480668,
-0.608677773048107));
#51514=CARTESIAN_POINT('Ctrl Pts',(0.176678881529869,-0.368917749301704,
-0.588810596104967));
#51515=CARTESIAN_POINT('Ctrl Pts',(0.405823973625002,-0.0512116721993414,
-0.568943419161826));
#51516=CARTESIAN_POINT('Ctrl Pts',(0.262789437287646,0.313460435399907,
-0.549076242218683));
#51517=CARTESIAN_POINT('Ctrl Pts',(-0.121248296095373,0.390659165546662,
-0.529209065275544));
#51518=CARTESIAN_POINT('Ctrl Pts',(-0.394089676741475,0.109585855266091,
-0.509341888332401));
#51519=CARTESIAN_POINT('Ctrl Pts',(-0.305512907904833,-0.271988227499954,
-0.48947471138926));
#51520=CARTESIAN_POINT('Ctrl Pts',(0.0632485904940357,-0.404122937715866,
-0.469607534446119));
#51521=CARTESIAN_POINT('Ctrl Pts',(0.374005047320018,-0.165638032701151,
-0.449740357502979));
#51522=CARTESIAN_POINT('Ctrl Pts',(0.341762890397528,0.224752883620358,
-0.429873180559837));
#51523=CARTESIAN_POINT('Ctrl Pts',(-0.00390871422013135,0.409023783613815,
-0.410006003616696));
#51524=CARTESIAN_POINT('Ctrl Pts',(-0.345995659532523,0.218180518603753,
-0.390138826673554));
#51525=CARTESIAN_POINT('Ctrl Pts',(-0.370771281864659,-0.172755267508155,
-0.370271649730414));
#51526=CARTESIAN_POINT('Ctrl Pts',(-0.0555139947999592,-0.405257863415184,
-0.350404472787271));
#51527=CARTESIAN_POINT('Ctrl Pts',(0.310655020540657,-0.266099987415665,
-0.330537295844131));
#51528=CARTESIAN_POINT('Ctrl Pts',(0.39192339032466,0.117097138394392,-0.310670118900989));
#51529=CARTESIAN_POINT('Ctrl Pts',(0.113760501983795,0.392904999458956,
-0.290802941957848));
#51530=CARTESIAN_POINT('Ctrl Pts',(-0.268732090740969,0.308381026668334,
-0.270935765014708));
#51531=CARTESIAN_POINT('Ctrl Pts',(-0.404770775527847,-0.0589577342741226,
-0.251068588071565));
#51532=CARTESIAN_POINT('Ctrl Pts',(-0.169597105673178,-0.372227122060309,
-0.231201411128425));
#51533=CARTESIAN_POINT('Ctrl Pts',(0.221116088077751,-0.344127389853583,
-0.211334234185283));
#51534=CARTESIAN_POINT('Ctrl Pts',(0.409039460479538,-0.000431717698386653,
-0.191467057242142));
#51535=CARTESIAN_POINT('Ctrl Pts',(0.221844048719085,0.343663682250411,
-0.171599880299001));
#51536=CARTESIAN_POINT('Ctrl Pts',(-0.168822377308669,0.372579143530119,
-0.151732703355859));
#51537=CARTESIAN_POINT('Ctrl Pts',(-0.404626678038961,0.0598176191706426,
-0.131865526412719));
#51538=CARTESIAN_POINT('Ctrl Pts',(-0.269417866660982,-0.307829099249045,
-0.111998349469577));
#51539=CARTESIAN_POINT('Ctrl Pts',(0.113004229631694,-0.393115819865864,
-0.0921311725264359));
#51540=CARTESIAN_POINT('Ctrl Pts',(0.391538855652792,-0.117975432897604,
-0.0722639955832951));
#51541=CARTESIAN_POINT('Ctrl Pts',(0.311481610440272,0.265548040686658,
-0.0523968186401534));
#51542=CARTESIAN_POINT('Ctrl Pts',(-0.0552111731989857,0.405170886763949,
-0.0325296416970127));
#51543=CARTESIAN_POINT('Ctrl Pts',(-0.264417563050825,0.251050518777684,
-0.0192848570682517));
#51544=CARTESIAN_POINT('Ctrl Pts',(-0.313273600006485,0.146768709331986,
-0.0126624647538713));
#51545=CARTESIAN_POINT('Ctrl Pts',(-0.0953060101009229,-0.307860260611276,
-2.84));
#51546=CARTESIAN_POINT('Ctrl Pts',(0.00717381913557572,-0.339585510310479,
-2.83337760768562));
#51547=CARTESIAN_POINT('Ctrl Pts',(0.244531614604281,-0.292083776802967,
-2.82013282305686));
#51548=CARTESIAN_POINT('Ctrl Pts',(0.378255106318521,0.0481000370439281,
-2.80026564611372));
#51549=CARTESIAN_POINT('Ctrl Pts',(0.164216515677071,0.34372885516354,-2.78039846917058));
#51550=CARTESIAN_POINT('Ctrl Pts',(-0.199989402997138,0.324342678219355,
-2.76053129222744));
#51551=CARTESIAN_POINT('Ctrl Pts',(-0.381011092423822,0.00739103095495322,
-2.74066411528429));
#51552=CARTESIAN_POINT('Ctrl Pts',(-0.212491497362003,-0.316280562276384,
-2.72079693834115));
#51553=CARTESIAN_POINT('Ctrl Pts',(0.150841923458968,-0.349922901607075,
-2.70092976139801));
#51554=CARTESIAN_POINT('Ctrl Pts',(0.375870812198945,-0.0626363718479885,
-2.68106258445487));
#51555=CARTESIAN_POINT('Ctrl Pts',(0.256173277980071,0.282085432090484,
-2.66119540751173));
#51556=CARTESIAN_POINT('Ctrl Pts',(-0.0984510634044162,0.368112092752765,
-2.64132823056859));
#51557=CARTESIAN_POINT('Ctrl Pts',(-0.36279086990387,0.11654228264341,-2.62146105362545));
#51558=CARTESIAN_POINT('Ctrl Pts',(-0.294414161567723,-0.24190683006692,
-2.60159387668231));
#51559=CARTESIAN_POINT('Ctrl Pts',(0.0439674142038161,-0.378504723556717,
-2.58172669973917));
#51560=CARTESIAN_POINT('Ctrl Pts',(0.342027290992345,-0.167977046624136,
-2.56185952279602));
#51561=CARTESIAN_POINT('Ctrl Pts',(0.32641489581436,0.196601574673756,-2.54199234585288));
#51562=CARTESIAN_POINT('Ctrl Pts',(0.0114488138936679,0.380877724874727,
-2.52212516890974));
#51563=CARTESIAN_POINT('Ctrl Pts',(-0.314017024464519,0.215852310903206,
-2.5022579919666));
#51564=CARTESIAN_POINT('Ctrl Pts',(-0.351498991253425,-0.147130415436207,
-2.48239081502346));
#51565=CARTESIAN_POINT('Ctrl Pts',(-0.066622590386437,-0.375180407854742,
-2.46252363808032));
#51566=CARTESIAN_POINT('Ctrl Pts',(0.279353148857915,-0.259153863380453,
-2.44265646113718));
#51567=CARTESIAN_POINT('Ctrl Pts',(0.369135166970047,0.0945417037460469,
-2.42278928419404));
#51568=CARTESIAN_POINT('Ctrl Pts',(0.120384725846265,0.361533434408456,
-2.40292210725089));
#51569=CARTESIAN_POINT('Ctrl Pts',(-0.238770093047016,0.296964221429498,
-2.38305493030775));
#51570=CARTESIAN_POINT('Ctrl Pts',(-0.378949763416092,-0.0399497532244903,
-2.36318775336461));
#51571=CARTESIAN_POINT('Ctrl Pts',(-0.171596042253934,-0.340225960835699,
-2.34332057642147));
#51572=CARTESIAN_POINT('Ctrl Pts',(0.193127759284308,-0.328482228877282,
-2.32345339947833));
#51573=CARTESIAN_POINT('Ctrl Pts',(0.380734824477702,-0.0154886896292257,
-2.30358622253519));
#51574=CARTESIAN_POINT('Ctrl Pts',(0.219171424964897,0.311709468221516,
-2.28371904559205));
#51575=CARTESIAN_POINT('Ctrl Pts',(-0.143393257897354,0.353040053933262,
-2.2638518686489));
#51576=CARTESIAN_POINT('Ctrl Pts',(-0.374452527293689,0.0705989439959352,
-2.24398469170576));
#51577=CARTESIAN_POINT('Ctrl Pts',(-0.262102802862633,-0.276588189958943,
-2.22411751476262));
#51578=CARTESIAN_POINT('Ctrl Pts',(0.090620408871829,-0.370117342997772,
-2.20425033781948));
#51579=CARTESIAN_POINT('Ctrl Pts',(0.360235987022344,-0.124213283290337,
-2.18438316087634));
#51580=CARTESIAN_POINT('Ctrl Pts',(0.299480506547509,0.235606307831963,
-2.1645159839332));
#51581=CARTESIAN_POINT('Ctrl Pts',(-0.0359274116371167,0.379352246843221,
-2.14464880699006));
#51582=CARTESIAN_POINT('Ctrl Pts',(-0.338386436751582,0.175195677784914,
-2.12478163004692));
#51583=CARTESIAN_POINT('Ctrl Pts',(-0.330512542996479,-0.189632183486893,
-2.10491445310378));
#51584=CARTESIAN_POINT('Ctrl Pts',(-0.0195268484971016,-0.380549087871386,
-2.08504727616063));
#51585=CARTESIAN_POINT('Ctrl Pts',(0.309366844764242,-0.222465865814493,
-2.06518009921749));
#51586=CARTESIAN_POINT('Ctrl Pts',(0.354541377001136,0.139639958772985,
-2.04531292227435));
#51587=CARTESIAN_POINT('Ctrl Pts',(0.0745673558825864,0.373682506318743,
-2.02544574533121));
#51588=CARTESIAN_POINT('Ctrl Pts',(-0.273792104751763,0.265022243344928,
-2.00557856838807));
#51589=CARTESIAN_POINT('Ctrl Pts',(-0.371057863620839,-0.0866889147303015,
-1.98571139144493));
#51590=CARTESIAN_POINT('Ctrl Pts',(-0.128027861842815,-0.358897997603687,
-1.96584421450179));
#51591=CARTESIAN_POINT('Ctrl Pts',(0.232416006884924,-0.301963086875939,
-1.94597703755865));
#51592=CARTESIAN_POINT('Ctrl Pts',(0.37971203641127,0.0319010265725857,
-1.9261098606155));
#51593=CARTESIAN_POINT('Ctrl Pts',(0.178775596218371,0.336508829436531,
-1.90624268367236));
#51594=CARTESIAN_POINT('Ctrl Pts',(-0.18611526581757,0.332505659984359,
-1.88637550672922));
#51595=CARTESIAN_POINT('Ctrl Pts',(-0.380320522833848,0.0235628097511194,
-1.86650832978608));
#51596=CARTESIAN_POINT('Ctrl Pts',(-0.225735269538518,-0.306989404016411,
-1.84664115284294));
#51597=CARTESIAN_POINT('Ctrl Pts',(0.13587094405367,-0.356002798660267,
-1.8267739758998));
#51598=CARTESIAN_POINT('Ctrl Pts',(0.372870429720997,-0.0785273756829916,
-1.80690679895666));
#51599=CARTESIAN_POINT('Ctrl Pts',(0.267911857239273,0.270965205963022,
-1.78703962201352));
#51600=CARTESIAN_POINT('Ctrl Pts',(-0.0827476642965211,0.371956624010715,
-1.76717244507038));
#51601=CARTESIAN_POINT('Ctrl Pts',(-0.357519616468391,0.131828031663501,
-1.74730526812723));
#51602=CARTESIAN_POINT('Ctrl Pts',(-0.304411683155098,-0.229199548975689,
-1.72743809118409));
#51603=CARTESIAN_POINT('Ctrl Pts',(0.0278710512479263,-0.380029091773661,
-1.70757091424095));
#51604=CARTESIAN_POINT('Ctrl Pts',(0.334593350165504,-0.182335394580983,
-1.68770373729781));
#51605=CARTESIAN_POINT('Ctrl Pts',(0.334461355547943,0.182577402043658,
-1.66783656035467));
#51606=CARTESIAN_POINT('Ctrl Pts',(0.0275961191588265,0.380049155109377,
-1.64796938341153));
#51607=CARTESIAN_POINT('Ctrl Pts',(-0.304577413538642,0.228979268175285,
-1.62810220646839));
#51608=CARTESIAN_POINT('Ctrl Pts',(-0.357424154439649,-0.132086637912698,
-1.60823502952524));
#51609=CARTESIAN_POINT('Ctrl Pts',(-0.0824785577203104,-0.372016388897528,
-1.5883678525821));
#51610=CARTESIAN_POINT('Ctrl Pts',(0.268107811741657,-0.270771319336224,
-1.56850067563896));
#51611=CARTESIAN_POINT('Ctrl Pts',(0.372813523017964,0.0787971011326718,
-1.54863349869582));
#51612=CARTESIAN_POINT('Ctrl Pts',(0.135613365066933,0.35610099874502,-1.52876632175268));
#51613=CARTESIAN_POINT('Ctrl Pts',(-0.225957296096291,0.306826019810628,
-1.50889914480954));
#51614=CARTESIAN_POINT('Ctrl Pts',(-0.380303377247864,-0.023837939211441,
-1.4890319678664));
#51615=CARTESIAN_POINT('Ctrl Pts',(-0.185874672239764,-0.332640214513727,
-1.46916479092326));
#51616=CARTESIAN_POINT('Ctrl Pts',(0.179018990329492,-0.336379409585943,
-1.44929761398012));
#51617=CARTESIAN_POINT('Ctrl Pts',(0.379735015238712,-0.0316263227965929,
-1.42943043703697));
#51618=CARTESIAN_POINT('Ctrl Pts',(0.232197496633113,0.302131144785331,
-1.40956326009383));
#51619=CARTESIAN_POINT('Ctrl Pts',(-0.128287466249961,0.358805284374608,
-1.38969608315069));
#51620=CARTESIAN_POINT('Ctrl Pts',(-0.371120479965266,0.0864204573138163,
-1.36982890620755));
#51621=CARTESIAN_POINT('Ctrl Pts',(-0.273600307821276,-0.26522024366945,
-1.34996172926441));
#51622=CARTESIAN_POINT('Ctrl Pts',(0.0748376698498334,-0.373628464203982,
-1.33009455232127));
#51623=CARTESIAN_POINT('Ctrl Pts',(0.354642304090093,-0.139383436037601,
-1.31022737537813));
#51624=CARTESIAN_POINT('Ctrl Pts',(0.309205825124097,0.222689613141937,
-1.29036019843499));
#51625=CARTESIAN_POINT('Ctrl Pts',(-0.0198021443645707,0.380534861964767,
-1.27049302149184));
#51626=CARTESIAN_POINT('Ctrl Pts',(-0.330649642294355,0.189393030871235,
-1.2506258445487));
#51627=CARTESIAN_POINT('Ctrl Pts',(-0.33825960623342,-0.175440431151973,
-1.23075866760556));
#51628=CARTESIAN_POINT('Ctrl Pts',(-0.0356529670902981,-0.379378138576325,
-1.21089149066242));
#51629=CARTESIAN_POINT('Ctrl Pts',(0.299650873068665,-0.235389592720591,
-1.19102431371928));
#51630=CARTESIAN_POINT('Ctrl Pts',(0.360146033027642,0.124473856638375,
-1.17115713677614));
#51631=CARTESIAN_POINT('Ctrl Pts',(0.0903526308274595,0.37018280375314,
-1.151289959833));
#51632=CARTESIAN_POINT('Ctrl Pts',(-0.262302826724056,0.276398504309537,
-1.13142278288985));
#51633=CARTESIAN_POINT('Ctrl Pts',(-0.374401355852254,-0.0708698160571368,
-1.11155560594672));
#51634=CARTESIAN_POINT('Ctrl Pts',(-0.14313782027769,-0.353143696670534,
-1.09168842900357));
#51635=CARTESIAN_POINT('Ctrl Pts',(0.219396867869826,-0.311550831263358,
-1.07182125206043));
#51636=CARTESIAN_POINT('Ctrl Pts',(0.380723519872219,0.0157641209106834,
-1.05195407511729));
#51637=CARTESIAN_POINT('Ctrl Pts',(0.192890074506225,0.328621857533794,
-1.03208689817415));
#51638=CARTESIAN_POINT('Ctrl Pts',(-0.171842127255466,0.340101733886045,
-1.01221972123101));
#51639=CARTESIAN_POINT('Ctrl Pts',(-0.378978565286443,0.039675598866412,
-0.992352544287869));
#51640=CARTESIAN_POINT('Ctrl Pts',(-0.238555197187349,-0.297136877527654,
-0.972485367344726));
#51641=CARTESIAN_POINT('Ctrl Pts',(0.12064623827576,-0.361446249505908,
-0.952618190401585));
#51642=CARTESIAN_POINT('Ctrl Pts',(0.369203465790718,-0.0942746357198006,
-0.932751013458444));
#51643=CARTESIAN_POINT('Ctrl Pts',(0.279165593881561,0.259355889242436,
-0.912883836515302));
#51644=CARTESIAN_POINT('Ctrl Pts',(-0.0668939863116134,0.375132110978679,
-0.893016659572163));
#51645=CARTESIAN_POINT('Ctrl Pts',(-0.351605345145198,0.146876095254826,
-0.873149482629021));
#51646=CARTESIAN_POINT('Ctrl Pts',(-0.313860774312695,-0.216079430857763,
-0.85328230568588));
#51647=CARTESIAN_POINT('Ctrl Pts',(0.0117243233039672,-0.38086932973796,
-0.833415128742737));
#51648=CARTESIAN_POINT('Ctrl Pts',(0.326557088446483,-0.196365409574429,
-0.813547951799597));
#51649=CARTESIAN_POINT('Ctrl Pts',(0.341905585223924,0.168224483606484,
-0.793680774856455));
#51650=CARTESIAN_POINT('Ctrl Pts',(0.0436937654029756,0.378536340338528,
-0.773813597913315));
#51651=CARTESIAN_POINT('Ctrl Pts',(-0.294589441096693,0.241693953764487,
-0.753946420970174));
#51652=CARTESIAN_POINT('Ctrl Pts',(-0.362705787478237,-0.11680504193654,
-0.734079244027031));
#51653=CARTESIAN_POINT('Ctrl Pts',(-0.098186030593751,-0.368182576296315,
-0.714212067083892));
#51654=CARTESIAN_POINT('Ctrl Pts',(0.256379762883779,-0.281901265118838,
-0.694344890140749));
#51655=CARTESIAN_POINT('Ctrl Pts',(0.375820647341585,0.0629106280680267,
-0.674477713197609));
#51656=CARTESIAN_POINT('Ctrl Pts',(0.150597840249194,0.35002742264572,-0.654610536254467));
#51657=CARTESIAN_POINT('Ctrl Pts',(-0.212737675461616,0.316135394302848,
-0.634743359311326));
#51658=CARTESIAN_POINT('Ctrl Pts',(-0.38097227515361,-0.00768320619890207,
-0.614876182368184));
#51659=CARTESIAN_POINT('Ctrl Pts',(-0.199818644945625,-0.324455567408028,
-0.595009005425044));
#51660=CARTESIAN_POINT('Ctrl Pts',(0.164587907342214,-0.343670957237192,
-0.575141828481902));
#51661=CARTESIAN_POINT('Ctrl Pts',(0.378051513513506,-0.0477070144762039,
-0.555274651538762));
#51662=CARTESIAN_POINT('Ctrl Pts',(0.24480550918305,0.2920088504654,-0.535407474595619));
#51663=CARTESIAN_POINT('Ctrl Pts',(-0.112950699881881,0.363924505207545,
-0.515540297652479));
#51664=CARTESIAN_POINT('Ctrl Pts',(-0.367120250243846,0.102086375215724,
-0.495673120709337));
#51665=CARTESIAN_POINT('Ctrl Pts',(-0.284605209987079,-0.253374782533741,
-0.475805943766196));
#51666=CARTESIAN_POINT('Ctrl Pts',(0.0589201893379548,-0.376466887562887,
-0.455938766823054));
#51667=CARTESIAN_POINT('Ctrl Pts',(0.348410107313365,-0.154302636186626,
-0.436071589879914));
#51668=CARTESIAN_POINT('Ctrl Pts',(0.318374434175064,0.20937197736306,-0.416204412936773));
#51669=CARTESIAN_POINT('Ctrl Pts',(-0.0036412223595689,0.38103234532199,
-0.396337235993631));
#51670=CARTESIAN_POINT('Ctrl Pts',(-0.322317534834062,0.203249390469792,
-0.37647005905049));
#51671=CARTESIAN_POINT('Ctrl Pts',(-0.345397643772028,-0.160932804845182,
-0.356602882107349));
#51672=CARTESIAN_POINT('Ctrl Pts',(-0.0517149087271477,-0.377524144911485,
-0.336735705164208));
#51673=CARTESIAN_POINT('Ctrl Pts',(0.289395423456396,-0.247889502657562,
-0.316868528221066));
#51674=CARTESIAN_POINT('Ctrl Pts',(0.365102213085359,0.109083625599228,
-0.297001351277925));
#51675=CARTESIAN_POINT('Ctrl Pts',(0.105975331050231,0.366016646048953,
-0.277134174334784));
#51676=CARTESIAN_POINT('Ctrl Pts',(-0.250341478663234,0.287277049774642,
-0.257266997391643));
#51677=CARTESIAN_POINT('Ctrl Pts',(-0.377070390759466,-0.0549229767688766,
-0.237399820448501));
#51678=CARTESIAN_POINT('Ctrl Pts',(-0.157990771009751,-0.346753853915265,
-0.21753264350536));
#51679=CARTESIAN_POINT('Ctrl Pts',(0.205984064995685,-0.320577119714015,
-0.197665466562219));
#51680=CARTESIAN_POINT('Ctrl Pts',(0.381046949345406,-0.000402173207826333,
-0.177798289619077));
#51681=CARTESIAN_POINT('Ctrl Pts',(0.206662207836228,0.320145145822377,
-0.157931112675937));
#51682=CARTESIAN_POINT('Ctrl Pts',(-0.157269060983239,0.347081784885588,
-0.138063935732795));
#51683=CARTESIAN_POINT('Ctrl Pts',(-0.376936154545472,0.0557240156618553,
-0.118196758789654));
#51684=CARTESIAN_POINT('Ctrl Pts',(-0.250980323683099,-0.286762893367498,
-0.0983295818465129));
#51685=CARTESIAN_POINT('Ctrl Pts',(0.105270814003626,-0.366213039015092,
-0.0784624049033714));
#51686=CARTESIAN_POINT('Ctrl Pts',(0.364743993945667,-0.10990181424216,
-0.0585952279602307));
#51687=CARTESIAN_POINT('Ctrl Pts',(0.290165445887089,0.247375328262155,
-0.038728051017089));
#51688=CARTESIAN_POINT('Ctrl Pts',(-0.0514328106451888,0.377443120485191,
-0.0188608740739483));
#51689=CARTESIAN_POINT('Ctrl Pts',(-0.246322214574953,0.233869940566782,
-0.00561608944518735));
#51690=CARTESIAN_POINT('Ctrl Pts',(-0.291834801104466,0.136724630148766,
0.00100630286919312));
#51691=CARTESIAN_POINT('Origin',(0.,0.,-2.22));
#51692=CARTESIAN_POINT('Origin',(0.,0.,-0.04));
#51693=CARTESIAN_POINT('Origin',(0.,0.,-0.04));
#51694=CARTESIAN_POINT('',(-0.4333,5.30639458070548E-17,0.));
#51695=CARTESIAN_POINT('Origin',(-0.4333,-5.30639458070548E-17,-0.04));
#51696=CARTESIAN_POINT('Origin',(0.,0.,0.));
#51697=CARTESIAN_POINT('Origin',(0.61,0.,0.));
#51698=CARTESIAN_POINT('',(-0.61,-7.47034547479885E-17,1.04083408558608E-17));
#51699=CARTESIAN_POINT('Origin',(0.,0.,0.));
#51700=CARTESIAN_POINT('Origin',(0.,0.,0.31));
#51701=CARTESIAN_POINT('',(0.,0.,0.22));
#51702=CARTESIAN_POINT('',(-0.29999119987093,-3.67383262694308E-17,0.4));
#51703=CARTESIAN_POINT('',(-0.149995599935465,-1.83691631347154E-17,0.31));
#51704=CARTESIAN_POINT('Origin',(0.,0.,0.4));
#51705=CARTESIAN_POINT('Origin',(0.173205080756888,0.3,0.8));
#51706=CARTESIAN_POINT('',(0.173205080756888,0.3,0.8));
#51707=CARTESIAN_POINT('',(0.346410161513775,0.,0.8));
#51708=CARTESIAN_POINT('',(0.21650635094611,0.225,0.8));
#51709=CARTESIAN_POINT('',(0.173205080756888,0.3,0.4));
#51710=CARTESIAN_POINT('',(0.173205080756888,0.3,0.8));
#51711=CARTESIAN_POINT('',(0.346410161513775,0.,0.4));
#51712=CARTESIAN_POINT('',(0.346410161513775,0.,0.4));
#51713=CARTESIAN_POINT('',(0.346410161513775,0.,0.8));
#51714=CARTESIAN_POINT('Origin',(-0.173205080756888,0.3,0.8));
#51715=CARTESIAN_POINT('',(-0.173205080756888,0.3,0.8));
#51716=CARTESIAN_POINT('',(-0.0866025403784438,0.3,0.8));
#51717=CARTESIAN_POINT('',(-0.173205080756888,0.3,0.4));
#51718=CARTESIAN_POINT('',(-0.173205080756888,0.3,0.8));
#51719=CARTESIAN_POINT('',(0.173205080756888,0.3,0.4));
#51720=CARTESIAN_POINT('Origin',(-0.346410161513775,5.55111512312578E-17,
0.8));
#51721=CARTESIAN_POINT('',(-0.346410161513775,4.24230095489963E-17,0.8));
#51722=CARTESIAN_POINT('',(-0.303108891324554,0.0750000000000001,0.8));
#51723=CARTESIAN_POINT('',(-0.346410161513775,5.55111512312578E-17,0.4));
#51724=CARTESIAN_POINT('',(-0.346410161513775,4.24230095489963E-17,0.8));
#51725=CARTESIAN_POINT('',(-0.173205080756888,0.3,0.4));
#51726=CARTESIAN_POINT('Origin',(-0.173205080756888,-0.3,0.8));
#51727=CARTESIAN_POINT('',(-0.173205080756888,-0.3,0.8));
#51728=CARTESIAN_POINT('',(-0.21650635094611,-0.225,0.8));
#51729=CARTESIAN_POINT('',(-0.173205080756888,-0.3,0.4));
#51730=CARTESIAN_POINT('',(-0.173205080756888,-0.3,0.8));
#51731=CARTESIAN_POINT('',(-0.346410161513775,4.24230095489963E-17,0.4));
#51732=CARTESIAN_POINT('Origin',(0.173205080756888,-0.3,0.8));
#51733=CARTESIAN_POINT('',(0.173205080756888,-0.3,0.8));
#51734=CARTESIAN_POINT('',(0.0866025403784439,-0.3,0.8));
#51735=CARTESIAN_POINT('',(0.173205080756888,-0.3,0.4));
#51736=CARTESIAN_POINT('',(0.173205080756888,-0.3,0.8));
#51737=CARTESIAN_POINT('',(-0.173205080756888,-0.3,0.4));
#51738=CARTESIAN_POINT('Origin',(0.346410161513775,0.,0.8));
#51739=CARTESIAN_POINT('',(0.303108891324554,-0.075,0.8));
#51740=CARTESIAN_POINT('',(0.173205080756888,-0.3,0.4));
#51741=CARTESIAN_POINT('Origin',(0.,5.55111512312578E-17,0.4));
#51742=CARTESIAN_POINT('Origin',(0.635148348882184,-0.269604478657599,0.74));
#51743=CARTESIAN_POINT('',(0.605292169324788,-0.236899535149592,0.14));
#51744=CARTESIAN_POINT('',(0.605292169324788,-0.236899535149592,0.74));
#51745=CARTESIAN_POINT('',(0.605292169324788,-0.236899535149592,0.39));
#51746=CARTESIAN_POINT('',(0.582609424887263,-0.212052488861915,0.14));
#51747=CARTESIAN_POINT('',(0.635148348882184,-0.269604478657599,0.14));
#51748=CARTESIAN_POINT('',(0.582609424887263,-0.212052488861915,0.74));
#51749=CARTESIAN_POINT('',(0.582609424887263,-0.212052488861915,0.74));
#51750=CARTESIAN_POINT('',(0.635148348882184,-0.269604478657599,0.74));
#51751=CARTESIAN_POINT('Origin',(0.621229853250879,-0.235670477458144,0.74));
#51752=CARTESIAN_POINT('',(0.615956788709343,-0.207598734203447,0.74));
#51753=CARTESIAN_POINT('Origin',(0.,0.,0.74));
#51754=CARTESIAN_POINT('',(0.582609424887263,-0.212052488861915,0.74));
#51755=CARTESIAN_POINT('Origin',(0.582609424887263,-0.212052488861915,0.74));
#51756=CARTESIAN_POINT('',(0.615956788709343,-0.207598734203447,0.14));
#51757=CARTESIAN_POINT('',(0.615956788709343,-0.207598734203447,0.39));
#51758=CARTESIAN_POINT('',(0.582609424887263,-0.212052488861915,0.14));
#51759=CARTESIAN_POINT('Origin',(0.621229853250879,-0.235670477458144,0.14));
#51760=CARTESIAN_POINT('Origin',(0.,0.,0.14));
#51761=CARTESIAN_POINT('Origin',(0.504634054117228,-0.470578868443124,0.74));
#51762=CARTESIAN_POINT('',(0.48776417196835,-0.429634859554052,0.14));
#51763=CARTESIAN_POINT('',(0.48776417196835,-0.429634859554052,0.74));
#51764=CARTESIAN_POINT('',(0.48776417196835,-0.429634859554052,0.39));
#51765=CARTESIAN_POINT('',(0.474947554733766,-0.398528318005655,0.14));
#51766=CARTESIAN_POINT('',(0.504634054117228,-0.470578868443124,0.14));
#51767=CARTESIAN_POINT('',(0.474947554733766,-0.398528318005655,0.74));
#51768=CARTESIAN_POINT('',(0.474947554733766,-0.398528318005655,0.74));
#51769=CARTESIAN_POINT('',(0.504634054117228,-0.470578868443124,0.74));
#51770=CARTESIAN_POINT('Origin',(0.513003028333199,-0.434553593224389,0.74));
#51771=CARTESIAN_POINT('',(0.507807100246665,-0.405748627772263,0.74));
#51772=CARTESIAN_POINT('Origin',(0.,0.,0.74));
#51773=CARTESIAN_POINT('',(0.474947554733766,-0.398528318005655,0.74));
#51774=CARTESIAN_POINT('Origin',(0.474947554733766,-0.398528318005655,0.74));
#51775=CARTESIAN_POINT('',(0.507807100246665,-0.405748627772263,0.14));
#51776=CARTESIAN_POINT('',(0.507807100246665,-0.405748627772263,0.39));
#51777=CARTESIAN_POINT('',(0.474947554733766,-0.398528318005655,0.14));
#51778=CARTESIAN_POINT('Origin',(0.513003028333199,-0.434553593224389,0.14));
#51779=CARTESIAN_POINT('Origin',(0.,0.,0.14));
#51780=CARTESIAN_POINT('Origin',(0.313253444820287,-0.614794501689974,0.74));
#51781=CARTESIAN_POINT('',(0.311404616840027,-0.570549879161074,0.14));
#51782=CARTESIAN_POINT('',(0.311404616840027,-0.570549879161074,0.74));
#51783=CARTESIAN_POINT('',(0.311404616840027,-0.570549879161074,0.39));
#51784=CARTESIAN_POINT('',(0.31,-0.536935750346352,0.14));
#51785=CARTESIAN_POINT('',(0.313253444820287,-0.614794501689974,0.14));
#51786=CARTESIAN_POINT('',(0.31,-0.536935750346352,0.74));
#51787=CARTESIAN_POINT('',(0.31,-0.536935750346352,0.74));
#51788=CARTESIAN_POINT('',(0.313253444820287,-0.614794501689974,0.74));
#51789=CARTESIAN_POINT('Origin',(0.342900467080184,-0.575865126018163,0.74));
#51790=CARTESIAN_POINT('',(0.338408381059618,-0.55495924861976,0.74));
#51791=CARTESIAN_POINT('Origin',(0.,0.,0.74));
#51792=CARTESIAN_POINT('',(0.31,-0.536935750346352,0.74));
#51793=CARTESIAN_POINT('Origin',(0.31,-0.536935750346352,0.74));
#51794=CARTESIAN_POINT('',(0.338408381059618,-0.55495924861976,0.14));
#51795=CARTESIAN_POINT('',(0.338408381059618,-0.55495924861976,0.39));
#51796=CARTESIAN_POINT('',(0.31,-0.536935750346352,0.14));
#51797=CARTESIAN_POINT('Origin',(0.342900467080184,-0.575865126018163,0.14));
#51798=CARTESIAN_POINT('Origin',(0.,0.,0.14));
#51799=CARTESIAN_POINT('Origin',(0.0840898469495519,-0.684856844632512,
0.74));
#51800=CARTESIAN_POINT('',(0.097485069078123,-0.642648162921854,0.14));
#51801=CARTESIAN_POINT('',(0.097485069078123,-0.642648162921854,0.74));
#51802=CARTESIAN_POINT('',(0.097485069078123,-0.642648162921854,0.39));
#51803=CARTESIAN_POINT('',(0.107661870153497,-0.610580806867569,0.14));
#51804=CARTESIAN_POINT('',(0.0840898469495519,-0.684856844632512,0.14));
#51805=CARTESIAN_POINT('',(0.107661870153497,-0.610580806867569,0.74));
#51806=CARTESIAN_POINT('',(0.107661870153497,-0.610580806867569,0.74));
#51807=CARTESIAN_POINT('',(0.0840898469495519,-0.684856844632512,0.74));
#51808=CARTESIAN_POINT('Origin',(0.119653037223409,-0.647718825750041,0.74));
#51809=CARTESIAN_POINT('',(0.128192616740993,-0.637233593757499,0.74));
#51810=CARTESIAN_POINT('Origin',(0.,0.,0.74));
#51811=CARTESIAN_POINT('',(0.107661870153497,-0.610580806867569,0.74));
#51812=CARTESIAN_POINT('Origin',(0.107661870153497,-0.610580806867569,0.74));
#51813=CARTESIAN_POINT('',(0.128192616740993,-0.637233593757499,0.14));
#51814=CARTESIAN_POINT('',(0.128192616740993,-0.637233593757499,0.39));
#51815=CARTESIAN_POINT('',(0.107661870153497,-0.610580806867569,0.14));
#51816=CARTESIAN_POINT('Origin',(0.119653037223409,-0.647718825750041,0.14));
#51817=CARTESIAN_POINT('Origin',(0.,0.,0.14));
#51818=CARTESIAN_POINT('Origin',(-0.155216227497267,-0.672315344701812,
0.74));
#51819=CARTESIAN_POINT('',(-0.128192616740993,-0.637233593757499,0.14));
#51820=CARTESIAN_POINT('',(-0.128192616740993,-0.637233593757499,0.74));
#51821=CARTESIAN_POINT('',(-0.128192616740993,-0.637233593757499,0.39));
#51822=CARTESIAN_POINT('',(-0.107661870153497,-0.610580806867569,0.14));
#51823=CARTESIAN_POINT('',(-0.155216227497267,-0.672315344701812,0.14));
#51824=CARTESIAN_POINT('',(-0.107661870153497,-0.610580806867569,0.74));
#51825=CARTESIAN_POINT('',(-0.107661870153497,-0.610580806867569,0.74));
#51826=CARTESIAN_POINT('',(-0.155216227497267,-0.672315344701812,0.74));
#51827=CARTESIAN_POINT('Origin',(-0.119653037223409,-0.647718825750041,
0.74));
#51828=CARTESIAN_POINT('',(-0.097485069078123,-0.642648162921854,0.74));
#51829=CARTESIAN_POINT('Origin',(0.,0.,0.74));
#51830=CARTESIAN_POINT('',(-0.107661870153497,-0.610580806867569,0.74));
#51831=CARTESIAN_POINT('Origin',(-0.107661870153497,-0.610580806867569,
0.74));
#51832=CARTESIAN_POINT('',(-0.097485069078123,-0.642648162921854,0.14));
#51833=CARTESIAN_POINT('',(-0.097485069078123,-0.642648162921854,0.39));
#51834=CARTESIAN_POINT('',(-0.107661870153497,-0.610580806867569,0.14));
#51835=CARTESIAN_POINT('Origin',(-0.119653037223409,-0.647718825750041,
0.14));
#51836=CARTESIAN_POINT('Origin',(0.,0.,0.14));
#51837=CARTESIAN_POINT('Origin',(-0.375800934160369,-0.578682691882343,
0.74));
#51838=CARTESIAN_POINT('',(-0.338408381059618,-0.55495924861976,0.14));
#51839=CARTESIAN_POINT('',(-0.338408381059618,-0.55495924861976,0.74));
#51840=CARTESIAN_POINT('',(-0.338408381059618,-0.55495924861976,0.39));
#51841=CARTESIAN_POINT('',(-0.31,-0.536935750346352,0.14));
#51842=CARTESIAN_POINT('',(-0.375800934160369,-0.578682691882343,0.14));
#51843=CARTESIAN_POINT('',(-0.31,-0.536935750346352,0.74));
#51844=CARTESIAN_POINT('',(-0.31,-0.536935750346352,0.74));
#51845=CARTESIAN_POINT('',(-0.375800934160369,-0.578682691882343,0.74));
#51846=CARTESIAN_POINT('Origin',(-0.342900467080184,-0.575865126018163,
0.74));
#51847=CARTESIAN_POINT('',(-0.311404616840027,-0.570549879161074,0.74));
#51848=CARTESIAN_POINT('Origin',(0.,0.,0.74));
#51849=CARTESIAN_POINT('',(-0.31,-0.536935750346352,0.74));
#51850=CARTESIAN_POINT('Origin',(-0.31,-0.536935750346352,0.74));
#51851=CARTESIAN_POINT('',(-0.311404616840027,-0.570549879161074,0.14));
#51852=CARTESIAN_POINT('',(-0.311404616840027,-0.570549879161074,0.39));
#51853=CARTESIAN_POINT('',(-0.31,-0.536935750346352,0.14));
#51854=CARTESIAN_POINT('Origin',(-0.342900467080184,-0.575865126018163,
0.14));
#51855=CARTESIAN_POINT('Origin',(0.,0.,0.14));
#51856=CARTESIAN_POINT('Origin',(-0.551058501932632,-0.415252365974913,
0.74));
#51857=CARTESIAN_POINT('',(-0.507807100246665,-0.405748627772262,0.14));
#51858=CARTESIAN_POINT('',(-0.507807100246665,-0.405748627772262,0.74));
#51859=CARTESIAN_POINT('',(-0.507807100246665,-0.405748627772262,0.39));
#51860=CARTESIAN_POINT('',(-0.474947554733766,-0.398528318005654,0.14));
#51861=CARTESIAN_POINT('',(-0.551058501932632,-0.415252365974913,0.14));
#51862=CARTESIAN_POINT('',(-0.474947554733766,-0.398528318005654,0.74));
#51863=CARTESIAN_POINT('',(-0.474947554733766,-0.398528318005654,0.74));
#51864=CARTESIAN_POINT('',(-0.551058501932632,-0.415252365974913,0.74));
#51865=CARTESIAN_POINT('Origin',(-0.513003028333199,-0.434553593224389,
0.74));
#51866=CARTESIAN_POINT('',(-0.48776417196835,-0.429634859554052,0.74));
#51867=CARTESIAN_POINT('Origin',(0.,0.,0.74));
#51868=CARTESIAN_POINT('',(-0.474947554733766,-0.398528318005654,0.74));
#51869=CARTESIAN_POINT('Origin',(-0.474947554733766,-0.398528318005654,
0.74));
#51870=CARTESIAN_POINT('',(-0.48776417196835,-0.429634859554052,0.14));
#51871=CARTESIAN_POINT('',(-0.48776417196835,-0.429634859554052,0.39));
#51872=CARTESIAN_POINT('',(-0.474947554733766,-0.398528318005654,0.14));
#51873=CARTESIAN_POINT('Origin',(-0.513003028333199,-0.434553593224389,
0.14));
#51874=CARTESIAN_POINT('Origin',(0.,0.,0.14));
#51875=CARTESIAN_POINT('Origin',(-0.659850281614495,-0.201736476258688,
0.74));
#51876=CARTESIAN_POINT('',(-0.615956788709343,-0.207598734203447,0.14));
#51877=CARTESIAN_POINT('',(-0.615956788709343,-0.207598734203447,0.74));
#51878=CARTESIAN_POINT('',(-0.615956788709343,-0.207598734203447,0.39));
#51879=CARTESIAN_POINT('',(-0.582609424887263,-0.212052488861915,0.14));
#51880=CARTESIAN_POINT('',(-0.659850281614495,-0.201736476258688,0.14));
#51881=CARTESIAN_POINT('',(-0.582609424887263,-0.212052488861915,0.74));
#51882=CARTESIAN_POINT('',(-0.582609424887263,-0.212052488861915,0.74));
#51883=CARTESIAN_POINT('',(-0.659850281614495,-0.201736476258688,0.74));
#51884=CARTESIAN_POINT('Origin',(-0.621229853250879,-0.235670477458144,
0.74));
#51885=CARTESIAN_POINT('',(-0.605292169324788,-0.236899535149591,0.74));
#51886=CARTESIAN_POINT('Origin',(0.,0.,0.74));
#51887=CARTESIAN_POINT('',(-0.582609424887263,-0.212052488861915,0.74));
#51888=CARTESIAN_POINT('Origin',(-0.582609424887263,-0.212052488861915,
0.74));
#51889=CARTESIAN_POINT('',(-0.605292169324788,-0.236899535149591,0.14));
#51890=CARTESIAN_POINT('',(-0.605292169324788,-0.236899535149591,0.39));
#51891=CARTESIAN_POINT('',(-0.582609424887263,-0.212052488861915,0.14));
#51892=CARTESIAN_POINT('Origin',(-0.621229853250879,-0.235670477458144,
0.14));
#51893=CARTESIAN_POINT('Origin',(0.,0.,0.14));
#51894=CARTESIAN_POINT('Origin',(-0.689054378980656,0.0361118098076312,
0.74));
#51895=CARTESIAN_POINT('',(-0.649812997899645,0.0155906305413142,0.14));
#51896=CARTESIAN_POINT('',(-0.649812997899645,0.0155906305413142,0.74));
#51897=CARTESIAN_POINT('',(-0.649812997899645,0.0155906305413142,0.39));
#51898=CARTESIAN_POINT('',(-0.62,7.59281015471359E-17,0.14));
#51899=CARTESIAN_POINT('',(-0.689054378980656,0.0361118098076312,0.14));
#51900=CARTESIAN_POINT('',(-0.62,7.59281015471359E-17,0.74));
#51901=CARTESIAN_POINT('',(-0.62,7.59281015471359E-17,0.74));
#51902=CARTESIAN_POINT('',(-0.689054378980656,0.0361118098076312,0.74));
#51903=CARTESIAN_POINT('Origin',(-0.654527189490328,8.32667268468867E-17,
0.74));
#51904=CARTESIAN_POINT('',(-0.65,-7.9602041944578E-17,0.74));
#51905=CARTESIAN_POINT('Origin',(0.,0.,0.74));
#51906=CARTESIAN_POINT('',(-0.649812997899645,-0.015590630541314,0.74));
#51907=CARTESIAN_POINT('',(-0.62,7.59281015471359E-17,0.74));
#51908=CARTESIAN_POINT('Origin',(0.,0.,0.74));
#51909=CARTESIAN_POINT('Origin',(-0.62,7.59281015471359E-17,0.74));
#51910=CARTESIAN_POINT('',(-0.649812997899645,-0.015590630541314,0.14));
#51911=CARTESIAN_POINT('',(-0.649812997899645,-0.015590630541314,0.39));
#51912=CARTESIAN_POINT('',(-0.62,7.59281015471359E-17,0.14));
#51913=CARTESIAN_POINT('Origin',(-0.654527189490328,8.32667268468867E-17,
0.14));
#51914=CARTESIAN_POINT('',(-0.65,-7.9602041944578E-17,0.14));
#51915=CARTESIAN_POINT('Origin',(0.,0.,0.14));
#51916=CARTESIAN_POINT('Origin',(0.,0.,0.14));
#51917=CARTESIAN_POINT('Origin',(-0.672315344701812,0.155216227497267,0.74));
#51918=CARTESIAN_POINT('',(-0.637233593757499,0.128192616740993,0.14));
#51919=CARTESIAN_POINT('',(-0.637233593757499,0.128192616740993,0.74));
#51920=CARTESIAN_POINT('',(-0.637233593757499,0.128192616740993,0.39));
#51921=CARTESIAN_POINT('',(-0.610580806867569,0.107661870153497,0.14));
#51922=CARTESIAN_POINT('',(-0.672315344701812,0.155216227497267,0.14));
#51923=CARTESIAN_POINT('',(-0.610580806867569,0.107661870153497,0.74));
#51924=CARTESIAN_POINT('',(-0.610580806867569,0.107661870153497,0.74));
#51925=CARTESIAN_POINT('',(-0.672315344701812,0.155216227497267,0.74));
#51926=CARTESIAN_POINT('Origin',(-0.647718825750041,0.119653037223409,0.74));
#51927=CARTESIAN_POINT('',(-0.642648162921854,0.0974850690781231,0.74));
#51928=CARTESIAN_POINT('Origin',(0.,0.,0.74));
#51929=CARTESIAN_POINT('',(-0.610580806867569,0.107661870153497,0.74));
#51930=CARTESIAN_POINT('Origin',(-0.610580806867569,0.107661870153497,0.74));
#51931=CARTESIAN_POINT('',(-0.642648162921854,0.0974850690781231,0.14));
#51932=CARTESIAN_POINT('',(-0.642648162921854,0.0974850690781231,0.39));
#51933=CARTESIAN_POINT('',(-0.610580806867569,0.107661870153497,0.14));
#51934=CARTESIAN_POINT('Origin',(-0.647718825750041,0.119653037223409,0.14));
#51935=CARTESIAN_POINT('Origin',(0.,0.,0.14));
#51936=CARTESIAN_POINT('Origin',(-0.578682691882343,0.375800934160369,0.74));
#51937=CARTESIAN_POINT('',(-0.55495924861976,0.338408381059618,0.14));
#51938=CARTESIAN_POINT('',(-0.55495924861976,0.338408381059618,0.74));
#51939=CARTESIAN_POINT('',(-0.55495924861976,0.338408381059618,0.39));
#51940=CARTESIAN_POINT('',(-0.536935750346352,0.31,0.14));
#51941=CARTESIAN_POINT('',(-0.578682691882343,0.375800934160369,0.14));
#51942=CARTESIAN_POINT('',(-0.536935750346352,0.31,0.74));
#51943=CARTESIAN_POINT('',(-0.536935750346352,0.31,0.74));
#51944=CARTESIAN_POINT('',(-0.578682691882343,0.375800934160369,0.74));
#51945=CARTESIAN_POINT('Origin',(-0.575865126018163,0.342900467080184,0.74));
#51946=CARTESIAN_POINT('',(-0.570549879161074,0.311404616840027,0.74));
#51947=CARTESIAN_POINT('Origin',(0.,0.,0.74));
#51948=CARTESIAN_POINT('',(-0.536935750346352,0.31,0.74));
#51949=CARTESIAN_POINT('Origin',(-0.536935750346352,0.31,0.74));
#51950=CARTESIAN_POINT('',(-0.570549879161074,0.311404616840027,0.14));
#51951=CARTESIAN_POINT('',(-0.570549879161074,0.311404616840027,0.39));
#51952=CARTESIAN_POINT('',(-0.536935750346352,0.31,0.14));
#51953=CARTESIAN_POINT('Origin',(-0.575865126018163,0.342900467080184,0.14));
#51954=CARTESIAN_POINT('Origin',(0.,0.,0.14));
#51955=CARTESIAN_POINT('Origin',(-0.415252365974913,0.551058501932632,0.74));
#51956=CARTESIAN_POINT('',(-0.405748627772263,0.507807100246665,0.14));
#51957=CARTESIAN_POINT('',(-0.405748627772263,0.507807100246665,0.74));
#51958=CARTESIAN_POINT('',(-0.405748627772263,0.507807100246665,0.39));
#51959=CARTESIAN_POINT('',(-0.398528318005654,0.474947554733766,0.14));
#51960=CARTESIAN_POINT('',(-0.415252365974913,0.551058501932632,0.14));
#51961=CARTESIAN_POINT('',(-0.398528318005654,0.474947554733766,0.74));
#51962=CARTESIAN_POINT('',(-0.398528318005654,0.474947554733766,0.74));
#51963=CARTESIAN_POINT('',(-0.415252365974913,0.551058501932632,0.74));
#51964=CARTESIAN_POINT('Origin',(-0.434553593224389,0.513003028333199,0.74));
#51965=CARTESIAN_POINT('',(-0.429634859554052,0.48776417196835,0.74));
#51966=CARTESIAN_POINT('Origin',(0.,0.,0.74));
#51967=CARTESIAN_POINT('',(-0.398528318005654,0.474947554733766,0.74));
#51968=CARTESIAN_POINT('Origin',(-0.398528318005654,0.474947554733766,0.74));
#51969=CARTESIAN_POINT('',(-0.429634859554052,0.48776417196835,0.14));
#51970=CARTESIAN_POINT('',(-0.429634859554052,0.48776417196835,0.39));
#51971=CARTESIAN_POINT('',(-0.398528318005654,0.474947554733766,0.14));
#51972=CARTESIAN_POINT('Origin',(-0.434553593224389,0.513003028333199,0.14));
#51973=CARTESIAN_POINT('Origin',(0.,0.,0.14));
#51974=CARTESIAN_POINT('Origin',(-0.201736476258688,0.659850281614495,0.74));
#51975=CARTESIAN_POINT('',(-0.207598734203447,0.615956788709343,0.14));
#51976=CARTESIAN_POINT('',(-0.207598734203447,0.615956788709343,0.74));
#51977=CARTESIAN_POINT('',(-0.207598734203447,0.615956788709343,0.39));
#51978=CARTESIAN_POINT('',(-0.212052488861915,0.582609424887263,0.14));
#51979=CARTESIAN_POINT('',(-0.201736476258688,0.659850281614495,0.14));
#51980=CARTESIAN_POINT('',(-0.212052488861915,0.582609424887263,0.74));
#51981=CARTESIAN_POINT('',(-0.212052488861915,0.582609424887263,0.74));
#51982=CARTESIAN_POINT('',(-0.201736476258688,0.659850281614495,0.74));
#51983=CARTESIAN_POINT('Origin',(-0.235670477458144,0.621229853250879,0.74));
#51984=CARTESIAN_POINT('',(-0.236899535149591,0.605292169324788,0.74));
#51985=CARTESIAN_POINT('Origin',(0.,0.,0.74));
#51986=CARTESIAN_POINT('',(-0.212052488861915,0.582609424887263,0.74));
#51987=CARTESIAN_POINT('Origin',(-0.212052488861915,0.582609424887263,0.74));
#51988=CARTESIAN_POINT('',(-0.236899535149591,0.605292169324788,0.14));
#51989=CARTESIAN_POINT('',(-0.236899535149591,0.605292169324788,0.39));
#51990=CARTESIAN_POINT('',(-0.212052488861915,0.582609424887263,0.14));
#51991=CARTESIAN_POINT('Origin',(-0.235670477458144,0.621229853250879,0.14));
#51992=CARTESIAN_POINT('Origin',(0.,0.,0.14));
#51993=CARTESIAN_POINT('Origin',(0.0361118098076313,0.689054378980656,0.74));
#51994=CARTESIAN_POINT('',(0.0155906305413142,0.649812997899645,0.14));
#51995=CARTESIAN_POINT('',(0.0155906305413142,0.649812997899645,0.74));
#51996=CARTESIAN_POINT('',(0.0155906305413142,0.649812997899645,0.39));
#51997=CARTESIAN_POINT('',(3.7964050773568E-17,0.62,0.14));
#51998=CARTESIAN_POINT('',(0.0361118098076313,0.689054378980656,0.14));
#51999=CARTESIAN_POINT('',(3.7964050773568E-17,0.62,0.74));
#52000=CARTESIAN_POINT('',(3.7964050773568E-17,0.62,0.74));
#52001=CARTESIAN_POINT('',(0.0361118098076313,0.689054378980656,0.74));
#52002=CARTESIAN_POINT('Origin',(4.16333634234434E-17,0.654527189490328,
0.74));
#52003=CARTESIAN_POINT('',(-0.0155906305413141,0.649812997899645,0.74));
#52004=CARTESIAN_POINT('Origin',(0.,0.,0.74));
#52005=CARTESIAN_POINT('',(3.7964050773568E-17,0.62,0.74));
#52006=CARTESIAN_POINT('Origin',(3.7964050773568E-17,0.62,0.74));
#52007=CARTESIAN_POINT('',(-0.0155906305413141,0.649812997899645,0.14));
#52008=CARTESIAN_POINT('',(-0.0155906305413141,0.649812997899645,0.39));
#52009=CARTESIAN_POINT('',(3.7964050773568E-17,0.62,0.14));
#52010=CARTESIAN_POINT('Origin',(4.16333634234434E-17,0.654527189490328,
0.14));
#52011=CARTESIAN_POINT('Origin',(0.,0.,0.14));
#52012=CARTESIAN_POINT('Origin',(0.269604478657599,0.635148348882184,0.74));
#52013=CARTESIAN_POINT('',(0.236899535149591,0.605292169324788,0.14));
#52014=CARTESIAN_POINT('',(0.236899535149591,0.605292169324788,0.74));
#52015=CARTESIAN_POINT('',(0.236899535149591,0.605292169324788,0.39));
#52016=CARTESIAN_POINT('',(0.212052488861915,0.582609424887263,0.14));
#52017=CARTESIAN_POINT('',(0.269604478657599,0.635148348882184,0.14));
#52018=CARTESIAN_POINT('',(0.212052488861915,0.582609424887263,0.74));
#52019=CARTESIAN_POINT('',(0.212052488861915,0.582609424887263,0.74));
#52020=CARTESIAN_POINT('',(0.269604478657599,0.635148348882184,0.74));
#52021=CARTESIAN_POINT('Origin',(0.235670477458144,0.621229853250879,0.74));
#52022=CARTESIAN_POINT('',(0.207598734203447,0.615956788709343,0.74));
#52023=CARTESIAN_POINT('Origin',(0.,0.,0.74));
#52024=CARTESIAN_POINT('',(0.212052488861915,0.582609424887263,0.74));
#52025=CARTESIAN_POINT('Origin',(0.212052488861915,0.582609424887263,0.74));
#52026=CARTESIAN_POINT('',(0.207598734203447,0.615956788709343,0.14));
#52027=CARTESIAN_POINT('',(0.207598734203447,0.615956788709343,0.39));
#52028=CARTESIAN_POINT('',(0.212052488861915,0.582609424887263,0.14));
#52029=CARTESIAN_POINT('Origin',(0.235670477458144,0.621229853250879,0.14));
#52030=CARTESIAN_POINT('Origin',(0.,0.,0.14));
#52031=CARTESIAN_POINT('Origin',(0.470578868443124,0.504634054117228,0.74));
#52032=CARTESIAN_POINT('',(0.429634859554052,0.48776417196835,0.14));
#52033=CARTESIAN_POINT('',(0.429634859554052,0.48776417196835,0.74));
#52034=CARTESIAN_POINT('',(0.429634859554052,0.48776417196835,0.39));
#52035=CARTESIAN_POINT('',(0.398528318005654,0.474947554733766,0.14));
#52036=CARTESIAN_POINT('',(0.470578868443124,0.504634054117228,0.14));
#52037=CARTESIAN_POINT('',(0.398528318005654,0.474947554733766,0.74));
#52038=CARTESIAN_POINT('',(0.398528318005654,0.474947554733766,0.74));
#52039=CARTESIAN_POINT('',(0.470578868443124,0.504634054117228,0.74));
#52040=CARTESIAN_POINT('Origin',(0.434553593224389,0.513003028333199,0.74));
#52041=CARTESIAN_POINT('',(0.405748627772262,0.507807100246665,0.74));
#52042=CARTESIAN_POINT('Origin',(0.,0.,0.74));
#52043=CARTESIAN_POINT('',(0.398528318005654,0.474947554733766,0.74));
#52044=CARTESIAN_POINT('Origin',(0.398528318005654,0.474947554733766,0.74));
#52045=CARTESIAN_POINT('',(0.405748627772262,0.507807100246665,0.14));
#52046=CARTESIAN_POINT('',(0.405748627772262,0.507807100246665,0.39));
#52047=CARTESIAN_POINT('',(0.398528318005654,0.474947554733766,0.14));
#52048=CARTESIAN_POINT('Origin',(0.434553593224389,0.513003028333199,0.14));
#52049=CARTESIAN_POINT('Origin',(0.,0.,0.14));
#52050=CARTESIAN_POINT('Origin',(0.614794501689974,0.313253444820287,0.74));
#52051=CARTESIAN_POINT('',(0.570549879161074,0.311404616840027,0.14));
#52052=CARTESIAN_POINT('',(0.570549879161074,0.311404616840027,0.74));
#52053=CARTESIAN_POINT('',(0.570549879161074,0.311404616840027,0.39));
#52054=CARTESIAN_POINT('',(0.536935750346352,0.31,0.14));
#52055=CARTESIAN_POINT('',(0.614794501689974,0.313253444820287,0.14));
#52056=CARTESIAN_POINT('',(0.536935750346352,0.31,0.74));
#52057=CARTESIAN_POINT('',(0.536935750346352,0.31,0.74));
#52058=CARTESIAN_POINT('',(0.614794501689974,0.313253444820287,0.74));
#52059=CARTESIAN_POINT('Origin',(0.575865126018163,0.342900467080184,0.74));
#52060=CARTESIAN_POINT('',(0.55495924861976,0.338408381059618,0.74));
#52061=CARTESIAN_POINT('Origin',(0.,0.,0.74));
#52062=CARTESIAN_POINT('',(0.536935750346352,0.31,0.74));
#52063=CARTESIAN_POINT('Origin',(0.536935750346352,0.31,0.74));
#52064=CARTESIAN_POINT('',(0.55495924861976,0.338408381059618,0.14));
#52065=CARTESIAN_POINT('',(0.55495924861976,0.338408381059618,0.39));
#52066=CARTESIAN_POINT('',(0.536935750346352,0.31,0.14));
#52067=CARTESIAN_POINT('Origin',(0.575865126018163,0.342900467080184,0.14));
#52068=CARTESIAN_POINT('Origin',(0.,0.,0.14));
#52069=CARTESIAN_POINT('Origin',(0.684856844632512,0.0840898469495518,0.74));
#52070=CARTESIAN_POINT('',(0.642648162921854,0.0974850690781231,0.14));
#52071=CARTESIAN_POINT('',(0.642648162921854,0.0974850690781231,0.74));
#52072=CARTESIAN_POINT('',(0.642648162921854,0.0974850690781232,0.39));
#52073=CARTESIAN_POINT('',(0.610580806867569,0.107661870153497,0.14));
#52074=CARTESIAN_POINT('',(0.684856844632512,0.0840898469495518,0.14));
#52075=CARTESIAN_POINT('',(0.610580806867569,0.107661870153497,0.74));
#52076=CARTESIAN_POINT('',(0.610580806867569,0.107661870153497,0.74));
#52077=CARTESIAN_POINT('',(0.684856844632512,0.0840898469495518,0.74));
#52078=CARTESIAN_POINT('Origin',(0.647718825750041,0.119653037223409,0.74));
#52079=CARTESIAN_POINT('',(0.637233593757499,0.128192616740993,0.74));
#52080=CARTESIAN_POINT('Origin',(0.,0.,0.74));
#52081=CARTESIAN_POINT('',(0.610580806867569,0.107661870153497,0.74));
#52082=CARTESIAN_POINT('Origin',(0.610580806867569,0.107661870153497,0.74));
#52083=CARTESIAN_POINT('',(0.637233593757499,0.128192616740993,0.14));
#52084=CARTESIAN_POINT('',(0.637233593757499,0.128192616740993,0.39));
#52085=CARTESIAN_POINT('',(0.610580806867569,0.107661870153497,0.14));
#52086=CARTESIAN_POINT('Origin',(0.647718825750041,0.119653037223409,0.14));
#52087=CARTESIAN_POINT('Origin',(0.,0.,0.14));
#52088=CARTESIAN_POINT('Origin',(0.659850281614495,0.201736476258688,0.74));
#52089=CARTESIAN_POINT('',(0.615956788709343,0.207598734203447,0.14));
#52090=CARTESIAN_POINT('',(0.615956788709343,0.207598734203447,0.74));
#52091=CARTESIAN_POINT('',(0.615956788709343,0.207598734203447,0.39));
#52092=CARTESIAN_POINT('',(0.582609424887263,0.212052488861915,0.14));
#52093=CARTESIAN_POINT('',(0.659850281614495,0.201736476258688,0.14));
#52094=CARTESIAN_POINT('',(0.582609424887263,0.212052488861915,0.74));
#52095=CARTESIAN_POINT('',(0.582609424887263,0.212052488861915,0.74));
#52096=CARTESIAN_POINT('',(0.659850281614495,0.201736476258688,0.74));
#52097=CARTESIAN_POINT('Origin',(0.621229853250879,0.235670477458144,0.74));
#52098=CARTESIAN_POINT('',(0.605292169324788,0.236899535149591,0.74));
#52099=CARTESIAN_POINT('Origin',(0.,0.,0.74));
#52100=CARTESIAN_POINT('',(0.582609424887263,0.212052488861915,0.74));
#52101=CARTESIAN_POINT('Origin',(0.582609424887263,0.212052488861915,0.74));
#52102=CARTESIAN_POINT('',(0.605292169324788,0.236899535149591,0.14));
#52103=CARTESIAN_POINT('',(0.605292169324788,0.236899535149591,0.39));
#52104=CARTESIAN_POINT('',(0.582609424887263,0.212052488861915,0.14));
#52105=CARTESIAN_POINT('Origin',(0.621229853250879,0.235670477458144,0.14));
#52106=CARTESIAN_POINT('Origin',(0.,0.,0.14));
#52107=CARTESIAN_POINT('Origin',(0.551058501932632,0.415252365974913,0.74));
#52108=CARTESIAN_POINT('',(0.507807100246665,0.405748627772262,0.14));
#52109=CARTESIAN_POINT('',(0.507807100246665,0.405748627772262,0.74));
#52110=CARTESIAN_POINT('',(0.507807100246665,0.405748627772262,0.39));
#52111=CARTESIAN_POINT('',(0.474947554733766,0.398528318005654,0.14));
#52112=CARTESIAN_POINT('',(0.551058501932632,0.415252365974913,0.14));
#52113=CARTESIAN_POINT('',(0.474947554733766,0.398528318005654,0.74));
#52114=CARTESIAN_POINT('',(0.474947554733766,0.398528318005654,0.74));
#52115=CARTESIAN_POINT('',(0.551058501932632,0.415252365974913,0.74));
#52116=CARTESIAN_POINT('Origin',(0.513003028333199,0.434553593224389,0.74));
#52117=CARTESIAN_POINT('',(0.48776417196835,0.429634859554052,0.74));
#52118=CARTESIAN_POINT('Origin',(0.,0.,0.74));
#52119=CARTESIAN_POINT('',(0.474947554733766,0.398528318005654,0.74));
#52120=CARTESIAN_POINT('Origin',(0.474947554733766,0.398528318005654,0.74));
#52121=CARTESIAN_POINT('',(0.48776417196835,0.429634859554052,0.14));
#52122=CARTESIAN_POINT('',(0.48776417196835,0.429634859554052,0.39));
#52123=CARTESIAN_POINT('',(0.474947554733766,0.398528318005654,0.14));
#52124=CARTESIAN_POINT('Origin',(0.513003028333199,0.434553593224389,0.14));
#52125=CARTESIAN_POINT('Origin',(0.,0.,0.14));
#52126=CARTESIAN_POINT('Origin',(0.375800934160369,0.578682691882343,0.74));
#52127=CARTESIAN_POINT('',(0.338408381059618,0.55495924861976,0.14));
#52128=CARTESIAN_POINT('',(0.338408381059618,0.55495924861976,0.74));
#52129=CARTESIAN_POINT('',(0.338408381059618,0.55495924861976,0.39));
#52130=CARTESIAN_POINT('',(0.31,0.536935750346352,0.14));
#52131=CARTESIAN_POINT('',(0.375800934160369,0.578682691882343,0.14));
#52132=CARTESIAN_POINT('',(0.31,0.536935750346352,0.74));
#52133=CARTESIAN_POINT('',(0.31,0.536935750346352,0.74));
#52134=CARTESIAN_POINT('',(0.375800934160369,0.578682691882343,0.74));
#52135=CARTESIAN_POINT('Origin',(0.342900467080184,0.575865126018163,0.74));
#52136=CARTESIAN_POINT('',(0.311404616840027,0.570549879161074,0.74));
#52137=CARTESIAN_POINT('Origin',(0.,0.,0.74));
#52138=CARTESIAN_POINT('',(0.31,0.536935750346352,0.74));
#52139=CARTESIAN_POINT('Origin',(0.31,0.536935750346352,0.74));
#52140=CARTESIAN_POINT('',(0.311404616840027,0.570549879161074,0.14));
#52141=CARTESIAN_POINT('',(0.311404616840027,0.570549879161074,0.39));
#52142=CARTESIAN_POINT('',(0.31,0.536935750346352,0.14));
#52143=CARTESIAN_POINT('Origin',(0.342900467080184,0.575865126018163,0.14));
#52144=CARTESIAN_POINT('Origin',(0.,0.,0.14));
#52145=CARTESIAN_POINT('Origin',(0.155216227497267,0.672315344701812,0.74));
#52146=CARTESIAN_POINT('',(0.128192616740993,0.637233593757499,0.14));
#52147=CARTESIAN_POINT('',(0.128192616740993,0.637233593757499,0.74));
#52148=CARTESIAN_POINT('',(0.128192616740993,0.637233593757499,0.39));
#52149=CARTESIAN_POINT('',(0.107661870153497,0.610580806867569,0.14));
#52150=CARTESIAN_POINT('',(0.155216227497267,0.672315344701812,0.14));
#52151=CARTESIAN_POINT('',(0.107661870153497,0.610580806867569,0.74));
#52152=CARTESIAN_POINT('',(0.107661870153497,0.610580806867569,0.74));
#52153=CARTESIAN_POINT('',(0.155216227497267,0.672315344701812,0.74));
#52154=CARTESIAN_POINT('Origin',(0.119653037223409,0.647718825750041,0.74));
#52155=CARTESIAN_POINT('',(0.0974850690781232,0.642648162921854,0.74));
#52156=CARTESIAN_POINT('Origin',(0.,0.,0.74));
#52157=CARTESIAN_POINT('',(0.107661870153497,0.610580806867569,0.74));
#52158=CARTESIAN_POINT('Origin',(0.107661870153497,0.610580806867569,0.74));
#52159=CARTESIAN_POINT('',(0.0974850690781232,0.642648162921854,0.14));
#52160=CARTESIAN_POINT('',(0.0974850690781232,0.642648162921854,0.39));
#52161=CARTESIAN_POINT('',(0.107661870153497,0.610580806867569,0.14));
#52162=CARTESIAN_POINT('Origin',(0.119653037223409,0.647718825750041,0.14));
#52163=CARTESIAN_POINT('Origin',(0.,0.,0.14));
#52164=CARTESIAN_POINT('Origin',(-0.0840898469495517,0.684856844632512,
0.74));
#52165=CARTESIAN_POINT('',(-0.0974850690781231,0.642648162921854,0.14));
#52166=CARTESIAN_POINT('',(-0.0974850690781231,0.642648162921854,0.74));
#52167=CARTESIAN_POINT('',(-0.0974850690781231,0.642648162921854,0.39));
#52168=CARTESIAN_POINT('',(-0.107661870153497,0.610580806867569,0.14));
#52169=CARTESIAN_POINT('',(-0.0840898469495517,0.684856844632512,0.14));
#52170=CARTESIAN_POINT('',(-0.107661870153497,0.610580806867569,0.74));
#52171=CARTESIAN_POINT('',(-0.107661870153497,0.610580806867569,0.74));
#52172=CARTESIAN_POINT('',(-0.0840898469495517,0.684856844632512,0.74));
#52173=CARTESIAN_POINT('Origin',(-0.119653037223409,0.647718825750041,0.74));
#52174=CARTESIAN_POINT('',(-0.128192616740993,0.637233593757499,0.74));
#52175=CARTESIAN_POINT('Origin',(0.,0.,0.74));
#52176=CARTESIAN_POINT('',(-0.107661870153497,0.610580806867569,0.74));
#52177=CARTESIAN_POINT('Origin',(-0.107661870153497,0.610580806867569,0.74));
#52178=CARTESIAN_POINT('',(-0.128192616740993,0.637233593757499,0.14));
#52179=CARTESIAN_POINT('',(-0.128192616740993,0.637233593757499,0.39));
#52180=CARTESIAN_POINT('',(-0.107661870153497,0.610580806867569,0.14));
#52181=CARTESIAN_POINT('Origin',(-0.119653037223409,0.647718825750041,0.14));
#52182=CARTESIAN_POINT('Origin',(0.,0.,0.14));
#52183=CARTESIAN_POINT('Origin',(-0.313253444820287,0.614794501689974,0.74));
#52184=CARTESIAN_POINT('',(-0.311404616840027,0.570549879161074,0.14));
#52185=CARTESIAN_POINT('',(-0.311404616840027,0.570549879161074,0.74));
#52186=CARTESIAN_POINT('',(-0.311404616840027,0.570549879161074,0.39));
#52187=CARTESIAN_POINT('',(-0.31,0.536935750346352,0.14));
#52188=CARTESIAN_POINT('',(-0.313253444820287,0.614794501689974,0.14));
#52189=CARTESIAN_POINT('',(-0.31,0.536935750346352,0.74));
#52190=CARTESIAN_POINT('',(-0.31,0.536935750346352,0.74));
#52191=CARTESIAN_POINT('',(-0.313253444820287,0.614794501689974,0.74));
#52192=CARTESIAN_POINT('Origin',(-0.342900467080184,0.575865126018163,0.74));
#52193=CARTESIAN_POINT('',(-0.338408381059618,0.55495924861976,0.74));
#52194=CARTESIAN_POINT('Origin',(0.,0.,0.74));
#52195=CARTESIAN_POINT('',(-0.31,0.536935750346352,0.74));
#52196=CARTESIAN_POINT('Origin',(-0.31,0.536935750346352,0.74));
#52197=CARTESIAN_POINT('',(-0.338408381059618,0.55495924861976,0.14));
#52198=CARTESIAN_POINT('',(-0.338408381059618,0.55495924861976,0.39));
#52199=CARTESIAN_POINT('',(-0.31,0.536935750346352,0.14));
#52200=CARTESIAN_POINT('Origin',(-0.342900467080184,0.575865126018163,0.14));
#52201=CARTESIAN_POINT('Origin',(0.,0.,0.14));
#52202=CARTESIAN_POINT('Origin',(-0.504634054117228,0.470578868443124,0.74));
#52203=CARTESIAN_POINT('',(-0.48776417196835,0.429634859554052,0.14));
#52204=CARTESIAN_POINT('',(-0.48776417196835,0.429634859554052,0.74));
#52205=CARTESIAN_POINT('',(-0.48776417196835,0.429634859554052,0.39));
#52206=CARTESIAN_POINT('',(-0.474947554733766,0.398528318005654,0.14));
#52207=CARTESIAN_POINT('',(-0.504634054117228,0.470578868443124,0.14));
#52208=CARTESIAN_POINT('',(-0.474947554733766,0.398528318005654,0.74));
#52209=CARTESIAN_POINT('',(-0.474947554733766,0.398528318005654,0.74));
#52210=CARTESIAN_POINT('',(-0.504634054117228,0.470578868443124,0.74));
#52211=CARTESIAN_POINT('Origin',(-0.513003028333199,0.434553593224389,0.74));
#52212=CARTESIAN_POINT('',(-0.507807100246665,0.405748627772262,0.74));
#52213=CARTESIAN_POINT('Origin',(0.,0.,0.74));
#52214=CARTESIAN_POINT('',(-0.474947554733766,0.398528318005654,0.74));
#52215=CARTESIAN_POINT('Origin',(-0.474947554733766,0.398528318005654,0.74));
#52216=CARTESIAN_POINT('',(-0.507807100246665,0.405748627772262,0.14));
#52217=CARTESIAN_POINT('',(-0.507807100246665,0.405748627772262,0.39));
#52218=CARTESIAN_POINT('',(-0.474947554733766,0.398528318005654,0.14));
#52219=CARTESIAN_POINT('Origin',(-0.513003028333199,0.434553593224389,0.14));
#52220=CARTESIAN_POINT('Origin',(0.,0.,0.14));
#52221=CARTESIAN_POINT('Origin',(-0.635148348882184,0.269604478657599,0.74));
#52222=CARTESIAN_POINT('',(-0.605292169324788,0.236899535149591,0.14));
#52223=CARTESIAN_POINT('',(-0.605292169324788,0.236899535149591,0.74));
#52224=CARTESIAN_POINT('',(-0.605292169324788,0.236899535149591,0.39));
#52225=CARTESIAN_POINT('',(-0.582609424887263,0.212052488861915,0.14));
#52226=CARTESIAN_POINT('',(-0.635148348882184,0.269604478657599,0.14));
#52227=CARTESIAN_POINT('',(-0.582609424887263,0.212052488861915,0.74));
#52228=CARTESIAN_POINT('',(-0.582609424887263,0.212052488861915,0.74));
#52229=CARTESIAN_POINT('',(-0.635148348882184,0.269604478657599,0.74));
#52230=CARTESIAN_POINT('Origin',(-0.621229853250879,0.235670477458144,0.74));
#52231=CARTESIAN_POINT('',(-0.615956788709343,0.207598734203447,0.74));
#52232=CARTESIAN_POINT('Origin',(0.,0.,0.74));
#52233=CARTESIAN_POINT('',(-0.582609424887263,0.212052488861915,0.74));
#52234=CARTESIAN_POINT('Origin',(-0.582609424887263,0.212052488861915,0.74));
#52235=CARTESIAN_POINT('',(-0.615956788709343,0.207598734203447,0.14));
#52236=CARTESIAN_POINT('',(-0.615956788709343,0.207598734203447,0.39));
#52237=CARTESIAN_POINT('',(-0.582609424887263,0.212052488861915,0.14));
#52238=CARTESIAN_POINT('Origin',(-0.621229853250879,0.235670477458144,0.14));
#52239=CARTESIAN_POINT('Origin',(0.,0.,0.14));
#52240=CARTESIAN_POINT('Origin',(0.654527189490328,0.,0.74));
#52241=CARTESIAN_POINT('',(0.649812997899645,-0.0155906305413142,0.74));
#52242=CARTESIAN_POINT('',(0.649812997899645,0.0155906305413142,0.74));
#52243=CARTESIAN_POINT('Origin',(0.,0.,0.74));
#52244=CARTESIAN_POINT('',(0.62,0.,0.74));
#52245=CARTESIAN_POINT('',(0.689054378980656,-0.0361118098076312,0.74));
#52246=CARTESIAN_POINT('',(0.62,0.,0.74));
#52247=CARTESIAN_POINT('Origin',(0.689054378980656,-0.0361118098076312,
0.74));
#52248=CARTESIAN_POINT('',(0.649812997899645,-0.0155906305413142,0.14));
#52249=CARTESIAN_POINT('',(0.649812997899645,-0.0155906305413142,0.39));
#52250=CARTESIAN_POINT('',(0.62,0.,0.14));
#52251=CARTESIAN_POINT('',(0.689054378980656,-0.0361118098076312,0.14));
#52252=CARTESIAN_POINT('',(0.62,0.,0.74));
#52253=CARTESIAN_POINT('Origin',(0.62,0.,0.74));
#52254=CARTESIAN_POINT('',(0.649812997899645,0.0155906305413142,0.14));
#52255=CARTESIAN_POINT('',(0.649812997899645,0.0155906305413142,0.39));
#52256=CARTESIAN_POINT('',(0.62,0.,0.14));
#52257=CARTESIAN_POINT('Origin',(0.654527189490328,0.,0.14));
#52258=CARTESIAN_POINT('Origin',(0.,0.,0.14));
#52259=CARTESIAN_POINT('Origin',(-0.684856844632512,-0.0840898469495517,
0.74));
#52260=CARTESIAN_POINT('',(-0.642648162921854,-0.0974850690781232,0.14));
#52261=CARTESIAN_POINT('',(-0.642648162921854,-0.0974850690781232,0.74));
#52262=CARTESIAN_POINT('',(-0.642648162921854,-0.0974850690781232,0.39));
#52263=CARTESIAN_POINT('',(-0.610580806867569,-0.107661870153497,0.14));
#52264=CARTESIAN_POINT('',(-0.684856844632512,-0.0840898469495517,0.14));
#52265=CARTESIAN_POINT('',(-0.610580806867569,-0.107661870153497,0.74));
#52266=CARTESIAN_POINT('',(-0.610580806867569,-0.107661870153497,0.74));
#52267=CARTESIAN_POINT('',(-0.684856844632512,-0.0840898469495517,0.74));
#52268=CARTESIAN_POINT('Origin',(-0.647718825750041,-0.119653037223409,
0.74));
#52269=CARTESIAN_POINT('',(-0.637233593757499,-0.128192616740993,0.74));
#52270=CARTESIAN_POINT('Origin',(0.,0.,0.74));
#52271=CARTESIAN_POINT('',(-0.610580806867569,-0.107661870153497,0.74));
#52272=CARTESIAN_POINT('Origin',(-0.610580806867569,-0.107661870153497,
0.74));
#52273=CARTESIAN_POINT('',(-0.637233593757499,-0.128192616740993,0.14));
#52274=CARTESIAN_POINT('',(-0.637233593757499,-0.128192616740993,0.39));
#52275=CARTESIAN_POINT('',(-0.610580806867569,-0.107661870153497,0.14));
#52276=CARTESIAN_POINT('Origin',(-0.647718825750041,-0.119653037223409,
0.14));
#52277=CARTESIAN_POINT('Origin',(0.,0.,0.14));
#52278=CARTESIAN_POINT('Origin',(-0.614794501689974,-0.313253444820287,
0.74));
#52279=CARTESIAN_POINT('',(-0.570549879161074,-0.311404616840027,0.14));
#52280=CARTESIAN_POINT('',(-0.570549879161074,-0.311404616840027,0.74));
#52281=CARTESIAN_POINT('',(-0.570549879161074,-0.311404616840027,0.39));
#52282=CARTESIAN_POINT('',(-0.536935750346352,-0.31,0.14));
#52283=CARTESIAN_POINT('',(-0.614794501689974,-0.313253444820287,0.14));
#52284=CARTESIAN_POINT('',(-0.536935750346352,-0.31,0.74));
#52285=CARTESIAN_POINT('',(-0.536935750346352,-0.31,0.74));
#52286=CARTESIAN_POINT('',(-0.614794501689974,-0.313253444820287,0.74));
#52287=CARTESIAN_POINT('Origin',(-0.575865126018163,-0.342900467080184,
0.74));
#52288=CARTESIAN_POINT('',(-0.55495924861976,-0.338408381059618,0.74));
#52289=CARTESIAN_POINT('Origin',(0.,0.,0.74));
#52290=CARTESIAN_POINT('',(-0.536935750346352,-0.31,0.74));
#52291=CARTESIAN_POINT('Origin',(-0.536935750346352,-0.31,0.74));
#52292=CARTESIAN_POINT('',(-0.55495924861976,-0.338408381059618,0.14));
#52293=CARTESIAN_POINT('',(-0.55495924861976,-0.338408381059618,0.39));
#52294=CARTESIAN_POINT('',(-0.536935750346352,-0.31,0.14));
#52295=CARTESIAN_POINT('Origin',(-0.575865126018163,-0.342900467080184,
0.14));
#52296=CARTESIAN_POINT('Origin',(0.,0.,0.14));
#52297=CARTESIAN_POINT('Origin',(-0.470578868443124,-0.504634054117228,
0.74));
#52298=CARTESIAN_POINT('',(-0.429634859554052,-0.48776417196835,0.14));
#52299=CARTESIAN_POINT('',(-0.429634859554052,-0.48776417196835,0.74));
#52300=CARTESIAN_POINT('',(-0.429634859554052,-0.48776417196835,0.39));
#52301=CARTESIAN_POINT('',(-0.398528318005654,-0.474947554733766,0.14));
#52302=CARTESIAN_POINT('',(-0.470578868443124,-0.504634054117228,0.14));
#52303=CARTESIAN_POINT('',(-0.398528318005654,-0.474947554733766,0.74));
#52304=CARTESIAN_POINT('',(-0.398528318005654,-0.474947554733766,0.74));
#52305=CARTESIAN_POINT('',(-0.470578868443124,-0.504634054117228,0.74));
#52306=CARTESIAN_POINT('Origin',(-0.434553593224389,-0.513003028333199,
0.74));
#52307=CARTESIAN_POINT('',(-0.405748627772262,-0.507807100246665,0.74));
#52308=CARTESIAN_POINT('Origin',(0.,0.,0.74));
#52309=CARTESIAN_POINT('',(-0.398528318005654,-0.474947554733766,0.74));
#52310=CARTESIAN_POINT('Origin',(-0.398528318005654,-0.474947554733766,
0.74));
#52311=CARTESIAN_POINT('',(-0.405748627772262,-0.507807100246665,0.14));
#52312=CARTESIAN_POINT('',(-0.405748627772263,-0.507807100246665,0.39));
#52313=CARTESIAN_POINT('',(-0.398528318005654,-0.474947554733766,0.14));
#52314=CARTESIAN_POINT('Origin',(-0.434553593224389,-0.513003028333199,
0.14));
#52315=CARTESIAN_POINT('Origin',(0.,0.,0.14));
#52316=CARTESIAN_POINT('Origin',(-0.269604478657599,-0.635148348882184,
0.74));
#52317=CARTESIAN_POINT('',(-0.236899535149592,-0.605292169324788,0.14));
#52318=CARTESIAN_POINT('',(-0.236899535149592,-0.605292169324788,0.74));
#52319=CARTESIAN_POINT('',(-0.236899535149592,-0.605292169324788,0.39));
#52320=CARTESIAN_POINT('',(-0.212052488861914,-0.582609424887263,0.14));
#52321=CARTESIAN_POINT('',(-0.269604478657599,-0.635148348882184,0.14));
#52322=CARTESIAN_POINT('',(-0.212052488861914,-0.582609424887263,0.74));
#52323=CARTESIAN_POINT('',(-0.212052488861914,-0.582609424887263,0.74));
#52324=CARTESIAN_POINT('',(-0.269604478657599,-0.635148348882184,0.74));
#52325=CARTESIAN_POINT('Origin',(-0.235670477458144,-0.621229853250879,
0.74));
#52326=CARTESIAN_POINT('',(-0.207598734203447,-0.615956788709343,0.74));
#52327=CARTESIAN_POINT('Origin',(0.,0.,0.74));
#52328=CARTESIAN_POINT('',(-0.212052488861914,-0.582609424887263,0.74));
#52329=CARTESIAN_POINT('Origin',(-0.212052488861914,-0.582609424887263,
0.74));
#52330=CARTESIAN_POINT('',(-0.207598734203447,-0.615956788709343,0.14));
#52331=CARTESIAN_POINT('',(-0.207598734203447,-0.615956788709343,0.39));
#52332=CARTESIAN_POINT('',(-0.212052488861914,-0.582609424887263,0.14));
#52333=CARTESIAN_POINT('Origin',(-0.235670477458144,-0.621229853250879,
0.14));
#52334=CARTESIAN_POINT('Origin',(0.,0.,0.14));
#52335=CARTESIAN_POINT('Origin',(-0.0361118098076316,-0.689054378980656,
0.74));
#52336=CARTESIAN_POINT('',(-0.0155906305413143,-0.649812997899645,0.14));
#52337=CARTESIAN_POINT('',(-0.0155906305413143,-0.649812997899645,0.74));
#52338=CARTESIAN_POINT('',(-0.0155906305413143,-0.649812997899645,0.39));
#52339=CARTESIAN_POINT('',(-1.13892152320704E-16,-0.62,0.14));
#52340=CARTESIAN_POINT('',(-0.0361118098076316,-0.689054378980656,0.14));
#52341=CARTESIAN_POINT('',(-1.13892152320704E-16,-0.62,0.74));
#52342=CARTESIAN_POINT('',(-1.13892152320704E-16,-0.62,0.74));
#52343=CARTESIAN_POINT('',(-0.0361118098076316,-0.689054378980656,0.74));
#52344=CARTESIAN_POINT('Origin',(-1.2490009027033E-16,-0.654527189490328,
0.74));
#52345=CARTESIAN_POINT('',(0.0155906305413141,-0.649812997899645,0.74));
#52346=CARTESIAN_POINT('Origin',(0.,0.,0.74));
#52347=CARTESIAN_POINT('',(-1.13892152320704E-16,-0.62,0.74));
#52348=CARTESIAN_POINT('Origin',(-1.13892152320704E-16,-0.62,0.74));
#52349=CARTESIAN_POINT('',(0.0155906305413141,-0.649812997899645,0.14));
#52350=CARTESIAN_POINT('',(0.0155906305413141,-0.649812997899645,0.39));
#52351=CARTESIAN_POINT('',(-1.13892152320704E-16,-0.62,0.14));
#52352=CARTESIAN_POINT('Origin',(-1.2490009027033E-16,-0.654527189490328,
0.14));
#52353=CARTESIAN_POINT('Origin',(0.,0.,0.14));
#52354=CARTESIAN_POINT('Origin',(0.201736476258688,-0.659850281614495,0.74));
#52355=CARTESIAN_POINT('',(0.207598734203447,-0.615956788709343,0.14));
#52356=CARTESIAN_POINT('',(0.207598734203447,-0.615956788709343,0.74));
#52357=CARTESIAN_POINT('',(0.207598734203447,-0.615956788709343,0.39));
#52358=CARTESIAN_POINT('',(0.212052488861915,-0.582609424887263,0.14));
#52359=CARTESIAN_POINT('',(0.201736476258688,-0.659850281614495,0.14));
#52360=CARTESIAN_POINT('',(0.212052488861915,-0.582609424887263,0.74));
#52361=CARTESIAN_POINT('',(0.212052488861915,-0.582609424887263,0.74));
#52362=CARTESIAN_POINT('',(0.201736476258688,-0.659850281614495,0.74));
#52363=CARTESIAN_POINT('Origin',(0.235670477458144,-0.621229853250879,0.74));
#52364=CARTESIAN_POINT('',(0.236899535149591,-0.605292169324788,0.74));
#52365=CARTESIAN_POINT('Origin',(0.,0.,0.74));
#52366=CARTESIAN_POINT('',(0.212052488861915,-0.582609424887263,0.74));
#52367=CARTESIAN_POINT('Origin',(0.212052488861915,-0.582609424887263,0.74));
#52368=CARTESIAN_POINT('',(0.236899535149591,-0.605292169324788,0.14));
#52369=CARTESIAN_POINT('',(0.236899535149591,-0.605292169324788,0.39));
#52370=CARTESIAN_POINT('',(0.212052488861915,-0.582609424887263,0.14));
#52371=CARTESIAN_POINT('Origin',(0.235670477458144,-0.621229853250879,0.14));
#52372=CARTESIAN_POINT('Origin',(0.,0.,0.14));
#52373=CARTESIAN_POINT('Origin',(0.415252365974913,-0.551058501932632,0.74));
#52374=CARTESIAN_POINT('',(0.405748627772262,-0.507807100246665,0.14));
#52375=CARTESIAN_POINT('',(0.405748627772262,-0.507807100246665,0.74));
#52376=CARTESIAN_POINT('',(0.405748627772262,-0.507807100246665,0.39));
#52377=CARTESIAN_POINT('',(0.398528318005654,-0.474947554733766,0.14));
#52378=CARTESIAN_POINT('',(0.415252365974913,-0.551058501932632,0.14));
#52379=CARTESIAN_POINT('',(0.398528318005654,-0.474947554733766,0.74));
#52380=CARTESIAN_POINT('',(0.398528318005654,-0.474947554733766,0.74));
#52381=CARTESIAN_POINT('',(0.415252365974913,-0.551058501932632,0.74));
#52382=CARTESIAN_POINT('Origin',(0.434553593224389,-0.513003028333199,0.74));
#52383=CARTESIAN_POINT('',(0.429634859554052,-0.48776417196835,0.74));
#52384=CARTESIAN_POINT('Origin',(0.,0.,0.74));
#52385=CARTESIAN_POINT('',(0.398528318005654,-0.474947554733766,0.74));
#52386=CARTESIAN_POINT('Origin',(0.398528318005654,-0.474947554733766,0.74));
#52387=CARTESIAN_POINT('',(0.429634859554052,-0.48776417196835,0.14));
#52388=CARTESIAN_POINT('',(0.429634859554052,-0.48776417196835,0.39));
#52389=CARTESIAN_POINT('',(0.398528318005654,-0.474947554733766,0.14));
#52390=CARTESIAN_POINT('Origin',(0.434553593224389,-0.513003028333199,0.14));
#52391=CARTESIAN_POINT('Origin',(0.,0.,0.14));
#52392=CARTESIAN_POINT('Origin',(0.578682691882343,-0.375800934160369,0.74));
#52393=CARTESIAN_POINT('',(0.55495924861976,-0.338408381059618,0.14));
#52394=CARTESIAN_POINT('',(0.55495924861976,-0.338408381059618,0.74));
#52395=CARTESIAN_POINT('',(0.55495924861976,-0.338408381059618,0.39));
#52396=CARTESIAN_POINT('',(0.536935750346352,-0.31,0.14));
#52397=CARTESIAN_POINT('',(0.578682691882343,-0.375800934160369,0.14));
#52398=CARTESIAN_POINT('',(0.536935750346352,-0.31,0.74));
#52399=CARTESIAN_POINT('',(0.536935750346352,-0.31,0.74));
#52400=CARTESIAN_POINT('',(0.578682691882343,-0.375800934160369,0.74));
#52401=CARTESIAN_POINT('Origin',(0.575865126018163,-0.342900467080184,0.74));
#52402=CARTESIAN_POINT('',(0.570549879161074,-0.311404616840027,0.74));
#52403=CARTESIAN_POINT('Origin',(0.,0.,0.74));
#52404=CARTESIAN_POINT('',(0.536935750346352,-0.31,0.74));
#52405=CARTESIAN_POINT('Origin',(0.536935750346352,-0.31,0.74));
#52406=CARTESIAN_POINT('',(0.570549879161074,-0.311404616840027,0.14));
#52407=CARTESIAN_POINT('',(0.570549879161074,-0.311404616840027,0.39));
#52408=CARTESIAN_POINT('',(0.536935750346352,-0.31,0.14));
#52409=CARTESIAN_POINT('Origin',(0.575865126018163,-0.342900467080184,0.14));
#52410=CARTESIAN_POINT('Origin',(0.,0.,0.14));
#52411=CARTESIAN_POINT('Origin',(0.672315344701812,-0.155216227497267,0.74));
#52412=CARTESIAN_POINT('',(0.637233593757499,-0.128192616740993,0.14));
#52413=CARTESIAN_POINT('',(0.637233593757499,-0.128192616740993,0.74));
#52414=CARTESIAN_POINT('',(0.637233593757499,-0.128192616740993,0.39));
#52415=CARTESIAN_POINT('',(0.610580806867569,-0.107661870153497,0.14));
#52416=CARTESIAN_POINT('',(0.672315344701812,-0.155216227497267,0.14));
#52417=CARTESIAN_POINT('',(0.610580806867569,-0.107661870153497,0.74));
#52418=CARTESIAN_POINT('',(0.610580806867569,-0.107661870153497,0.74));
#52419=CARTESIAN_POINT('',(0.672315344701812,-0.155216227497267,0.74));
#52420=CARTESIAN_POINT('Origin',(0.647718825750041,-0.119653037223409,0.74));
#52421=CARTESIAN_POINT('',(0.642648162921854,-0.0974850690781231,0.74));
#52422=CARTESIAN_POINT('Origin',(0.,0.,0.74));
#52423=CARTESIAN_POINT('',(0.610580806867569,-0.107661870153497,0.74));
#52424=CARTESIAN_POINT('Origin',(0.610580806867569,-0.107661870153497,0.74));
#52425=CARTESIAN_POINT('',(0.642648162921854,-0.0974850690781231,0.14));
#52426=CARTESIAN_POINT('',(0.642648162921854,-0.0974850690781231,0.39));
#52427=CARTESIAN_POINT('',(0.610580806867569,-0.107661870153497,0.14));
#52428=CARTESIAN_POINT('Origin',(0.647718825750041,-0.119653037223409,0.14));
#52429=CARTESIAN_POINT('Origin',(0.,0.,0.14));
#52430=CARTESIAN_POINT('Origin',(0.34,0.,-4.5));
#52431=CARTESIAN_POINT('',(-0.34,-4.163799117101E-17,-4.5));
#52432=CARTESIAN_POINT('Origin',(0.,0.,-4.5));
#52433=CARTESIAN_POINT('Origin',(0.,0.,-4.47));
#52434=CARTESIAN_POINT('',(-0.37,-4.53119315684521E-17,-4.47));
#52435=CARTESIAN_POINT('Origin',(0.,0.,0.02));
#52436=CARTESIAN_POINT('',(-0.65,-7.9602041944578E-17,0.04));
#52437=CARTESIAN_POINT('Origin',(0.,0.,0.04));
#52438=CARTESIAN_POINT('',(-0.63,-7.71527483462833E-17,0.02));
#52439=CARTESIAN_POINT('Origin',(0.,0.,0.39));
#52440=CARTESIAN_POINT('Origin',(0.,0.,0.74));
#52441=CARTESIAN_POINT('Origin',(0.,0.,0.74));
#52442=CARTESIAN_POINT('Origin',(0.,0.,0.74));
#52443=CARTESIAN_POINT('Origin',(0.,0.,0.74));
#52444=CARTESIAN_POINT('Origin',(0.,0.,0.74));
#52445=CARTESIAN_POINT('Origin',(0.,0.,0.74));
#52446=CARTESIAN_POINT('Origin',(0.,0.,0.74));
#52447=CARTESIAN_POINT('Origin',(0.,0.,0.74));
#52448=CARTESIAN_POINT('Origin',(0.,0.,0.74));
#52449=CARTESIAN_POINT('Origin',(0.,0.,0.74));
#52450=CARTESIAN_POINT('Origin',(0.,0.,0.74));
#52451=CARTESIAN_POINT('Origin',(0.,0.,0.74));
#52452=CARTESIAN_POINT('Origin',(0.,0.,0.74));
#52453=CARTESIAN_POINT('Origin',(0.,0.,0.74));
#52454=CARTESIAN_POINT('Origin',(0.,0.,0.74));
#52455=CARTESIAN_POINT('Origin',(0.,0.,0.74));
#52456=CARTESIAN_POINT('',(-0.65,-7.9602041944578E-17,0.39));
#52457=CARTESIAN_POINT('Origin',(0.,0.,0.74));
#52458=CARTESIAN_POINT('Origin',(0.,0.,0.74));
#52459=CARTESIAN_POINT('Origin',(0.,0.,0.74));
#52460=CARTESIAN_POINT('Origin',(0.,0.,0.74));
#52461=CARTESIAN_POINT('Origin',(0.,0.,0.74));
#52462=CARTESIAN_POINT('Origin',(0.,0.,0.74));
#52463=CARTESIAN_POINT('Origin',(0.,0.,0.74));
#52464=CARTESIAN_POINT('Origin',(0.,0.,0.74));
#52465=CARTESIAN_POINT('Origin',(0.,0.,0.74));
#52466=CARTESIAN_POINT('Origin',(0.,0.,0.74));
#52467=CARTESIAN_POINT('Origin',(0.,0.,0.74));
#52468=CARTESIAN_POINT('Origin',(0.,0.,0.74));
#52469=CARTESIAN_POINT('Origin',(0.,0.,0.74));
#52470=CARTESIAN_POINT('Origin',(0.,0.,0.74));
#52471=CARTESIAN_POINT('Origin',(0.,0.,0.74));
#52472=CARTESIAN_POINT('Origin',(0.,0.,0.74));
#52473=CARTESIAN_POINT('Origin',(0.,0.,0.74));
#52474=CARTESIAN_POINT('Origin',(0.,0.,0.74));
#52475=CARTESIAN_POINT('Origin',(0.,0.,0.74));
#52476=CARTESIAN_POINT('Origin',(0.,0.,0.74));
#52477=CARTESIAN_POINT('Origin',(0.,0.,0.77));
#52478=CARTESIAN_POINT('',(-0.59,-7.22541611496939E-17,0.8));
#52479=CARTESIAN_POINT('Origin',(0.,0.,0.8));
#52480=CARTESIAN_POINT('',(-0.62,-7.59281015471359E-17,0.77));
#52481=CARTESIAN_POINT('Origin',(0.,0.,0.8));
#52482=CARTESIAN_POINT('',(0.,0.,0.));
#52483=CARTESIAN_POINT('Origin',(0.,0.,-1.33003901172249));
#52484=CARTESIAN_POINT('',(-0.747455179358203,1.21560254385408E-5,-0.193723222248809));
#52485=CARTESIAN_POINT('',(-0.747444078220075,-6.40459137768446E-6,-0.187197830382769));
#52486=CARTESIAN_POINT('',(-0.7475,-1.95907305151415E-14,-1.33003901172249));
#52487=CARTESIAN_POINT('',(0.708694801171171,0.237542783106672,-0.12));
#52488=CARTESIAN_POINT('Ctrl Pts',(-0.747455179358203,1.21560254385013E-5,
-0.193723222248809));
#52489=CARTESIAN_POINT('Ctrl Pts',(-0.747409043365026,-0.0764700511820665,
-0.191546603424788));
#52490=CARTESIAN_POINT('Ctrl Pts',(-0.717056524628226,-0.275197846725086,
-0.185891997066607));
#52491=CARTESIAN_POINT('Ctrl Pts',(-0.543630981761295,-0.556730447339991,
-0.176759403174265));
#52492=CARTESIAN_POINT('Ctrl Pts',(-0.217353554555276,-0.747156946739449,
-0.166325440571785));
#52493=CARTESIAN_POINT('Ctrl Pts',(0.160155550638935,-0.76146581913925,
-0.155891477969304));
#52494=CARTESIAN_POINT('Ctrl Pts',(0.499915663487163,-0.596301280456369,
-0.145457515366823));
#52495=CARTESIAN_POINT('Ctrl Pts',(0.721838643854927,-0.290560778341026,
-0.135023552764342));
#52496=CARTESIAN_POINT('Ctrl Pts',(0.763953513632067,0.0137597889773751,
-0.126537714308735));
#52497=CARTESIAN_POINT('Ctrl Pts',(0.725795582116321,0.186572354342488,
-0.121529863387288));
#52498=CARTESIAN_POINT('Ctrl Pts',(0.708694801171171,0.237542783106672,
-0.12));
#52499=CARTESIAN_POINT('',(0.747395528060274,0.0124969850565577,-0.12));
#52500=CARTESIAN_POINT('Origin',(0.,0.,-0.12));
#52501=CARTESIAN_POINT('Ctrl Pts',(-0.747444078220075,-6.40459137771915E-6,
-0.187197830382769));
#52502=CARTESIAN_POINT('Ctrl Pts',(-0.747460394071194,-0.0538175344429418,
-0.185666478793474));
#52503=CARTESIAN_POINT('Ctrl Pts',(-0.728699568742348,-0.229832596850165,
-0.180657139670018));
#52504=CARTESIAN_POINT('Ctrl Pts',(-0.591963456523637,-0.50503391867701,
-0.172169813012403));
#52505=CARTESIAN_POINT('Ctrl Pts',(-0.284343786563672,-0.724320025643111,
-0.161735850409922));
#52506=CARTESIAN_POINT('Ctrl Pts',(0.0903167314019248,-0.772864465068914,
-0.151301887807442));
#52507=CARTESIAN_POINT('Ctrl Pts',(0.443652359236502,-0.639262442637615,
-0.140867925204961));
#52508=CARTESIAN_POINT('Ctrl Pts',(0.692489824641793,-0.354929918130671,
-0.130433962602481));
#52509=CARTESIAN_POINT('Ctrl Pts',(0.749438361810143,-0.109676867461668,
-0.12347798753416));
#52510=CARTESIAN_POINT('Ctrl Pts',(0.747395528060274,0.0124969850565577,
-0.12));
#52511=CARTESIAN_POINT('Origin',(0.,0.,-1.33003901172249));
#52512=CARTESIAN_POINT('',(-0.747444051384665,-6.42748184076532E-6,-0.327407432775125));
#52513=CARTESIAN_POINT('',(-0.747492032740272,-1.77696257386839E-5,-0.320882040909085));
#52514=CARTESIAN_POINT('',(-0.7475,-1.95907305151415E-14,-1.33003901172249));
#52515=CARTESIAN_POINT('Ctrl Pts',(-0.747444051384665,-6.42748184076503E-6,
-0.327407432775125));
#52516=CARTESIAN_POINT('Ctrl Pts',(-0.747460735268479,-0.0535655898421423,
-0.325883248386414));
#52517=CARTESIAN_POINT('Ctrl Pts',(-0.728815731862444,-0.229328242581179,
-0.320881076463544));
#52518=CARTESIAN_POINT('Ctrl Pts',(-0.592475727944838,-0.504436944883217,
-0.312400917006513));
#52519=CARTESIAN_POINT('Ctrl Pts',(-0.285071300054302,-0.724029331642761,
-0.301966954404033));
#52520=CARTESIAN_POINT('Ctrl Pts',(0.0895271131383138,-0.772961199617316,
-0.291532991801552));
#52521=CARTESIAN_POINT('Ctrl Pts',(0.443023143994609,-0.639698844990302,
-0.281099029199071));
#52522=CARTESIAN_POINT('Ctrl Pts',(0.692094455558162,-0.355653462496763,
-0.270665066596591));
#52523=CARTESIAN_POINT('Ctrl Pts',(0.778032597283113,0.0122227909580791,
-0.26023110399411));
#52524=CARTESIAN_POINT('Ctrl Pts',(0.68058114334938,0.377218004776167,-0.249797141391629));
#52525=CARTESIAN_POINT('Ctrl Pts',(0.42271031352139,0.65329941426342,-0.239363178789149));
#52526=CARTESIAN_POINT('Ctrl Pts',(0.0652026943778764,0.775391960536891,
-0.228929216186668));
#52527=CARTESIAN_POINT('Ctrl Pts',(-0.307673823063886,0.714717431064047,
-0.218495253584187));
#52528=CARTESIAN_POINT('Ctrl Pts',(-0.608028707877244,0.485577090895009,
-0.208061290981707));
#52529=CARTESIAN_POINT('Ctrl Pts',(-0.732306246915873,0.213659075752667,
-0.199803947203247));
#52530=CARTESIAN_POINT('Ctrl Pts',(-0.747482763396928,0.045739754373763,
-0.195024590958948));
#52531=CARTESIAN_POINT('Ctrl Pts',(-0.747455179358203,1.21560254385013E-5,
-0.193723222248809));
#52532=CARTESIAN_POINT('Ctrl Pts',(-0.747492032740272,-1.77696257387602E-5,
-0.320882040909085));
#52533=CARTESIAN_POINT('Ctrl Pts',(-0.747521461794713,-0.0308968347335454,
-0.3200031237551));
#52534=CARTESIAN_POINT('Ctrl Pts',(-0.738208053524619,-0.183950674319056,
-0.315646219066955));
#52535=CARTESIAN_POINT('Ctrl Pts',(-0.635857117988054,-0.448519615362855,
-0.307811326844651));
#52536=CARTESIAN_POINT('Ctrl Pts',(-0.349675784487414,-0.695133774103566,
-0.29737736424217));
#52537=CARTESIAN_POINT('Ctrl Pts',(0.0189274157531999,-0.777898369643473,
-0.28694340163969));
#52538=CARTESIAN_POINT('Ctrl Pts',(0.383069251609923,-0.677305003145055,
-0.276509439037209));
#52539=CARTESIAN_POINT('Ctrl Pts',(0.656918053157327,-0.417064487823471,
-0.266075476434728));
#52540=CARTESIAN_POINT('Ctrl Pts',(0.775925115315039,-0.0585179376441868,
-0.255641513832248));
#52541=CARTESIAN_POINT('Ctrl Pts',(0.712039292365906,0.313821812003498,
-0.245207551229767));
#52542=CARTESIAN_POINT('Ctrl Pts',(0.480319196218488,0.612190866640268,
-0.234773588627287));
#52543=CARTESIAN_POINT('Ctrl Pts',(0.135383189993233,0.766260668703223,
-0.224339626024806));
#52544=CARTESIAN_POINT('Ctrl Pts',(-0.24146359128836,0.739715845333337,
-0.213905663422326));
#52545=CARTESIAN_POINT('Ctrl Pts',(-0.561395755032477,0.538812615893194,
-0.203471700819845));
#52546=CARTESIAN_POINT('Ctrl Pts',(-0.721466439761006,0.259032440630972,
-0.194569089806659));
#52547=CARTESIAN_POINT('Ctrl Pts',(-0.747423337703997,0.0683976642946505,
-0.189144466327634));
#52548=CARTESIAN_POINT('Ctrl Pts',(-0.747444078220075,-6.40459137771915E-6,
-0.187197830382769));
#52549=CARTESIAN_POINT('Origin',(0.,0.,-1.33003901172249));
#52550=CARTESIAN_POINT('',(-0.747492771866375,-1.77854026473198E-5,-0.461091643301441));
#52551=CARTESIAN_POINT('',(-0.747552914013562,-7.59237280051339E-6,-0.4545662514354));
#52552=CARTESIAN_POINT('',(-0.7475,-1.95907305151415E-14,-1.33003901172249));
#52553=CARTESIAN_POINT('Ctrl Pts',(-0.747492771866375,-1.7785402647276E-5,
-0.461091643301441));
#52554=CARTESIAN_POINT('Ctrl Pts',(-0.747522042549812,-0.030644957535598,
-0.460219893348041));
#52555=CARTESIAN_POINT('Ctrl Pts',(-0.738300189612616,-0.183446679313347,
-0.455870155860481));
#52556=CARTESIAN_POINT('Ctrl Pts',(-0.636310057828864,-0.447876802013019,
-0.448042430838761));
#52557=CARTESIAN_POINT('Ctrl Pts',(-0.350378094607062,-0.694780044542988,
-0.43760846823628));
#52558=CARTESIAN_POINT('Ctrl Pts',(0.018141279213836,-0.777917099351843,
-0.4271745056338));
#52559=CARTESIAN_POINT('Ctrl Pts',(0.382384582988471,-0.677691781098527,
-0.416740543031318));
#52560=CARTESIAN_POINT('Ctrl Pts',(0.656496245978099,-0.417728139454391,
-0.406306580428839));
#52561=CARTESIAN_POINT('Ctrl Pts',(0.775865572452268,-0.0593020485231031,
-0.395872617826358));
#52562=CARTESIAN_POINT('Ctrl Pts',(0.712356090039248,0.313102092711016,
-0.385438655223878));
#52563=CARTESIAN_POINT('Ctrl Pts',(0.480937580760017,0.611705127399059,
-0.375004692621396));
#52564=CARTESIAN_POINT('Ctrl Pts',(0.136157562681009,0.766123513283346,
-0.364570730018916));
#52565=CARTESIAN_POINT('Ctrl Pts',(-0.240716072858239,0.739959385191355,
-0.354136767416435));
#52566=CARTESIAN_POINT('Ctrl Pts',(-0.560850667196372,0.539379874112091,
-0.343702804813955));
#52567=CARTESIAN_POINT('Ctrl Pts',(-0.721333836132676,0.259535992032645,
-0.334793026600185));
#52568=CARTESIAN_POINT('Ctrl Pts',(-0.747422664848419,0.0686493471490352,
-0.329361235920575));
#52569=CARTESIAN_POINT('Ctrl Pts',(-0.747444051384665,-6.42748184076503E-6,
-0.327407432775125));
#52570=CARTESIAN_POINT('Ctrl Pts',(-0.747552914013563,-7.59237280050992E-6,
-0.4545662514354));
#52571=CARTESIAN_POINT('Ctrl Pts',(-0.747557174200554,-0.0079627541396081,
-0.454339768716727));
#52572=CARTESIAN_POINT('Ctrl Pts',(-0.745521898301695,-0.13807937304922,
-0.450635298463893));
#52573=CARTESIAN_POINT('Ctrl Pts',(-0.674371225051021,-0.388210728933227,
-0.443452840676899));
#52574=CARTESIAN_POINT('Ctrl Pts',(-0.412054943730932,-0.660071846531001,
-0.433018878074418));
#52575=CARTESIAN_POINT('Ctrl Pts',(-0.052613438684712,-0.776347824950466,
-0.422584915471938));
#52576=CARTESIAN_POINT('Ctrl Pts',(0.319229548446942,-0.709631323036312,
-0.412150952869457));
#52577=CARTESIAN_POINT('Ctrl Pts',(0.615827130120364,-0.475648047450975,
-0.401716990266977));
#52578=CARTESIAN_POINT('Ctrl Pts',(0.767268468189366,-0.129550055793595,
-0.391283027664495));
#52579=CARTESIAN_POINT('Ctrl Pts',(0.73785741566876,0.247084101843196,-0.380849065062015));
#52580=CARTESIAN_POINT('Ctrl Pts',(0.53452643409528,0.565478213973466,-0.370415102459534));
#52581=CARTESIAN_POINT('Ctrl Pts',(0.205202547258297,0.750583795355784,
-0.359981139857054));
#52582=CARTESIAN_POINT('Ctrl Pts',(-0.172489509004575,0.758769720339227,
-0.349547177254573));
#52583=CARTESIAN_POINT('Ctrl Pts',(-0.509524166428119,0.588106489551374,
-0.339113214652092));
#52584=CARTESIAN_POINT('Ctrl Pts',(-0.708185410677575,0.304874056256311,
-0.329558169203597));
#52585=CARTESIAN_POINT('Ctrl Pts',(-0.747405007264241,0.0912955733046984,
-0.323481111289261));
#52586=CARTESIAN_POINT('Ctrl Pts',(-0.747492032740272,-1.77696257387602E-5,
-0.320882040909085));
#52587=CARTESIAN_POINT('Origin',(0.,0.,-1.33003901172249));
#52588=CARTESIAN_POINT('',(-0.747553321122147,-7.36938303809654E-6,-0.594775853827757));
#52589=CARTESIAN_POINT('',(-0.747538056636855,1.30170342584265E-5,-0.588250461961717));
#52590=CARTESIAN_POINT('',(-0.7475,-1.95907305151415E-14,-1.33003901172249));
#52591=CARTESIAN_POINT('Ctrl Pts',(-0.747553321122147,-7.36938303808141E-6,
-0.594775853827757));
#52592=CARTESIAN_POINT('Ctrl Pts',(-0.74755734320473,-0.0077107724177583,
-0.594556538309668));
#52593=CARTESIAN_POINT('Ctrl Pts',(-0.745590310689939,-0.137575565048743,
-0.590859235257418));
#52594=CARTESIAN_POINT('Ctrl Pts',(-0.674763198638609,-0.387529025027267,
-0.583683944671009));
#52595=CARTESIAN_POINT('Ctrl Pts',(-0.412721788492083,-0.659655095318369,
-0.573249982068528));
#52596=CARTESIAN_POINT('Ctrl Pts',(-0.0533979730410179,-0.776294258609907,
-0.562816019466048));
#52597=CARTESIAN_POINT('Ctrl Pts',(0.318512246619034,-0.709953567657271,
-0.552382056863567));
#52598=CARTESIAN_POINT('Ctrl Pts',(0.615346135603011,-0.476270146948171,
-0.541948094261087));
#52599=CARTESIAN_POINT('Ctrl Pts',(0.767137155915032,-0.130325375465359,
-0.531514131658606));
#52600=CARTESIAN_POINT('Ctrl Pts',(0.738106737168653,0.246338312127523,
-0.521080169056125));
#52601=CARTESIAN_POINT('Ctrl Pts',(0.535097621960437,0.564937743869073,
-0.510646206453644));
#52602=CARTESIAN_POINT('Ctrl Pts',(0.205960967115317,0.750376038730258,
-0.500212243851164));
#52603=CARTESIAN_POINT('Ctrl Pts',(-0.171722623797879,0.758943647414989,
-0.489778281248683));
#52604=CARTESIAN_POINT('Ctrl Pts',(-0.508929578017626,0.588621104017168,
-0.479344318646203));
#52605=CARTESIAN_POINT('Ctrl Pts',(-0.708026179252435,0.305377277568611,
-0.469782105997121));
#52606=CARTESIAN_POINT('Ctrl Pts',(-0.747405262420699,0.0915471027788979,
-0.463697880882201));
#52607=CARTESIAN_POINT('Ctrl Pts',(-0.747492771866375,-1.7785402647276E-5,
-0.461091643301441));
#52608=CARTESIAN_POINT('Ctrl Pts',(-0.747538056636855,1.30170342584213E-5,
-0.588250461961717));
#52609=CARTESIAN_POINT('Ctrl Pts',(-0.747449782311828,-0.107195335869156,
-0.585198426144193));
#52610=CARTESIAN_POINT('Ctrl Pts',(-0.697538394050389,-0.336653954873882,
-0.578668402792509));
#52611=CARTESIAN_POINT('Ctrl Pts',(-0.470949408769063,-0.619427779176754,
-0.568660391906666));
#52612=CARTESIAN_POINT('Ctrl Pts',(-0.123709349589915,-0.768231811408391,
-0.558226429304186));
#52613=CARTESIAN_POINT('Ctrl Pts',(0.25269016620706,-0.735956383991622,
-0.547792466701704));
#52614=CARTESIAN_POINT('Ctrl Pts',(0.569528234436074,-0.530209118571064,
-0.537358504099225));
#52615=CARTESIAN_POINT('Ctrl Pts',(0.752123144005562,-0.199486579716445,
-0.526924541496743));
#52616=CARTESIAN_POINT('Ctrl Pts',(0.757435558261681,0.178256821234392,
-0.516490578894263));
#52617=CARTESIAN_POINT('Ctrl Pts',(0.58421329122536,0.513983413731815,-0.506056616291782));
#52618=CARTESIAN_POINT('Ctrl Pts',(0.273286459598611,0.728559283954183,
-0.495622653689302));
#52619=CARTESIAN_POINT('Ctrl Pts',(-0.102056559562228,0.771406882187409,
-0.485188691086821));
#52620=CARTESIAN_POINT('Ctrl Pts',(-0.453343888260037,0.632426626742619,
-0.47475472848434));
#52621=CARTESIAN_POINT('Ctrl Pts',(-0.692468131949326,0.350629951601094,
-0.464547248600534));
#52622=CARTESIAN_POINT('Ctrl Pts',(-0.74749175253247,0.114200886509029,
-0.457817756250887));
#52623=CARTESIAN_POINT('Ctrl Pts',(-0.747552914013563,-7.59237280050992E-6,
-0.4545662514354));
#52624=CARTESIAN_POINT('Origin',(0.,0.,-1.33003901172249));
#52625=CARTESIAN_POINT('',(-0.747537418840408,1.3179381549518E-5,-0.728460064354072));
#52626=CARTESIAN_POINT('',(-0.747472643624562,1.62103417219173E-5,-0.721934672488032));
#52627=CARTESIAN_POINT('',(-0.7475,-1.95907305151415E-14,-1.33003901172249));
#52628=CARTESIAN_POINT('Ctrl Pts',(-0.747537418840409,1.31793815494937E-5,
-0.728460064354072));
#52629=CARTESIAN_POINT('Ctrl Pts',(-0.747448558105652,-0.106943676944281,
-0.725415195737134));
#52630=CARTESIAN_POINT('Ctrl Pts',(-0.697716187447847,-0.336151536347626,
-0.718892339586036));
#52631=CARTESIAN_POINT('Ctrl Pts',(-0.471575149406303,-0.618951531170264,
-0.708891495900775));
#52632=CARTESIAN_POINT('Ctrl Pts',(-0.124485645778937,-0.768106401138926,
-0.698457533298296));
#52633=CARTESIAN_POINT('Ctrl Pts',(0.251946294775518,-0.736211371838604,
-0.688023570695814));
#52634=CARTESIAN_POINT('Ctrl Pts',(0.568992125251127,-0.530784401501963,
-0.677589608093334));
#52635=CARTESIAN_POINT('Ctrl Pts',(0.751921163041749,-0.200246558136551,
-0.667155645490854));
#52636=CARTESIAN_POINT('Ctrl Pts',(0.757615314330881,0.177491281382813,
-0.656721682888373));
#52637=CARTESIAN_POINT('Ctrl Pts',(0.584732414132277,0.513392757388173,
-0.646287720285892));
#52638=CARTESIAN_POINT('Ctrl Pts',(0.274022587194117,0.728282734371093,
-0.635853757683412));
#52639=CARTESIAN_POINT('Ctrl Pts',(-0.101276939472307,0.771509624701283,
-0.625419795080931));
#52640=CARTESIAN_POINT('Ctrl Pts',(-0.452704539459636,0.632884443977122,
-0.61498583247845));
#52641=CARTESIAN_POINT('Ctrl Pts',(-0.69228154043425,0.351131872468849,
-0.604771185394059));
#52642=CARTESIAN_POINT('Ctrl Pts',(-0.747493559514422,0.114452674833002,
-0.598034525843828));
#52643=CARTESIAN_POINT('Ctrl Pts',(-0.747553321122147,-7.36938303808141E-6,
-0.594775853827757));
#52644=CARTESIAN_POINT('Ctrl Pts',(-0.747472643624562,1.62103417219207E-5,
-0.721934672488032));
#52645=CARTESIAN_POINT('Ctrl Pts',(-0.747402612221546,-0.0842954619945286,
-0.71953507110582));
#52646=CARTESIAN_POINT('Ctrl Pts',(-0.712499566770546,-0.290865199736192,
-0.713657482189446));
#52647=CARTESIAN_POINT('Ctrl Pts',(-0.525861117638762,-0.573545293931952,
-0.704301905738914));
#52648=CARTESIAN_POINT('Ctrl Pts',(-0.19375906706945,-0.753618964174968,
-0.693867943136433));
#52649=CARTESIAN_POINT('Ctrl Pts',(0.184013817024176,-0.756057560229359,
-0.683433980533953));
#52650=CARTESIAN_POINT('Ctrl Pts',(0.518412914638575,-0.580286282081279,
-0.673000017931471));
#52651=CARTESIAN_POINT('Ctrl Pts',(0.73061721497504,-0.267736072313561,
-0.662566055328992));
#52652=CARTESIAN_POINT('Ctrl Pts',(0.770608169635336,0.107922046529214,
-0.65213209272651));
#52653=CARTESIAN_POINT('Ctrl Pts',(0.628959534674377,0.458141924492801,
-0.641698130124031));
#52654=CARTESIAN_POINT('Ctrl Pts',(0.339059224908709,0.700373444128261,
-0.631264167521549));
#52655=CARTESIAN_POINT('Ctrl Pts',(-0.0307605314660725,0.777520359180196,
-0.620830204919069));
#52656=CARTESIAN_POINT('Ctrl Pts',(-0.393329741412475,0.671398416557689,
-0.610396242316588));
#52657=CARTESIAN_POINT('Ctrl Pts',(-0.663187433844336,0.407021555727386,
-0.599962279714107));
#52658=CARTESIAN_POINT('Ctrl Pts',(-0.74351458894893,0.152101734785077,
-0.592580352929151));
#52659=CARTESIAN_POINT('Ctrl Pts',(-0.747550376479258,0.0149753519108104,
-0.588676413678354));
#52660=CARTESIAN_POINT('Ctrl Pts',(-0.747538056636855,1.30170342584213E-5,
-0.588250461961717));
#52661=CARTESIAN_POINT('Origin',(0.,0.,-1.33003901172249));
#52662=CARTESIAN_POINT('',(-0.747472002174667,1.61159471936687E-5,-0.862144274880388));
#52663=CARTESIAN_POINT('',(-0.747440403350747,2.49991181755504E-7,-0.855618883014348));
#52664=CARTESIAN_POINT('',(-0.7475,-1.95907305151415E-14,-1.33003901172249));
#52665=CARTESIAN_POINT('Ctrl Pts',(-0.747472002174667,1.61159471936886E-5,
-0.862144274880388));
#52666=CARTESIAN_POINT('Ctrl Pts',(-0.747402682287736,-0.0840439390973357,
-0.85975184069876));
#52667=CARTESIAN_POINT('Ctrl Pts',(-0.712650382827926,-0.290361716183336,
-0.853881418982972));
#52668=CARTESIAN_POINT('Ctrl Pts',(-0.526440462347929,-0.573013576696856,
-0.844533009733024));
#52669=CARTESIAN_POINT('Ctrl Pts',(-0.194520560057908,-0.753422770554805,
-0.834099047130543));
#52670=CARTESIAN_POINT('Ctrl Pts',(0.183249666810382,-0.756243134903882,
-0.823665084528063));
#52671=CARTESIAN_POINT('Ctrl Pts',(0.517826224589069,-0.580809883355641,
-0.813231121925582));
#52672=CARTESIAN_POINT('Ctrl Pts',(0.730346273449163,-0.268474282445114,
-0.802797159323102));
#52673=CARTESIAN_POINT('Ctrl Pts',(0.770716840097935,0.107143230607854,
-0.79236319672062));
#52674=CARTESIAN_POINT('Ctrl Pts',(0.62942220247575,0.457506077015547,-0.781929234118141));
#52675=CARTESIAN_POINT('Ctrl Pts',(0.339766834898864,0.700030440322706,
-0.77149527151566));
#52676=CARTESIAN_POINT('Ctrl Pts',(-0.0299747696136753,0.777551048267701,
-0.761061308913179));
#52677=CARTESIAN_POINT('Ctrl Pts',(-0.392651039152919,0.671795564831833,
-0.750627346310698));
#52678=CARTESIAN_POINT('Ctrl Pts',(-0.66277576768029,0.4076915516066,-0.740193383708219));
#52679=CARTESIAN_POINT('Ctrl Pts',(-0.743438739207482,0.152605612016255,
-0.732804289722676));
#52680=CARTESIAN_POINT('Ctrl Pts',(-0.747550058881758,0.0152273129384325,
-0.728893183271294));
#52681=CARTESIAN_POINT('Ctrl Pts',(-0.747537418840409,1.31793815494937E-5,
-0.728460064354072));
#52682=CARTESIAN_POINT('Ctrl Pts',(-0.747440403350747,2.49991181772852E-7,
-0.855618883014348));
#52683=CARTESIAN_POINT('Ctrl Pts',(-0.747439664227336,-0.0613952789202318,
-0.853871716067446));
#52684=CARTESIAN_POINT('Ctrl Pts',(-0.725057127938405,-0.245007983420982,
-0.848646561586384));
#52685=CARTESIAN_POINT('Ctrl Pts',(-0.576325689361536,-0.522812412838008,
-0.839943419571161));
#52686=CARTESIAN_POINT('Ctrl Pts',(-0.262170190030731,-0.732632862145289,
-0.829509456968681));
#52687=CARTESIAN_POINT('Ctrl Pts',(0.113781287599417,-0.769764858789943,
-0.8190754943662));
#52688=CARTESIAN_POINT('Ctrl Pts',(0.462913446150841,-0.625456042107333,
-0.808641531763721));
#52689=CARTESIAN_POINT('Ctrl Pts',(0.702932553865032,-0.333721356752229,
-0.798207569161239));
#52690=CARTESIAN_POINT('Ctrl Pts',(0.77726385077405,0.036674589509254,-0.787773606558759));
#52691=CARTESIAN_POINT('Ctrl Pts',(0.668386751451238,0.398425990267,-0.777339643956278));
#52692=CARTESIAN_POINT('Ctrl Pts',(0.401964611697131,0.666264639748313,
-0.766905681353797));
#52693=CARTESIAN_POINT('Ctrl Pts',(0.0407956343310049,0.777058450475451,
-0.756471718751316));
#52694=CARTESIAN_POINT('Ctrl Pts',(-0.329989257542916,0.704692279751986,
-0.746037756148837));
#52695=CARTESIAN_POINT('Ctrl Pts',(-0.622992579377318,0.466223514289631,
-0.735603793546355));
#52696=CARTESIAN_POINT('Ctrl Pts',(-0.735537269423189,0.197977738940191,
-0.727569432326088));
#52697=CARTESIAN_POINT('Ctrl Pts',(-0.747504115891487,0.0379060617849304,
-0.72301305863998));
#52698=CARTESIAN_POINT('Ctrl Pts',(-0.747472643624562,1.62103417219207E-5,
-0.721934672488032));
#52699=CARTESIAN_POINT('Origin',(0.,0.,-1.33003901172249));
#52700=CARTESIAN_POINT('',(-0.747440394010334,2.88097105794361E-8,-0.995828485406704));
#52701=CARTESIAN_POINT('',(-0.747471187093045,-1.59917937688492E-5,-0.989303093540664));
#52702=CARTESIAN_POINT('',(-0.7475,-1.95907305151415E-14,-1.33003901172249));
#52703=CARTESIAN_POINT('Ctrl Pts',(-0.747440394010334,2.88097105755059E-8,
-0.995828485406704));
#52704=CARTESIAN_POINT('Ctrl Pts',(-0.747440305752118,-0.0611436444929975,
-0.994088485660387));
#52705=CARTESIAN_POINT('Ctrl Pts',(-0.725182114079541,-0.244504027566075,
-0.98887049837991));
#52706=CARTESIAN_POINT('Ctrl Pts',(-0.576853733233579,-0.522229725565813,
-0.980174523565272));
#52707=CARTESIAN_POINT('Ctrl Pts',(-0.262910442753169,-0.732367543071951,
-0.969740560962791));
#52708=CARTESIAN_POINT('Ctrl Pts',(0.113003322331731,-0.769879451565163,
-0.95930659836031));
#52709=CARTESIAN_POINT('Ctrl Pts',(0.462281136078411,-0.625923533367173,
-0.948872635757831));
#52710=CARTESIAN_POINT('Ctrl Pts',(0.70259494345804,-0.334431555819595,
-0.938438673155348));
#52711=CARTESIAN_POINT('Ctrl Pts',(0.777300516433144,0.0358890839459567,
-0.928004710552869));
#52712=CARTESIAN_POINT('Ctrl Pts',(0.668789051521525,0.397750328889645,
-0.917570747950388));
#52713=CARTESIAN_POINT('Ctrl Pts',(0.402637719871012,0.665858082479752,
-0.907136785347908));
#52714=CARTESIAN_POINT('Ctrl Pts',(0.0415808928872875,0.777016826591824,
-0.896702822745427));
#52715=CARTESIAN_POINT('Ctrl Pts',(-0.32927694153081,0.705025400441648,
-0.886268860142946));
#52716=CARTESIAN_POINT('Ctrl Pts',(-0.622521105437113,0.466852859850313,
-0.875834897540466));
#52717=CARTESIAN_POINT('Ctrl Pts',(-0.735437461077155,0.198481764760452,
-0.867793369119613));
#52718=CARTESIAN_POINT('Ctrl Pts',(-0.747503455677645,0.038157886060821,
-0.86322982823292));
#52719=CARTESIAN_POINT('Ctrl Pts',(-0.747472002174667,1.61159471936886E-5,
-0.862144274880388));
#52720=CARTESIAN_POINT('Ctrl Pts',(-0.747471187093045,-1.59917937688908E-5,
-0.989303093540664));
#52721=CARTESIAN_POINT('Ctrl Pts',(-0.747502606642687,-0.0384803988601513,
-0.988208361029073));
#52722=CARTESIAN_POINT('Ctrl Pts',(-0.735309243690986,-0.199127278369172,
-0.983635640983321));
#52723=CARTESIAN_POINT('Ctrl Pts',(-0.621916351700691,-0.467658178639452,
-0.97558493340341));
#52724=CARTESIAN_POINT('Ctrl Pts',(-0.328364174807744,-0.705450981188053,
-0.965150970800929));
#52725=CARTESIAN_POINT('Ctrl Pts',(0.0425865250681738,-0.776962359283856,
-0.954717008198449));
#52726=CARTESIAN_POINT('Ctrl Pts',(0.403499180542324,-0.665336403825433,
-0.944283045595967));
#52727=CARTESIAN_POINT('Ctrl Pts',(0.669303286159026,-0.396884404409992,
-0.933849082993487));
#52728=CARTESIAN_POINT('Ctrl Pts',(0.777346315469045,-0.0348830195569247,
-0.923415120391007));
#52729=CARTESIAN_POINT('Ctrl Pts',(0.702161510858138,0.335340620697414,
-0.912981157788526));
#52730=CARTESIAN_POINT('Ctrl Pts',(0.461470637519424,0.626521324425116,
-0.902547195186045));
#52731=CARTESIAN_POINT('Ctrl Pts',(0.112006796904718,0.770025062366403,
-0.892113232583565));
#52732=CARTESIAN_POINT('Ctrl Pts',(-0.26385809865297,0.732026654580473,
-0.881679269981084));
#52733=CARTESIAN_POINT('Ctrl Pts',(-0.577529159980992,0.521482682939164,
-0.871245307378604));
#52734=CARTESIAN_POINT('Ctrl Pts',(-0.72534176137517,0.243858607071591,
-0.862558511723024));
#52735=CARTESIAN_POINT('Ctrl Pts',(-0.747441135558977,0.0608213670538153,
-0.857349703601606));
#52736=CARTESIAN_POINT('Ctrl Pts',(-0.747440403350747,2.49991181772852E-7,
-0.855618883014348));
#52737=CARTESIAN_POINT('Origin',(0.,0.,-1.33003901172249));
#52738=CARTESIAN_POINT('',(-0.7475,-1.95907305151415E-14,-1.12625));
#52739=CARTESIAN_POINT('',(-0.747536615034749,-1.54000427277645E-5,-1.12298730406698));
#52740=CARTESIAN_POINT('',(-0.7475,-1.95907305151415E-14,-1.33003901172249));
#52741=CARTESIAN_POINT('',(-0.738728321778978,-0.114178441930227,-1.12625));
#52742=CARTESIAN_POINT('Origin',(0.,0.,-1.12625));
#52743=CARTESIAN_POINT('Ctrl Pts',(-0.738728321778979,-0.114178441930225,
-1.12625));
#52744=CARTESIAN_POINT('Ctrl Pts',(-0.720064014057808,-0.234935499803312,
-1.12277201246584));
#52745=CARTESIAN_POINT('Ctrl Pts',(-0.622428467720147,-0.467011987146758,
-1.11581603739752));
#52746=CARTESIAN_POINT('Ctrl Pts',(-0.329058176975973,-0.705127368582215,
-1.10538207479504));
#52747=CARTESIAN_POINT('Ctrl Pts',(0.0417919283474016,-0.77700066177415,
-1.09494811219256));
#52748=CARTESIAN_POINT('Ctrl Pts',(0.402831360764571,-0.66574603450436,
-1.08451414959008));
#52749=CARTESIAN_POINT('Ctrl Pts',(0.66889944257465,-0.397559467050142,
-1.0740801869876));
#52750=CARTESIAN_POINT('Ctrl Pts',(0.77731189566657,-0.0356691406410475,
-1.06364622438512));
#52751=CARTESIAN_POINT('Ctrl Pts',(0.70249941623784,0.334631148448006,-1.05321226178264));
#52752=CARTESIAN_POINT('Ctrl Pts',(0.462103868983754,0.626054505003761,
-1.04277829918016));
#52753=CARTESIAN_POINT('Ctrl Pts',(0.112784749994043,0.769911552166373,
-1.03234433657767));
#52754=CARTESIAN_POINT('Ctrl Pts',(-0.263118110857165,0.732292892594137,
-1.02191037397519));
#52755=CARTESIAN_POINT('Ctrl Pts',(-0.577001907123833,0.522066075167691,
-1.01147641137271));
#52756=CARTESIAN_POINT('Ctrl Pts',(-0.725217128854169,0.244362557690023,
-1.00278244851655));
#52757=CARTESIAN_POINT('Ctrl Pts',(-0.747440482166499,0.061073001796564,
-0.997566473194547));
#52758=CARTESIAN_POINT('Ctrl Pts',(-0.747440394010334,2.88097105755059E-8,
-0.995828485406704));
#52759=CARTESIAN_POINT('Ctrl Pts',(-0.747536615034749,-1.54000427278131E-5,
-1.12298730406698));
#52760=CARTESIAN_POINT('Ctrl Pts',(-0.747549574643972,-0.0155531187576153,
-1.1225450059907));
#52761=CARTESIAN_POINT('Ctrl Pts',(-0.743340401009098,-0.153262521212314,
-1.11862472038026));
#52762=CARTESIAN_POINT('Ctrl Pts',(-0.662248238305512,-0.408538693637006,
-1.11122644723566));
#52763=CARTESIAN_POINT('Ctrl Pts',(-0.391780881856498,-0.672308433025162,
-1.10079248463318));
#52764=CARTESIAN_POINT('Ctrl Pts',(-0.0289685614302447,-0.77758653236944,
-1.0903585220307));
#52765=CARTESIAN_POINT('Ctrl Pts',(0.340672665444815,-0.699591456600573,
-1.07992455942822));
#52766=CARTESIAN_POINT('Ctrl Pts',(0.630013764781798,-0.45669036663525,
-1.06949059682573));
#52767=CARTESIAN_POINT('Ctrl Pts',(0.770854889346007,-0.106145976774946,
-1.05905663422326));
#52768=CARTESIAN_POINT('Ctrl Pts',(0.72999817257357,0.269419497799126,-1.04862267162077));
#52769=CARTESIAN_POINT('Ctrl Pts',(0.517074073818034,0.581479511865617,
-1.03818870901829));
#52770=CARTESIAN_POINT('Ctrl Pts',(0.182270729955259,0.756479721113076,
-1.02775474641581));
#52771=CARTESIAN_POINT('Ctrl Pts',(-0.195495525574089,0.753170354596227,
-1.01732078381333));
#52772=CARTESIAN_POINT('Ctrl Pts',(-0.527181654493514,0.572331754114927,
-1.00688682121085));
#52773=CARTESIAN_POINT('Ctrl Pts',(-0.712843111741135,0.28971688006118,
-0.997547591119962));
#52774=CARTESIAN_POINT('Ctrl Pts',(-0.747402786092163,0.0837218074955242,
-0.991686348563233));
#52775=CARTESIAN_POINT('Ctrl Pts',(-0.747471187093045,-1.59917937688908E-5,
-0.989303093540664));
#52776=CARTESIAN_POINT('Origin',(0.,0.,1.095));
#52777=CARTESIAN_POINT('',(-0.792490573374725,2.00326525206102E-5,0.848268682536521));
#52778=CARTESIAN_POINT('',(-0.792490189019743,1.3140117316485E-5,0.826731317463479));
#52779=CARTESIAN_POINT('',(-0.7925,-9.70532588324277E-17,1.095));
#52780=CARTESIAN_POINT('',(0.345478907940192,0.713232482552815,0.8));
#52781=CARTESIAN_POINT('Ctrl Pts',(-0.792490573374725,2.00326525206102E-5,
0.848268682536521));
#52782=CARTESIAN_POINT('Ctrl Pts',(-0.792523353183581,0.0333301751535281,
0.847265264173584));
#52783=CARTESIAN_POINT('Ctrl Pts',(-0.790462051371192,0.0666362775783571,
0.846261845810648));
#52784=CARTESIAN_POINT('Ctrl Pts',(-0.786274148538905,0.0996727818564752,
0.845258427447711));
#52785=CARTESIAN_POINT('Ctrl Pts',(-0.769804202821169,0.22959686413684,
0.841312240864219));
#52786=CARTESIAN_POINT('Ctrl Pts',(-0.720443250858591,0.355351215356187,
0.837366054280727));
#52787=CARTESIAN_POINT('Ctrl Pts',(-0.644137104498692,0.461788800755913,
0.833419867697236));
#52788=CARTESIAN_POINT('Ctrl Pts',(-0.567830958138792,0.568226386155639,
0.829473681113744));
#52789=CARTESIAN_POINT('Ctrl Pts',(-0.46457961738157,0.655347205735744,
0.825527494530252));
#52790=CARTESIAN_POINT('Ctrl Pts',(-0.346820261793125,0.712655533465586,
0.821581307946761));
#52791=CARTESIAN_POINT('Ctrl Pts',(-0.229060906204681,0.769963861195427,
0.817635121363269));
#52792=CARTESIAN_POINT('Ctrl Pts',(-0.0967935357850139,0.797459697075005,
0.813688934779777));
#52793=CARTESIAN_POINT('Ctrl Pts',(0.0340494680202196,0.791834055085671,
0.809742748196285));
#52794=CARTESIAN_POINT('Ctrl Pts',(0.141728988687317,0.787204335381606,
0.80649516546419));
#52795=CARTESIAN_POINT('Ctrl Pts',(0.248443821076452,0.760142257936812,
0.803247582732095));
#52796=CARTESIAN_POINT('Ctrl Pts',(0.345504974425202,0.713245911452251,
0.8));
#52797=CARTESIAN_POINT('',(-0.345478907940189,0.713232482552817,0.8));
#52798=CARTESIAN_POINT('Origin',(0.,0.,0.8));
#52799=CARTESIAN_POINT('Ctrl Pts',(-0.345478907940187,0.713232482552818,
0.8));
#52800=CARTESIAN_POINT('Ctrl Pts',(-0.463374437871894,0.656125690688751,
0.803946186583492));
#52801=CARTESIAN_POINT('Ctrl Pts',(-0.56678182300553,0.569256548592082,
0.807892373166983));
#52802=CARTESIAN_POINT('Ctrl Pts',(-0.64328331919897,0.462978698222646,
0.811838559750475));
#52803=CARTESIAN_POINT('Ctrl Pts',(-0.719784815392412,0.356700847853208,
0.815784746333967));
#52804=CARTESIAN_POINT('Ctrl Pts',(-0.769380422645657,0.231014289211002,
0.819730932917459));
#52805=CARTESIAN_POINT('Ctrl Pts',(-0.786090265814568,0.101114707806154,
0.823677119500951));
#52806=CARTESIAN_POINT('Ctrl Pts',(-0.790401192991213,0.0676022666627898,
0.82469518548846));
#52807=CARTESIAN_POINT('Ctrl Pts',(-0.792523327817215,0.0338094174993378,
0.82571325147597));
#52808=CARTESIAN_POINT('Ctrl Pts',(-0.792490189019743,1.3140117316485E-5,
0.826731317463479));
#52809=CARTESIAN_POINT('Origin',(0.,0.,1.095));
#52810=CARTESIAN_POINT('',(-0.792556380474703,-9.7200913266593E-6,0.99826868253652));
#52811=CARTESIAN_POINT('',(-0.792557287165952,-9.28448389212729E-6,0.97673131746348));
#52812=CARTESIAN_POINT('',(-0.7925,-9.70532588324277E-17,1.095));
#52813=CARTESIAN_POINT('Ctrl Pts',(-0.792556380474703,-9.7200913266593E-6,
0.99826868253652));
#52814=CARTESIAN_POINT('Ctrl Pts',(-0.792481403648174,0.121101794392974,
0.994619503175485));
#52815=CARTESIAN_POINT('Ctrl Pts',(-0.764293771819342,0.242247017684031,
0.99097032381445));
#52816=CARTESIAN_POINT('Ctrl Pts',(-0.710683845299557,0.350842060800447,
0.987321144453415));
#52817=CARTESIAN_POINT('Ctrl Pts',(-0.652710599305326,0.468275669779912,
0.983374957869923));
#52818=CARTESIAN_POINT('Ctrl Pts',(-0.565008404019093,0.571033039869338,
0.979428771286432));
#52819=CARTESIAN_POINT('Ctrl Pts',(-0.458141477682844,0.646736473330992,
0.97548258470294));
#52820=CARTESIAN_POINT('Ctrl Pts',(-0.351274551346596,0.722439906792646,
0.971536398119448));
#52821=CARTESIAN_POINT('Ctrl Pts',(-0.225242893960332,0.771089403626528,
0.967590211535957));
#52822=CARTESIAN_POINT('Ctrl Pts',(-0.0952277211006728,0.786824860355167,
0.963644024952465));
#52823=CARTESIAN_POINT('Ctrl Pts',(0.0347874517589859,0.802560317083806,
0.959697838368973));
#52824=CARTESIAN_POINT('Ctrl Pts',(0.168786140092041,0.785381733707203,
0.955751651785481));
#52825=CARTESIAN_POINT('Ctrl Pts',(0.290627455022684,0.737358367191763,
0.951805465201989));
#52826=CARTESIAN_POINT('Ctrl Pts',(0.412468769953327,0.689335000676323,
0.947859278618497));
#52827=CARTESIAN_POINT('Ctrl Pts',(0.522152711481559,0.610466851022046,
0.943913092035006));
#52828=CARTESIAN_POINT('Ctrl Pts',(0.606467237537711,0.510254024749504,
0.939966905451514));
#52829=CARTESIAN_POINT('Ctrl Pts',(0.690781763593864,0.410041198476962,
0.936020718868022));
#52830=CARTESIAN_POINT('Ctrl Pts',(0.749726874177938,0.288483695586154,
0.93207453228453));
#52831=CARTESIAN_POINT('Ctrl Pts',(0.776202302140517,0.16022379814418,0.928128345701038));
#52832=CARTESIAN_POINT('Ctrl Pts',(0.802677730103097,0.0319639007022064,
0.924182159117547));
#52833=CARTESIAN_POINT('Ctrl Pts',(0.796683475444182,-0.102998391290932,
0.920235972534055));
#52834=CARTESIAN_POINT('Ctrl Pts',(0.758941579632242,-0.228406124124693,
0.916289785950564));
#52835=CARTESIAN_POINT('Ctrl Pts',(0.7211996838203,-0.353813856958455,0.912343599367072));
#52836=CARTESIAN_POINT('Ctrl Pts',(0.651710146855333,-0.469667030632837,
0.908397412783579));
#52837=CARTESIAN_POINT('Ctrl Pts',(0.558843370603139,-0.562010471638567,
0.904451226200087));
#52838=CARTESIAN_POINT('Ctrl Pts',(0.465976594350946,-0.654353912644296,
0.900505039616596));
#52839=CARTESIAN_POINT('Ctrl Pts',(0.349732578811529,-0.723187620981374,
0.896558853033105));
#52840=CARTESIAN_POINT('Ctrl Pts',(0.224113563887374,-0.760220218573038,
0.892612666449613));
#52841=CARTESIAN_POINT('Ctrl Pts',(0.0984945489632185,-0.797252816164703,
0.888666479866121));
#52842=CARTESIAN_POINT('Ctrl Pts',(-0.0364994653456741,-0.802484303010954,
0.884720293282628));
#52843=CARTESIAN_POINT('Ctrl Pts',(-0.164607698271848,-0.775284466464064,
0.880774106699137));
#52844=CARTESIAN_POINT('Ctrl Pts',(-0.292715931198022,-0.748084629917174,
0.876827920115645));
#52845=CARTESIAN_POINT('Ctrl Pts',(-0.413938382741478,-0.688453469977143,
0.872881733532154));
#52846=CARTESIAN_POINT('Ctrl Pts',(-0.513673131666121,-0.60357399285205,
0.868935546948662));
#52847=CARTESIAN_POINT('Ctrl Pts',(-0.613407880590764,-0.518694515726958,
0.86498936036517));
#52848=CARTESIAN_POINT('Ctrl Pts',(-0.691654926896594,-0.408566721416806,
0.861043173781678));
#52849=CARTESIAN_POINT('Ctrl Pts',(-0.738988980313063,-0.286455917591038,
0.857096987198186));
#52850=CARTESIAN_POINT('Ctrl Pts',(-0.774287146073082,-0.195394893160973,
0.854154218977631));
#52851=CARTESIAN_POINT('Ctrl Pts',(-0.792394438618434,-0.0976700559435039,
0.851211450757076));
#52852=CARTESIAN_POINT('Ctrl Pts',(-0.792490573374725,2.00326525206102E-5,
0.848268682536521));
#52853=CARTESIAN_POINT('Ctrl Pts',(-0.792490189019743,1.3140117316485E-5,
0.826731317463479));
#52854=CARTESIAN_POINT('Ctrl Pts',(-0.792394876538436,-0.0971903585595296,
0.829659438059461));
#52855=CARTESIAN_POINT('Ctrl Pts',(-0.774470502847006,-0.194422216474874,
0.832587558655444));
#52856=CARTESIAN_POINT('Ctrl Pts',(-0.739514560452847,-0.285092406647597,
0.835515679251426));
#52857=CARTESIAN_POINT('Ctrl Pts',(-0.69240493283764,-0.407287335529011,
0.839461865834918));
#52858=CARTESIAN_POINT('Ctrl Pts',(-0.61436159852265,-0.517564589124346,
0.843408052418409));
#52859=CARTESIAN_POINT('Ctrl Pts',(-0.514783468555716,-0.602628892990279,
0.847354239001901));
#52860=CARTESIAN_POINT('Ctrl Pts',(-0.415205338588783,-0.687693196856211,
0.851300425585393));
#52861=CARTESIAN_POINT('Ctrl Pts',(-0.294092412969906,-0.74754455099274,
0.855246612168885));
#52862=CARTESIAN_POINT('Ctrl Pts',(-0.166034353688321,-0.774979445676994,
0.859192798752377));
#52863=CARTESIAN_POINT('Ctrl Pts',(-0.0379762944067349,-0.802414340361247,
0.863138985335869));
#52864=CARTESIAN_POINT('Ctrl Pts',(0.0970268985375597,-0.797432775593224,
0.867085171919361));
#52865=CARTESIAN_POINT('Ctrl Pts',(0.222713811041056,-0.760631818600032,
0.871031358502853));
#52866=CARTESIAN_POINT('Ctrl Pts',(0.348400723544551,-0.723830861606839,
0.874977545086344));
#52867=CARTESIAN_POINT('Ctrl Pts',(0.464771355607247,-0.655210512388478,
0.878923731669835));
#52868=CARTESIAN_POINT('Ctrl Pts',(0.55780797689814,-0.563037985744865,
0.882869918253327));
#52869=CARTESIAN_POINT('Ctrl Pts',(0.650844598189034,-0.470865459101252,
0.886816104836819));
#52870=CARTESIAN_POINT('Ctrl Pts',(0.720547208708123,-0.355140755032387,
0.890762291420312));
#52871=CARTESIAN_POINT('Ctrl Pts',(0.758519861389888,-0.229802795205853,
0.894708478003803));
#52872=CARTESIAN_POINT('Ctrl Pts',(0.796492514071653,-0.104464835379319,
0.898654664587295));
#52873=CARTESIAN_POINT('Ctrl Pts',(0.802735208916092,0.0304863802048845,
0.902600851170786));
#52874=CARTESIAN_POINT('Ctrl Pts',(0.77649591743639,0.158794839290955,0.906547037754278));
#52875=CARTESIAN_POINT('Ctrl Pts',(0.750256625956688,0.287103298377025,
0.910493224337769));
#52876=CARTESIAN_POINT('Ctrl Pts',(0.691535348152843,0.408769000964962,
0.914439410921262));
#52877=CARTESIAN_POINT('Ctrl Pts',(0.607405420110863,0.509136830275265,
0.918385597504753));
#52878=CARTESIAN_POINT('Ctrl Pts',(0.523275492068883,0.609504659585568,
0.922331784088245));
#52879=CARTESIAN_POINT('Ctrl Pts',(0.413736913788769,0.688574615618236,
0.926277970671737));
#52880=CARTESIAN_POINT('Ctrl Pts',(0.29198420193571,0.736822182783594,0.930224157255229));
#52881=CARTESIAN_POINT('Ctrl Pts',(0.170231490082652,0.785069749948953,
0.93417034383872));
#52882=CARTESIAN_POINT('Ctrl Pts',(0.0362646446566508,0.802494928247001,
0.938116530422213));
#52883=CARTESIAN_POINT('Ctrl Pts',(-0.093779273240774,0.786998807714651,
0.942062717005704));
#52884=CARTESIAN_POINT('Ctrl Pts',(-0.2238231911382,0.771502687182301,0.946008903589196));
#52885=CARTESIAN_POINT('Ctrl Pts',(-0.34994418150705,0.723085267819551,
0.949955090172688));
#52886=CARTESIAN_POINT('Ctrl Pts',(-0.456950272099103,0.647578672431404,
0.953901276756179));
#52887=CARTESIAN_POINT('Ctrl Pts',(-0.563956362691155,0.572072077043258,
0.957847463339671));
#52888=CARTESIAN_POINT('Ctrl Pts',(-0.65184755350641,0.469476305629716,
0.961793649923163));
#52889=CARTESIAN_POINT('Ctrl Pts',(-0.710036858724068,0.352149603432412,
0.965739836506655));
#52890=CARTESIAN_POINT('Ctrl Pts',(-0.764062572465559,0.243217922543028,
0.969403663492263));
#52891=CARTESIAN_POINT('Ctrl Pts',(-0.792484823565687,0.121587962456681,
0.973067490477871));
#52892=CARTESIAN_POINT('Ctrl Pts',(-0.792557287165952,-9.28448389212729E-6,
0.97673131746348));
#52893=CARTESIAN_POINT('Origin',(0.,0.,1.095));
#52894=CARTESIAN_POINT('',(-0.792443402549405,-1.07763833267771E-5,1.14826868253652));
#52895=CARTESIAN_POINT('',(-0.792444147951047,-1.11489312963033E-5,1.12673131746348));
#52896=CARTESIAN_POINT('',(-0.7925,-9.70532588324277E-17,1.095));
#52897=CARTESIAN_POINT('Ctrl Pts',(-0.792443402549405,-1.07763833267771E-5,
1.14826868253652));
#52898=CARTESIAN_POINT('Ctrl Pts',(-0.792405491575818,0.0779733200496504,
1.14591992876088));
#52899=CARTESIAN_POINT('Ctrl Pts',(-0.780968401909595,0.1559682971011,1.14357117498524));
#52900=CARTESIAN_POINT('Ctrl Pts',(-0.758294050000535,0.230546770333913,
1.14122242120959));
#52901=CARTESIAN_POINT('Ctrl Pts',(-0.720198433414051,0.355847503659272,
1.1372762346261));
#52902=CARTESIAN_POINT('Ctrl Pts',(-0.650382262731333,0.47150412689294,
1.13333004804261));
#52903=CARTESIAN_POINT('Ctrl Pts',(-0.557255284838512,0.563585155142655,
1.12938386145912));
#52904=CARTESIAN_POINT('Ctrl Pts',(-0.464128306945689,0.65566618339237,
1.12543767487563));
#52905=CARTESIAN_POINT('Ctrl Pts',(-0.347690521842762,0.724171616658134,
1.12149148829214));
#52906=CARTESIAN_POINT('Ctrl Pts',(-0.221967509722995,0.760849593681277,
1.11754530170864));
#52907=CARTESIAN_POINT('Ctrl Pts',(-0.0962444976032272,0.797527570704419,
1.11359911512515));
#52908=CARTESIAN_POINT('Ctrl Pts',(0.0387637415333804,0.802378091484939,
1.10965292854166));
#52909=CARTESIAN_POINT('Ctrl Pts',(0.16679471280093,0.774816883759842,1.10570674195817));
#52910=CARTESIAN_POINT('Ctrl Pts',(0.294825684068478,0.747255676034745,
1.10176055537468));
#52911=CARTESIAN_POINT('Ctrl Pts',(0.415879387466968,0.687282739804032,
1.09781436879119));
#52912=CARTESIAN_POINT('Ctrl Pts',(0.515374229717151,0.602122149502075,
1.09386818220769));
#52913=CARTESIAN_POINT('Ctrl Pts',(0.614869071967334,0.516961559200118,
1.0899219956242));
#52914=CARTESIAN_POINT('Ctrl Pts',(0.69280505306921,0.406613314826917,1.08597580904071));
#52915=CARTESIAN_POINT('Ctrl Pts',(0.739794349715095,0.284369477453707,
1.08202962245722));
#52916=CARTESIAN_POINT('Ctrl Pts',(0.78678364636098,0.162125640080496,1.07808343587373));
#52917=CARTESIAN_POINT('Ctrl Pts',(0.802826258550874,0.0279862097072739,
1.07413724929023));
#52918=CARTESIAN_POINT('Ctrl Pts',(0.785989764231391,-0.101890971637066,
1.07019106270674));
#52919=CARTESIAN_POINT('Ctrl Pts',(0.769153269911908,-0.231768152981406,
1.06624487612325));
#52920=CARTESIAN_POINT('Ctrl Pts',(0.719437669083049,-0.357383085296865,
1.06229868953976));
#52921=CARTESIAN_POINT('Ctrl Pts',(0.642831482959536,-0.463604749860529,
1.05835250295627));
#52922=CARTESIAN_POINT('Ctrl Pts',(0.566225296836024,-0.569826414424192,
1.05440631637278));
#52923=CARTESIAN_POINT('Ctrl Pts',(0.462728525417858,-0.656654811236061,
1.05046012978928));
#52924=CARTESIAN_POINT('Ctrl Pts',(0.344807931671896,-0.71363097594976,
1.04651394320579));
#52925=CARTESIAN_POINT('Ctrl Pts',(0.226887337925933,-0.770607140663459,
1.0425677566223));
#52926=CARTESIAN_POINT('Ctrl Pts',(0.0945429218521742,-0.79773107327899,
1.03862157003881));
#52927=CARTESIAN_POINT('Ctrl Pts',(-0.0362836939983929,-0.79173554494208,
1.03467538345532));
#52928=CARTESIAN_POINT('Ctrl Pts',(-0.167110309848962,-0.78574001660517,
1.03072919687183));
#52929=CARTESIAN_POINT('Ctrl Pts',(-0.296419125476338,-0.746625027315819,
1.02678301028833));
#52930=CARTESIAN_POINT('Ctrl Pts',(-0.4086341733228,-0.679102195530961,
1.02283682370484));
#52931=CARTESIAN_POINT('Ctrl Pts',(-0.52084922116926,-0.611579363746103,
1.01889063712135));
#52932=CARTESIAN_POINT('Ctrl Pts',(-0.615970501234805,-0.515648689465738,
1.01494445053786));
#52933=CARTESIAN_POINT('Ctrl Pts',(-0.682540125167227,-0.40286555711433,
1.01099826395437));
#52934=CARTESIAN_POINT('Ctrl Pts',(-0.74910974909965,-0.290082424762922,
1.00705207737087));
#52935=CARTESIAN_POINT('Ctrl Pts',(-0.787127716898949,-0.160446834340471,
1.00310589078738));
#52936=CARTESIAN_POINT('Ctrl Pts',(-0.792014552447484,-0.0295741151944942,
0.999159704203891));
#52937=CARTESIAN_POINT('Ctrl Pts',(-0.79238235701581,-0.0197240632553592,
0.998862696981434));
#52938=CARTESIAN_POINT('Ctrl Pts',(-0.792562482849181,-0.00986700332289492,
0.998565689758977));
#52939=CARTESIAN_POINT('Ctrl Pts',(-0.792556380474703,-9.7200913266593E-6,
0.99826868253652));
#52940=CARTESIAN_POINT('Ctrl Pts',(-0.792557287165952,-9.28448389212729E-6,
0.97673131746348));
#52941=CARTESIAN_POINT('Ctrl Pts',(-0.792562871707229,-0.00938040104719254,
0.977013677061363));
#52942=CARTESIAN_POINT('Ctrl Pts',(-0.792400078381659,-0.0187513233173363,
0.977296036659247));
#52943=CARTESIAN_POINT('Ctrl Pts',(-0.792067650133023,-0.0281162240255477,
0.97757839625713));
#52944=CARTESIAN_POINT('Ctrl Pts',(-0.787421716704263,-0.158997716305135,
0.981524582840622));
#52945=CARTESIAN_POINT('Ctrl Pts',(-0.749642430226683,-0.288703067883244,
0.985470769424114));
#52946=CARTESIAN_POINT('Ctrl Pts',(-0.683280515807775,-0.401608542979231,
0.989416956007606));
#52947=CARTESIAN_POINT('Ctrl Pts',(-0.616918601388867,-0.514514018075219,
0.993363142591098));
#52948=CARTESIAN_POINT('Ctrl Pts',(-0.521974059028629,-0.610619616689085,
0.997309329174589));
#52949=CARTESIAN_POINT('Ctrl Pts',(-0.409883488297753,-0.678348885460243,
1.00125551575808));
#52950=CARTESIAN_POINT('Ctrl Pts',(-0.297792917566875,-0.746078154231402,
1.00520170234157));
#52951=CARTESIAN_POINT('Ctrl Pts',(-0.16855631846536,-0.785431093159854,
1.00914788892507));
#52952=CARTESIAN_POINT('Ctrl Pts',(-0.0377409595363729,-0.791667420581768,
1.01309407550856));
#52953=CARTESIAN_POINT('Ctrl Pts',(0.0930743993926127,-0.797903748003683,
1.01704026209205));
#52954=CARTESIAN_POINT('Ctrl Pts',(0.225468518149069,-0.771023463919061,
1.02098644867554));
#52955=CARTESIAN_POINT('Ctrl Pts',(0.343493787150374,-0.714264448786606,
1.02493263525903));
#52956=CARTESIAN_POINT('Ctrl Pts',(0.461519056151679,-0.657505433654151,
1.02887882184252));
#52957=CARTESIAN_POINT('Ctrl Pts',(0.565175475397833,-0.570867687473863,
1.03282500842602));
#52958=CARTESIAN_POINT('Ctrl Pts',(0.641977051484891,-0.464787209444585,
1.03677119500951));
#52959=CARTESIAN_POINT('Ctrl Pts',(0.71877862757195,-0.358706731415306,
1.040717381593));
#52960=CARTESIAN_POINT('Ctrl Pts',(0.768725360499914,-0.233183521537036,
1.04466356817649));
#52961=CARTESIAN_POINT('Ctrl Pts',(0.785800887887494,-0.103337550163271,
1.04860975475998));
#52962=CARTESIAN_POINT('Ctrl Pts',(0.802876415275075,0.0265084212104935,
1.05255594134347));
#52963=CARTESIAN_POINT('Ctrl Pts',(0.787080737122274,0.160677154079753,
1.05650212792697));
#52964=CARTESIAN_POINT('Ctrl Pts',(0.740316530909984,0.283007276821933,
1.06044831451046));
#52965=CARTESIAN_POINT('Ctrl Pts',(0.693552324697694,0.405337399564113,
1.06439450109395));
#52966=CARTESIAN_POINT('Ctrl Pts',(0.615819590425917,0.515828912179213,
1.06834068767744));
#52967=CARTESIAN_POINT('Ctrl Pts',(0.516481669184491,0.601172496109797,
1.07228687426093));
#52968=CARTESIAN_POINT('Ctrl Pts',(0.417143747943065,0.686516080040382,
1.07623306084442));
#52969=CARTESIAN_POINT('Ctrl Pts',(0.296200639731992,0.74671173528645,1.08017924742792));
#52970=CARTESIAN_POINT('Ctrl Pts',(0.168220616025976,0.774508559681008,
1.08412543401141));
#52971=CARTESIAN_POINT('Ctrl Pts',(0.0402405923199609,0.802305384075567,
1.0880716205949));
#52972=CARTESIAN_POINT('Ctrl Pts',(-0.0947763468809948,0.797703377618616,
1.09201780717839));
#52973=CARTESIAN_POINT('Ctrl Pts',(-0.220566658720863,0.761256877630617,
1.09596399376188));
#52974=CARTESIAN_POINT('Ctrl Pts',(-0.34635697056073,0.724810377642619,
1.09991018034538));
#52975=CARTESIAN_POINT('Ctrl Pts',(-0.462920655039508,0.656519384123574,
1.10385636692887));
#52976=CARTESIAN_POINT('Ctrl Pts',(-0.556216966681838,0.564609927873067,
1.10780255351236));
#52977=CARTESIAN_POINT('Ctrl Pts',(-0.649513278324167,0.47270047162256,
1.11174874009585));
#52978=CARTESIAN_POINT('Ctrl Pts',(-0.719542217130047,0.35717255264059,
1.11569492667934));
#52979=CARTESIAN_POINT('Ctrl Pts',(-0.757868407107316,0.231942152673131,
1.11964111326283));
#52980=CARTESIAN_POINT('Ctrl Pts',(-0.780822256131107,0.156940705992757,
1.12200451466305));
#52981=CARTESIAN_POINT('Ctrl Pts',(-0.792404633700123,0.0784590725890344,
1.12436791606326));
#52982=CARTESIAN_POINT('Ctrl Pts',(-0.792444147951047,-1.11489312963033E-5,
1.12673131746348));
#52983=CARTESIAN_POINT('Origin',(0.,0.,1.095));
#52984=CARTESIAN_POINT('',(-0.792486097671081,1.97476927368961E-5,1.29826868253652));
#52985=CARTESIAN_POINT('',(-0.792484660449143,1.96714801883982E-5,1.27673131746348));
#52986=CARTESIAN_POINT('',(-0.7925,-9.70532588324277E-17,1.095));
#52987=CARTESIAN_POINT('Ctrl Pts',(-0.792486097671081,1.97476927368961E-5,
1.29826868253652));
#52988=CARTESIAN_POINT('Ctrl Pts',(-0.792519712746547,0.0348213055222317,
1.29722035434627));
#52989=CARTESIAN_POINT('Ctrl Pts',(-0.790269179267766,0.0696185478218366,
1.29617202615602));
#52990=CARTESIAN_POINT('Ctrl Pts',(-0.785699122793507,0.104108443553474,
1.29512369796577));
#52991=CARTESIAN_POINT('Ctrl Pts',(-0.76849621275801,0.233937599220784,
1.29117751138228));
#52992=CARTESIAN_POINT('Ctrl Pts',(-0.718426354171464,0.359411745751982,
1.28723132479879));
#52993=CARTESIAN_POINT('Ctrl Pts',(-0.641520740569973,0.465416822854705,
1.2832851382153));
#52994=CARTESIAN_POINT('Ctrl Pts',(-0.564615126968481,0.571421899957427,
1.27933895163181));
#52995=CARTESIAN_POINT('Ctrl Pts',(-0.460873758352043,0.657957907631675,
1.27539276504832));
#52996=CARTESIAN_POINT('Ctrl Pts',(-0.342792860783382,0.71460110143601,
1.27144657846482));
#52997=CARTESIAN_POINT('Ctrl Pts',(-0.224711963214721,0.771244295240344,
1.26750039188133));
#52998=CARTESIAN_POINT('Ctrl Pts',(-0.0922915366938353,0.797994675174765,
1.26355420529784));
#52999=CARTESIAN_POINT('Ctrl Pts',(0.0385176403463696,0.79163000888026,
1.25960801871435));
#53000=CARTESIAN_POINT('Ctrl Pts',(0.169326817386578,0.785265342585755,
1.25566183213086));
#53001=CARTESIAN_POINT('Ctrl Pts',(0.298524744946107,0.745785630062321,
1.25171564554737));
#53002=CARTESIAN_POINT('Ctrl Pts',(0.410548812552865,0.677946422727524,
1.24776945896387));
#53003=CARTESIAN_POINT('Ctrl Pts',(0.522572880159619,0.610107215392729,
1.24382327238038));
#53004=CARTESIAN_POINT('Ctrl Pts',(0.617423087813604,0.513908513246573,
1.23987708579689));
#53005=CARTESIAN_POINT('Ctrl Pts',(0.683674199345799,0.400937986135629,
1.2359308992134));
#53006=CARTESIAN_POINT('Ctrl Pts',(0.749925310877995,0.287967459024683,
1.2319847126299));
#53007=CARTESIAN_POINT('Ctrl Pts',(0.787577326288399,0.158225106948951,
1.22803852604641));
#53008=CARTESIAN_POINT('Ctrl Pts',(0.792094850463563,0.0273391193478977,
1.22409233946292));
#53009=CARTESIAN_POINT('Ctrl Pts',(0.796612374638728,-0.103546868253156,
1.22014615287943));
#53010=CARTESIAN_POINT('Ctrl Pts',(0.767995407578652,-0.235576491379531,
1.21619996629594));
#53011=CARTESIAN_POINT('Ctrl Pts',(0.709691022465244,-0.352846046045368,
1.21225377971245));
#53012=CARTESIAN_POINT('Ctrl Pts',(0.651386637351836,-0.470115600711205,
1.20830759312896));
#53013=CARTESIAN_POINT('Ctrl Pts',(0.563394834185097,-0.572625086916506,
1.20436140654546));
#53014=CARTESIAN_POINT('Ctrl Pts',(0.456314716087557,-0.648026665700992,
1.20041521996197));
#53015=CARTESIAN_POINT('Ctrl Pts',(0.349234597990017,-0.723428244485478,
1.19646903337848));
#53016=CARTESIAN_POINT('Ctrl Pts',(0.223066164961679,-0.771721915849148,
1.19252284679499));
#53017=CARTESIAN_POINT('Ctrl Pts',(0.0930071079731554,-0.787090437906651,
1.1885766602115));
#53018=CARTESIAN_POINT('Ctrl Pts',(-0.0370519490153704,-0.802458959964154,
1.184630473628));
#53019=CARTESIAN_POINT('Ctrl Pts',(-0.17100162996408,-0.784902332715489,
1.18068428704451));
#53020=CARTESIAN_POINT('Ctrl Pts',(-0.292706949220785,-0.736535349766373,
1.17673810046102));
#53021=CARTESIAN_POINT('Ctrl Pts',(-0.414412268477487,-0.688168366817258,
1.17279191387753));
#53022=CARTESIAN_POINT('Ctrl Pts',(-0.523873226042186,-0.608991028167693,
1.16884572729404));
#53023=CARTESIAN_POINT('Ctrl Pts',(-0.60790463948464,-0.508540685560815,
1.16489954071055));
#53024=CARTESIAN_POINT('Ctrl Pts',(-0.691936052927096,-0.408090342953935,
1.16095335412705));
#53025=CARTESIAN_POINT('Ctrl Pts',(-0.750537922247308,-0.28636699638974,
1.15700716754356));
#53026=CARTESIAN_POINT('Ctrl Pts',(-0.776651325662288,-0.158032901399117,
1.15306098096007));
#53027=CARTESIAN_POINT('Ctrl Pts',(-0.787222140411448,-0.106082723837479,
1.15146354815222));
#53028=CARTESIAN_POINT('Ctrl Pts',(-0.792469186534774,-0.0530492665922584,
1.14986611534437));
#53029=CARTESIAN_POINT('Ctrl Pts',(-0.792443402549405,-1.07763833267771E-5,
1.14826868253652));
#53030=CARTESIAN_POINT('Ctrl Pts',(-0.792444147951047,-1.11489312963033E-5,
1.12673131746348));
#53031=CARTESIAN_POINT('Ctrl Pts',(-0.79247061090012,-0.0525631631340214,
1.12831410264676));
#53032=CARTESIAN_POINT('Ctrl Pts',(-0.787320021835728,-0.105110059030113,
1.12989688783003));
#53033=CARTESIAN_POINT('Ctrl Pts',(-0.776940900150374,-0.15660307261215,
1.13147967301331));
#53034=CARTESIAN_POINT('Ctrl Pts',(-0.751063762067508,-0.284985016977022,
1.1354258595968));
#53035=CARTESIAN_POINT('Ctrl Pts',(-0.692686044753119,-0.406816024753814,
1.13937204618029));
#53036=CARTESIAN_POINT('Ctrl Pts',(-0.608839669631833,-0.507420872018991,
1.14331823276378));
#53037=CARTESIAN_POINT('Ctrl Pts',(-0.524993294510546,-0.608025719284169,
1.14726441934728));
#53038=CARTESIAN_POINT('Ctrl Pts',(-0.415678261582362,-0.68740440603773,
1.15121060593077));
#53039=CARTESIAN_POINT('Ctrl Pts',(-0.294062175841689,-0.735995327034944,
1.15515679251426));
#53040=CARTESIAN_POINT('Ctrl Pts',(-0.172446090101016,-0.784586248032158,
1.15910297909775));
#53041=CARTESIAN_POINT('Ctrl Pts',(-0.0385289515478548,-0.802389403273024,
1.16304916568124));
#53042=CARTESIAN_POINT('Ctrl Pts',(0.0915581740785099,-0.787260303481235,
1.16699535226474));
#53043=CARTESIAN_POINT('Ctrl Pts',(0.221645299704875,-0.772131203689446,
1.17094153884823));
#53044=CARTESIAN_POINT('Ctrl Pts',(0.347902412404443,-0.724069848865002,
1.17488772543172));
#53045=CARTESIAN_POINT('Ctrl Pts',(0.455121139245943,-0.648865497071205,
1.17883391201521));
#53046=CARTESIAN_POINT('Ctrl Pts',(0.562339866087442,-0.573661145277409,
1.1827800985987));
#53047=CARTESIAN_POINT('Ctrl Pts',(0.650520207070873,-0.471313796514261,
1.1867262851822));
#53048=CARTESIAN_POINT('Ctrl Pts',(0.709040348642845,-0.354151759383475,
1.19067247176569));
#53049=CARTESIAN_POINT('Ctrl Pts',(0.767560490214817,-0.236989722252689,
1.19461865834918));
#53050=CARTESIAN_POINT('Ctrl Pts',(0.796420432375329,-0.105012996754264,
1.19856484493267));
#53051=CARTESIAN_POINT('Ctrl Pts',(0.792143834237383,0.0258810849400756,
1.20251103151616));
#53052=CARTESIAN_POINT('Ctrl Pts',(0.787867236099438,0.156775166634416,
1.20645721809965));
#53053=CARTESIAN_POINT('Ctrl Pts',(0.750454097663033,0.286586604524672,
1.21040340468315));
#53054=CARTESIAN_POINT('Ctrl Pts',(0.684411039978694,0.39967888739995,1.21434959126664));
#53055=CARTESIAN_POINT('Ctrl Pts',(0.618367982294357,0.512771170275227,
1.21829577785013));
#53056=CARTESIAN_POINT('Ctrl Pts',(0.523695005362085,0.609144298135527,
1.22224196443362));
#53057=CARTESIAN_POINT('Ctrl Pts',(0.411795996922659,0.677189590584832,
1.22618815101711));
#53058=CARTESIAN_POINT('Ctrl Pts',(0.299896988483233,0.745234883034137,
1.2301343376006));
#53059=CARTESIAN_POINT('Ctrl Pts',(0.170771948536651,0.784952340072448,
1.2340805241841));
#53060=CARTESIAN_POINT('Ctrl Pts',(0.0399747078357781,0.791557772630288,
1.23802671076759));
#53061=CARTESIAN_POINT('Ctrl Pts',(-0.0908225328650967,0.798163205188129,
1.24197289735108));
#53062=CARTESIAN_POINT('Ctrl Pts',(-0.223291974320261,0.771656613265497,
1.24591908393457));
#53063=CARTESIAN_POINT('Ctrl Pts',(-0.341476933974791,0.715230863596611,
1.24986527051806));
#53064=CARTESIAN_POINT('Ctrl Pts',(-0.459661893629321,0.658805113927726,
1.25381145710156));
#53065=CARTESIAN_POINT('Ctrl Pts',(-0.563562371483215,0.572460206512586,
1.25775764368505));
#53066=CARTESIAN_POINT('Ctrl Pts',(-0.640662975879288,0.466596866701304,
1.26170383026854));
#53067=CARTESIAN_POINT('Ctrl Pts',(-0.717763580275359,0.360733526890024,
1.26565001685203));
#53068=CARTESIAN_POINT('Ctrl Pts',(-0.76806431121361,0.235351754682601,
1.26959620343552));
#53069=CARTESIAN_POINT('Ctrl Pts',(-0.785506165296385,0.105554483369243,
1.27354239001901));
#53070=CARTESIAN_POINT('Ctrl Pts',(-0.790204440115218,0.0705912708305541,
1.27460536583384));
#53071=CARTESIAN_POINT('Ctrl Pts',(-0.792518506333689,0.0353076739102088,
1.27566834164866));
#53072=CARTESIAN_POINT('Ctrl Pts',(-0.792484660449143,1.96714801883982E-5,
1.27673131746348));
#53073=CARTESIAN_POINT('Origin',(0.,0.,1.095));
#53074=CARTESIAN_POINT('',(-0.79255903846122,-8.36642852242164E-6,1.44826868253652));
#53075=CARTESIAN_POINT('',(-0.792559834217432,-7.91270320494323E-6,1.42673131746348));
#53076=CARTESIAN_POINT('',(-0.7925,-9.70532588324277E-17,1.095));
#53077=CARTESIAN_POINT('Ctrl Pts',(-0.79255903846122,-8.36642852242164E-6,
1.44826868253652));
#53078=CARTESIAN_POINT('Ctrl Pts',(-0.792492123018653,0.122592452217723,
1.44457459334817));
#53079=CARTESIAN_POINT('Ctrl Pts',(-0.763581778346857,0.245223739974001,
1.44088050415983));
#53080=CARTESIAN_POINT('Ctrl Pts',(-0.708692548810537,0.354847221826574,
1.43718641497148));
#53081=CARTESIAN_POINT('Ctrl Pts',(-0.650057488818566,0.471951788410097,
1.43324022838799));
#53082=CARTESIAN_POINT('Ctrl Pts',(-0.561776778393065,0.574212574410295,
1.42929404180449));
#53083=CARTESIAN_POINT('Ctrl Pts',(-0.454484321146134,0.649311698192748,
1.425347855221));
#53084=CARTESIAN_POINT('Ctrl Pts',(-0.347191863899205,0.7244108219752,1.42140166863751));
#53085=CARTESIAN_POINT('Ctrl Pts',(-0.220887659830848,0.772348283539907,
1.41745548205402));
#53086=CARTESIAN_POINT('Ctrl Pts',(-0.0907857542901829,0.787349748457175,
1.41350929547053));
#53087=CARTESIAN_POINT('Ctrl Pts',(0.0393161512504821,0.802351213374442,
1.40956310888704));
#53088=CARTESIAN_POINT('Ctrl Pts',(0.173215758263455,0.784416681644269,
1.40561692230354));
#53089=CARTESIAN_POINT('Ctrl Pts',(0.294784112781199,0.735706467573458,
1.40167073572005));
#53090=CARTESIAN_POINT('Ctrl Pts',(0.416352467298942,0.686996253502646,
1.39772454913656));
#53091=CARTESIAN_POINT('Ctrl Pts',(0.525589569321458,0.607510357091197,
1.39377836255307));
#53092=CARTESIAN_POINT('Ctrl Pts',(0.609337201066242,0.506823297584445,
1.38983217596958));
#53093=CARTESIAN_POINT('Ctrl Pts',(0.693084832811026,0.406136238077694,
1.38588598938608));
#53094=CARTESIAN_POINT('Ctrl Pts',(0.751342994278079,0.28424801547564,1.38193980280259));
#53095=CARTESIAN_POINT('Ctrl Pts',(0.777094165211017,0.155840745546875,
1.3779936162191));
#53096=CARTESIAN_POINT('Ctrl Pts',(0.802845336143955,0.02743347561811,1.37404742963561));
#53097=CARTESIAN_POINT('Ctrl Pts',(0.796089516542778,-0.107492841637366,
1.37010124305212));
#53098=CARTESIAN_POINT('Ctrl Pts',(0.757640482532682,-0.232685579280836,
1.36615505646863));
#53099=CARTESIAN_POINT('Ctrl Pts',(0.719191448522586,-0.357878316924306,
1.36220886988514));
#53100=CARTESIAN_POINT('Ctrl Pts',(0.649049200103572,-0.473337474955769,
1.35826268330164));
#53101=CARTESIAN_POINT('Ctrl Pts',(0.555662762042532,-0.565155354267195,
1.35431649671815));
#53102=CARTESIAN_POINT('Ctrl Pts',(0.46227632398149,-0.656973233578622,
1.35037031013466));
#53103=CARTESIAN_POINT('Ctrl Pts',(0.345645696278421,-0.725149834170012,
1.34642412355117));
#53104=CARTESIAN_POINT('Ctrl Pts',(0.219819688092605,-0.761472904511042,
1.34247793696768));
#53105=CARTESIAN_POINT('Ctrl Pts',(0.0939936799067887,-0.797795974852073,
1.33853175038418));
#53106=CARTESIAN_POINT('Ctrl Pts',(-0.0410277087617754,-0.802265514942745,
1.33458556380069));
#53107=CARTESIAN_POINT('Ctrl Pts',(-0.168980399092773,-0.77434314376771,
1.3306393772172));
#53108=CARTESIAN_POINT('Ctrl Pts',(-0.296933089423769,-0.746420772592674,
1.32669319063371));
#53109=CARTESIAN_POINT('Ctrl Pts',(-0.417817081417198,-0.686106490151933,
1.32274700405022));
#53110=CARTESIAN_POINT('Ctrl Pts',(-0.517071224478458,-0.600665487933144,
1.31880081746672));
#53111=CARTESIAN_POINT('Ctrl Pts',(-0.616325367539718,-0.515224485714355,
1.31485463088323));
#53112=CARTESIAN_POINT('Ctrl Pts',(-0.693949661668808,-0.404656763717519,
1.31090844429974));
#53113=CARTESIAN_POINT('Ctrl Pts',(-0.74059382799113,-0.282280820317389,
1.30696225771625));
#53114=CARTESIAN_POINT('Ctrl Pts',(-0.774846691106731,-0.192414782001653,
1.30406439932301));
#53115=CARTESIAN_POINT('Ctrl Pts',(-0.79239317664741,-0.0961810293084249,
1.30116654092976));
#53116=CARTESIAN_POINT('Ctrl Pts',(-0.792486097671081,1.97476927368961E-5,
1.29826868253652));
#53117=CARTESIAN_POINT('Ctrl Pts',(-0.792484660449143,1.96714801883982E-5,
1.27673131746348));
#53118=CARTESIAN_POINT('Ctrl Pts',(-0.792392857025736,-0.0956953459194891,
1.27961452823215));
#53119=CARTESIAN_POINT('Ctrl Pts',(-0.775027255054072,-0.191442775046391,
1.28249773900082));
#53120=CARTESIAN_POINT('Ctrl Pts',(-0.741112163299563,-0.280917151643365,
1.28538094976949));
#53121=CARTESIAN_POINT('Ctrl Pts',(-0.69469332999267,-0.40337874492332,
1.28932713635298));
#53122=CARTESIAN_POINT('Ctrl Pts',(-0.617272686151585,-0.514089161063939,
1.29327332293647));
#53123=CARTESIAN_POINT('Ctrl Pts',(-0.518175979838655,-0.599712713385525,
1.29721950951997));
#53124=CARTESIAN_POINT('Ctrl Pts',(-0.419079273525725,-0.685336265707111,
1.30116569610346));
#53125=CARTESIAN_POINT('Ctrl Pts',(-0.298306504740949,-0.745872954209667,
1.30511188268695));
#53126=CARTESIAN_POINT('Ctrl Pts',(-0.170405426623534,-0.774030797355784,
1.30905806927044));
#53127=CARTESIAN_POINT('Ctrl Pts',(-0.042504348506119,-0.802188640501901,
1.31300425585393));
#53128=CARTESIAN_POINT('Ctrl Pts',(0.0925250389439315,-0.79796763829158,
1.31695044243742));
#53129=CARTESIAN_POINT('Ctrl Pts',(0.218417693408498,-0.761876233967231,
1.32089662902092));
#53130=CARTESIAN_POINT('Ctrl Pts',(0.344310347873065,-0.725784829642882,
1.32484281560441));
#53131=CARTESIAN_POINT('Ctrl Pts',(0.461066269352145,-0.657823023204503,
1.3287890021879));
#53132=CARTESIAN_POINT('Ctrl Pts',(0.5546215563528,-0.566177193029512,1.33273518877139));
#53133=CARTESIAN_POINT('Ctrl Pts',(0.648176843353457,-0.474531362854518,
1.33668137535488));
#53134=CARTESIAN_POINT('Ctrl Pts',(0.718531495875688,-0.359201508942911,
1.34062756193837));
#53135=CARTESIAN_POINT('Ctrl Pts',(0.757210903894515,-0.234079755000792,
1.34457374852187));
#53136=CARTESIAN_POINT('Ctrl Pts',(0.795890311913341,-0.108958001058676,
1.34851993510536));
#53137=CARTESIAN_POINT('Ctrl Pts',(0.802894475428763,0.0259556529139527,
1.35246612168885));
#53138=CARTESIAN_POINT('Ctrl Pts',(0.777379703906943,0.15441010534137,1.35641230827234));
#53139=CARTESIAN_POINT('Ctrl Pts',(0.751864932385123,0.282864557768787,
1.36035849485583));
#53140=CARTESIAN_POINT('Ctrl Pts',(0.693831225826063,0.404859808650995,
1.36430468143932));
#53141=CARTESIAN_POINT('Ctrl Pts',(0.610269067641456,0.505700850066526,
1.36825086802282));
#53142=CARTESIAN_POINT('Ctrl Pts',(0.526706909456849,0.606541891482058,
1.37219705460631));
#53143=CARTESIAN_POINT('Ctrl Pts',(0.417616299646695,0.686228723430912,
1.3761432411898));
#53144=CARTESIAN_POINT('Ctrl Pts',(0.296137810190029,0.735162622862339,
1.38008942777329));
#53145=CARTESIAN_POINT('Ctrl Pts',(0.174659320733361,0.784096522293767,
1.38403561435679));
#53146=CARTESIAN_POINT('Ctrl Pts',(0.0407929516301808,0.802277489207765,
1.38798180094028));
#53147=CARTESIAN_POINT('Ctrl Pts',(-0.0893363468434648,0.78751552480611,
1.39192798752377));
#53148=CARTESIAN_POINT('Ctrl Pts',(-0.219465645317109,0.772753560404456,
1.39587417410726));
#53149=CARTESIAN_POINT('Ctrl Pts',(-0.345857873161221,0.725048664687147,
1.39982036069075));
#53150=CARTESIAN_POINT('Ctrl Pts',(-0.453288382072276,0.650147158231332,
1.40376654727424));
#53151=CARTESIAN_POINT('Ctrl Pts',(-0.56071889098333,0.575245651775519,
1.40771273385774));
#53152=CARTESIAN_POINT('Ctrl Pts',(-0.64918768096133,0.473147534581201,
1.41165892044123));
#53153=CARTESIAN_POINT('Ctrl Pts',(-0.708038193163794,0.356151093918478,
1.41560510702472));
#53154=CARTESIAN_POINT('Ctrl Pts',(-0.763347554859349,0.24619455808673,
1.41931384383764));
#53155=CARTESIAN_POINT('Ctrl Pts',(-0.792495780424916,0.123078679523467,
1.42302258065056));
#53156=CARTESIAN_POINT('Ctrl Pts',(-0.792559834217432,-7.91270320494323E-6,
1.42673131746348));
#53157=CARTESIAN_POINT('Origin',(0.,0.,1.095));
#53158=CARTESIAN_POINT('',(-0.792445760035067,-1.19013985881156E-5,1.59826868253652));
#53159=CARTESIAN_POINT('',(-0.792446584180059,-1.22568943931671E-5,1.57673131746348));
#53160=CARTESIAN_POINT('',(-0.7925,-9.70532588324277E-17,1.095));
#53161=CARTESIAN_POINT('Ctrl Pts',(-0.792445760035067,-1.19013985881156E-5,
1.59826868253652));
#53162=CARTESIAN_POINT('Ctrl Pts',(-0.792402924653838,0.079462628716892,
1.59587501893357));
#53163=CARTESIAN_POINT('Ctrl Pts',(-0.780517347576401,0.158949689219715,
1.59348135533061));
#53164=CARTESIAN_POINT('Ctrl Pts',(-0.756980882452868,0.234822535499662,
1.59108769172766));
#53165=CARTESIAN_POINT('Ctrl Pts',(-0.718178737164498,0.359906280630659,
1.58714150514417));
#53166=CARTESIAN_POINT('Ctrl Pts',(-0.647710969507546,0.475167054131685,
1.58319531856068));
#53167=CARTESIAN_POINT('Ctrl Pts',(-0.554065814855426,0.566721053417116,
1.57924913197718));
#53168=CARTESIAN_POINT('Ctrl Pts',(-0.460420660203306,0.658275052702546,
1.57530294539369));
#53169=CARTESIAN_POINT('Ctrl Pts',(-0.343598118556019,0.726122277772382,
1.5713567588102));
#53170=CARTESIAN_POINT('Ctrl Pts',(-0.217670116177076,0.762090152213681,
1.56741057222671));
#53171=CARTESIAN_POINT('Ctrl Pts',(-0.091742113798131,0.79805802665498,
1.56346438564321));
#53172=CARTESIAN_POINT('Ctrl Pts',(0.04329134931247,0.80214655046774,1.55951819905972));
#53173=CARTESIAN_POINT('Ctrl Pts',(0.171164739900571,0.773863238170921,
1.55557201247623));
#53174=CARTESIAN_POINT('Ctrl Pts',(0.299038130488669,0.745579925874101,
1.55162582589274));
#53175=CARTESIAN_POINT('Ctrl Pts',(0.419751448554267,0.684924777467703,
1.54767963930925));
#53176=CARTESIAN_POINT('Ctrl Pts',(0.51876410212864,0.5992040436448,1.54373345272576));
#53177=CARTESIAN_POINT('Ctrl Pts',(0.617776755703014,0.513483309821894,
1.53978726614226));
#53178=CARTESIAN_POINT('Ctrl Pts',(0.695088744786162,0.402696990582482,
1.53584107955877));
#53179=CARTESIAN_POINT('Ctrl Pts',(0.741387409386929,0.280189915557558,
1.53189489297528));
#53180=CARTESIAN_POINT('Ctrl Pts',(0.787686073987695,0.157682840532634,
1.52794870639179));
#53181=CARTESIAN_POINT('Ctrl Pts',(0.802971414106082,0.0234550097221994,
1.5240025198083));
#53182=CARTESIAN_POINT('Ctrl Pts',(0.78540222533046,-0.106325086520418,
1.52005633322481));
#53183=CARTESIAN_POINT('Ctrl Pts',(0.767833036554838,-0.236105182763034,
1.51611014664131));
#53184=CARTESIAN_POINT('Ctrl Pts',(0.717409318885208,-0.361437544437834,
1.51216396005782));
#53185=CARTESIAN_POINT('Ctrl Pts',(0.640204890156501,-0.467225190028658,
1.50821777347433));
#53186=CARTESIAN_POINT('Ctrl Pts',(0.563000461427793,-0.573012835619484,
1.50427158689084));
#53187=CARTESIAN_POINT('Ctrl Pts',(0.459015321640008,-0.659255765126335,
1.50032540030735));
#53188=CARTESIAN_POINT('Ctrl Pts',(0.340775060452138,-0.715565537006538,
1.49637921372386));
#53189=CARTESIAN_POINT('Ctrl Pts',(0.222534799264268,-0.77187530888674,
1.49243302714036));
#53190=CARTESIAN_POINT('Ctrl Pts',(0.0900394166763145,-0.798251923140294,
1.48848684055687));
#53191=CARTESIAN_POINT('Ctrl Pts',(-0.040751280002766,-0.791518169567666,
1.48454065397338));
#53192=CARTESIAN_POINT('Ctrl Pts',(-0.171541976681846,-0.784784415995039,
1.48059446738989));
#53193=CARTESIAN_POINT('Ctrl Pts',(-0.300627987452053,-0.74494029459623,
1.4766482808064));
#53194=CARTESIAN_POINT('Ctrl Pts',(-0.412460182842351,-0.676785251868913,
1.4727020942229));
#53195=CARTESIAN_POINT('Ctrl Pts',(-0.524292378232649,-0.608630209141596,
1.46875590763941));
#53196=CARTESIAN_POINT('Ctrl Pts',(-0.618870758243037,-0.512164245085771,
1.46480972105592));
#53197=CARTESIAN_POINT('Ctrl Pts',(-0.684802829859224,-0.399007222734641,
1.46086353447243));
#53198=CARTESIAN_POINT('Ctrl Pts',(-0.750734901475411,-0.285850200383513,
1.45691734788894));
#53199=CARTESIAN_POINT('Ctrl Pts',(-0.788020664697396,-0.15600211973708,
1.45297116130545));
#53200=CARTESIAN_POINT('Ctrl Pts',(-0.792168841529171,-0.0251039058304422,
1.44902497472195));
#53201=CARTESIAN_POINT('Ctrl Pts',(-0.792433842828974,-0.0167416304902463,
1.44877287732681));
#53202=CARTESIAN_POINT('Ctrl Pts',(-0.792563605001957,-0.00837506940927601,
1.44852077993166));
#53203=CARTESIAN_POINT('Ctrl Pts',(-0.79255903846122,-8.36642852242164E-6,
1.44826868253652));
#53204=CARTESIAN_POINT('Ctrl Pts',(-0.792559834217432,-7.91270320494323E-6,
1.42673131746348));
#53205=CARTESIAN_POINT('Ctrl Pts',(-0.792563935225162,-0.00788846194650599,
1.42696876723405));
#53206=CARTESIAN_POINT('Ctrl Pts',(-0.792448816490436,-0.0157688911413652,
1.42720621700462));
#53207=CARTESIAN_POINT('Ctrl Pts',(-0.792213710879083,-0.023645739006679,
1.42744366677519));
#53208=CARTESIAN_POINT('Ctrl Pts',(-0.788306481964977,-0.154551367137981,
1.43138985335869));
#53209=CARTESIAN_POINT('Ctrl Pts',(-0.751259789709837,-0.28446785926946,
1.43533603994218));
#53210=CARTESIAN_POINT('Ctrl Pts',(-0.685536114679231,-0.397746049821345,
1.43928222652567));
#53211=CARTESIAN_POINT('Ctrl Pts',(-0.619812439648625,-0.511024240373231,
1.44322841310916));
#53212=CARTESIAN_POINT('Ctrl Pts',(-0.525411781842551,-0.607664129345523,
1.44717459969265));
#53213=CARTESIAN_POINT('Ctrl Pts',(-0.413705226645241,-0.676024903479442,
1.45112078627615));
#53214=CARTESIAN_POINT('Ctrl Pts',(-0.301998671447931,-0.74438567761336,
1.45506697285964));
#53215=CARTESIAN_POINT('Ctrl Pts',(-0.172986218859384,-0.784467336908906,
1.45901315944313));
#53216=CARTESIAN_POINT('Ctrl Pts',(-0.0422081378576713,-0.791441822104801,
1.46295934602662));
#53217=CARTESIAN_POINT('Ctrl Pts',(0.0885699431440433,-0.798416307300696,
1.46690553261011));
#53218=CARTESIAN_POINT('Ctrl Pts',(0.221113652558924,-0.772283618396939,
1.4708517191936));
#53219=CARTESIAN_POINT('Ctrl Pts',(0.339457361842355,-0.716191583425139,
1.4747979057771));
#53220=CARTESIAN_POINT('Ctrl Pts',(0.457801071125785,-0.660099548453339,
1.47874409236059));
#53221=CARTESIAN_POINT('Ctrl Pts',(0.561944780277766,-0.574048167413494,
1.48269027894408));
#53222=CARTESIAN_POINT('Ctrl Pts',(0.639343799075583,-0.468402808767816,
1.48663646552757));
#53223=CARTESIAN_POINT('Ctrl Pts',(0.7167428178734,-0.362757450122139,1.49058265211106));
#53224=CARTESIAN_POINT('Ctrl Pts',(0.767397146317053,-0.237518113870631,
1.49452883869456));
#53225=CARTESIAN_POINT('Ctrl Pts',(0.78520518821855,-0.107770576098722,
1.49847502527805));
#53226=CARTESIAN_POINT('Ctrl Pts',(0.803013230120048,0.021976961673187,
1.50242121186154));
#53227=CARTESIAN_POINT('Ctrl Pts',(0.787974985479389,0.156232700965494,
1.50636739844503));
#53228=CARTESIAN_POINT('Ctrl Pts',(0.7419018946807,0.278824789692679,1.51031358502852));
#53229=CARTESIAN_POINT('Ctrl Pts',(0.69582880388201,0.401416878419864,1.51425977161201));
#53230=CARTESIAN_POINT('Ctrl Pts',(0.618720866925289,0.512345316581927,
1.5182059581955));
#53231=CARTESIAN_POINT('Ctrl Pts',(0.519866164585757,0.598248155531527,
1.522152144779));
#53232=CARTESIAN_POINT('Ctrl Pts',(0.421011462246225,0.684150994481125,
1.52609833136249));
#53233=CARTESIAN_POINT('Ctrl Pts',(0.30040999452388,0.745028234218261,1.53004451794598));
#53234=CARTESIAN_POINT('Ctrl Pts',(0.172588880390198,0.773546871911222,
1.53399070452947));
#53235=CARTESIAN_POINT('Ctrl Pts',(0.0447677662565173,0.802065509604184,
1.53793689111296));
#53236=CARTESIAN_POINT('Ctrl Pts',(-0.0902729942885018,0.798225545252973,
1.54188307769645));
#53237=CARTESIAN_POINT('Ctrl Pts',(-0.216266988974055,0.762489523966117,
1.54582926427995));
#53238=CARTESIAN_POINT('Ctrl Pts',(-0.342260983659614,0.72675350267926,
1.54977545086344));
#53239=CARTESIAN_POINT('Ctrl Pts',(-0.459208212485706,0.659121424456755,
1.55372163744693));
#53240=CARTESIAN_POINT('Ctrl Pts',(-0.553021729923176,0.567739950074642,
1.55766782403042));
#53241=CARTESIAN_POINT('Ctrl Pts',(-0.646835247360645,0.47635847569253,
1.56161401061392));
#53242=CARTESIAN_POINT('Ctrl Pts',(-0.717515053409493,0.361227605150811,
1.56556019719741));
#53243=CARTESIAN_POINT('Ctrl Pts',(-0.756547371490182,0.236215493499633,
1.5695063837809));
#53244=CARTESIAN_POINT('Ctrl Pts',(-0.78036833582658,0.159922073080573,
1.57191469500842));
#53245=CARTESIAN_POINT('Ctrl Pts',(-0.792402138697298,0.0799483673713918,
1.57432300623595));
#53246=CARTESIAN_POINT('Ctrl Pts',(-0.792446584180059,-1.22568943931671E-5,
1.57673131746348));
#53247=CARTESIAN_POINT('Origin',(0.,0.,1.095));
#53248=CARTESIAN_POINT('',(-0.792481714638565,1.94816894887317E-5,1.74826868253652));
#53249=CARTESIAN_POINT('',(-0.792480310976121,1.93743401778285E-5,1.72673131746348));
#53250=CARTESIAN_POINT('',(-0.7925,-9.70532588324277E-17,1.095));
#53251=CARTESIAN_POINT('Ctrl Pts',(-0.792481714638565,1.94816894887317E-5,
1.74826868253652));
#53252=CARTESIAN_POINT('Ctrl Pts',(-0.792515970057648,0.0363124968327356,
1.74717544451896));
#53253=CARTESIAN_POINT('Ctrl Pts',(-0.790067815952362,0.0726009269833459,
1.7460822065014));
#53254=CARTESIAN_POINT('Ctrl Pts',(-0.785099074206255,0.108540882887942,
1.74498896848384));
#53255=CARTESIAN_POINT('Ctrl Pts',(-0.767163746582846,0.23827088634904,
1.74104278190035));
#53256=CARTESIAN_POINT('Ctrl Pts',(-0.716386571322305,0.36346046522512,
1.73709659531685));
#53257=CARTESIAN_POINT('Ctrl Pts',(-0.638883942196417,0.469029836983938,
1.73315040873336));
#53258=CARTESIAN_POINT('Ctrl Pts',(-0.561381313070528,0.574599208742756,
1.72920422214987));
#53259=CARTESIAN_POINT('Ctrl Pts',(-0.457153230079291,0.660548373384312,
1.72525803556638));
#53260=CARTESIAN_POINT('Ctrl Pts',(-0.338754546744625,0.716524274981285,
1.72131184898289));
#53261=CARTESIAN_POINT('Ctrl Pts',(-0.220355863409961,0.772500176578257,
1.7173656623994));
#53262=CARTESIAN_POINT('Ctrl Pts',(-0.0877865797318678,0.798502815130648,
1.7134194758159));
#53263=CARTESIAN_POINT('Ctrl Pts',(0.0429845951824947,0.791400027896518,
1.70947328923241));
#53264=CARTESIAN_POINT('Ctrl Pts',(0.173755770096857,0.784297240662389,
1.70552710264892));
#53265=CARTESIAN_POINT('Ctrl Pts',(0.302728836247484,0.744089027641742,
1.70158091606543));
#53266=CARTESIAN_POINT('Ctrl Pts',(0.414368268972285,0.6756186921974,1.69763472948194));
#53267=CARTESIAN_POINT('Ctrl Pts',(0.526007701697086,0.607148356753058,
1.69368854289845));
#53268=CARTESIAN_POINT('Ctrl Pts',(0.620313500996059,0.510415898885018,
1.68974235631495));
#53269=CARTESIAN_POINT('Ctrl Pts',(0.685926007720852,0.3970732822915,1.68579616973146));
#53270=CARTESIAN_POINT('Ctrl Pts',(0.751538514445645,0.283730665697983,
1.68184998314797));
#53271=CARTESIAN_POINT('Ctrl Pts',(0.788457728596263,0.153777890378985,
1.67790379656448));
#53272=CARTESIAN_POINT('Ctrl Pts',(0.792236525055337,0.0228684924264428,
1.67395760998099));
#53273=CARTESIAN_POINT('Ctrl Pts',(0.796015321514411,-0.108040905526099,
1.67001142339749));
#53274=CARTESIAN_POINT('Ctrl Pts',(0.766653700281941,-0.239906926112185,
1.666065236814));
#53275=CARTESIAN_POINT('Ctrl Pts',(0.707688432285305,-0.356845572183794,
1.66211905023051));
#53276=CARTESIAN_POINT('Ctrl Pts',(0.648723164288668,-0.473784218255407,
1.65817286364702));
#53277=CARTESIAN_POINT('Ctrl Pts',(0.560154249527864,-0.575795489812542,
1.65422667706353));
#53278=CARTESIAN_POINT('Ctrl Pts',(0.452650307433518,-0.650591560626139,
1.65028049048003));
#53279=CARTESIAN_POINT('Ctrl Pts',(0.345146365339177,-0.725387631439732,
1.64633430389654));
#53280=CARTESIAN_POINT('Ctrl Pts',(0.218707395911295,-0.772968501509789,
1.64238811731305));
#53281=CARTESIAN_POINT('Ctrl Pts',(0.088563677737676,-0.787602789839644,
1.63844193072956));
#53282=CARTESIAN_POINT('Ctrl Pts',(-0.0415800404359447,-0.802237078169498,
1.63449574414607));
#53283=CARTESIAN_POINT('Ctrl Pts',(-0.175428507355303,-0.78392478475915,
1.63054955756258));
#53284=CARTESIAN_POINT('Ctrl Pts',(-0.296858929162171,-0.734871727415269,
1.62660337097908));
#53285=CARTESIAN_POINT('Ctrl Pts',(-0.418289350969042,-0.685818670071388,
1.62265718439559));
#53286=CARTESIAN_POINT('Ctrl Pts',(-0.527301727663422,-0.606024848793974,
1.6187109978121));
#53287=CARTESIAN_POINT('Ctrl Pts',(-0.610764910881114,-0.505101874094718,
1.61476481122861));
#53288=CARTESIAN_POINT('Ctrl Pts',(-0.694228094098805,-0.404178899395464,
1.61081862464512));
#53289=CARTESIAN_POINT('Ctrl Pts',(-0.752142083839809,-0.28212677127437,
1.60687243806163));
#53290=CARTESIAN_POINT('Ctrl Pts',(-0.777530817250417,-0.153647348833338,
1.60292625147813));
#53291=CARTESIAN_POINT('Ctrl Pts',(-0.787519344460865,-0.103100510348724,
1.6013737284976));
#53292=CARTESIAN_POINT('Ctrl Pts',(-0.792473542933907,-0.0515588415030537,
1.59982120551706));
#53293=CARTESIAN_POINT('Ctrl Pts',(-0.792445760035067,-1.19013985881156E-5,
1.59826868253652));
#53294=CARTESIAN_POINT('Ctrl Pts',(-0.792446584180059,-1.22568943931671E-5,
1.57673131746348));
#53295=CARTESIAN_POINT('Ctrl Pts',(-0.792474965733008,-0.0510727145712751,
1.57826919281944));
#53296=CARTESIAN_POINT('Ctrl Pts',(-0.787614426950324,-0.102127838006081,
1.57980706817541));
#53297=CARTESIAN_POINT('Ctrl Pts',(-0.777812317880636,-0.152215908600686,
1.58134494353137));
#53298=CARTESIAN_POINT('Ctrl Pts',(-0.752660116077868,-0.280741846289199,
1.58529113011487));
#53299=CARTESIAN_POINT('Ctrl Pts',(-0.6949708823598,-0.402900368905588,
1.58923731669836));
#53300=CARTESIAN_POINT('Ctrl Pts',(-0.611693606464474,-0.503976801537991,
1.59318350328185));
#53301=CARTESIAN_POINT('Ctrl Pts',(-0.52841633056915,-0.605053234170393,
1.59712968986534));
#53302=CARTESIAN_POINT('Ctrl Pts',(-0.41955101249657,-0.685047576818808,
1.60107587644883));
#53303=CARTESIAN_POINT('Ctrl Pts',(-0.298211086580291,-0.734324065054783,
1.60502206303232));
#53304=CARTESIAN_POINT('Ctrl Pts',(-0.176871160664012,-0.783600553290759,
1.60896824961582));
#53305=CARTESIAN_POINT('Ctrl Pts',(-0.0430566269040337,-0.802159187114293,
1.61291443619931));
#53306=CARTESIAN_POINT('Ctrl Pts',(0.0871138082795939,-0.787764475642946,
1.6168606227828));
#53307=CARTESIAN_POINT('Ctrl Pts',(0.217284243463222,-0.773369764171598,
1.62080680936629));
#53308=CARTESIAN_POINT('Ctrl Pts',(0.343810580070499,-0.726021707405367,
1.62475299594978));
#53309=CARTESIAN_POINT('Ctrl Pts',(0.451452015649914,-0.651423642680866,
1.62869918253328));
#53310=CARTESIAN_POINT('Ctrl Pts',(0.559093451229331,-0.576825577956364,
1.63264536911677));
#53311=CARTESIAN_POINT('Ctrl Pts',(0.647849985780886,-0.474977505273591,
1.63659155570026));
#53312=CARTESIAN_POINT('Ctrl Pts',(0.70703040002444,-0.358147592647585,
1.64053774228375));
#53313=CARTESIAN_POINT('Ctrl Pts',(0.766210814267993,-0.241317680021578,
1.64448392886724));
#53314=CARTESIAN_POINT('Ctrl Pts',(0.795815108203546,-0.10950592745234,
1.64843011545073));
#53315=CARTESIAN_POINT('Ctrl Pts',(0.792277279624073,0.021410204797208,
1.65237630203423));
#53316=CARTESIAN_POINT('Ctrl Pts',(0.7887394510446,0.152326337046754,1.65632248861772));
#53317=CARTESIAN_POINT('Ctrl Pts',(0.752059499950102,0.282346848976609,
1.66026867520121));
#53318=CARTESIAN_POINT('Ctrl Pts',(0.686655730889281,0.395810045242522,
1.6642148617847));
#53319=CARTESIAN_POINT('Ctrl Pts',(0.621251961828459,0.509273241508435,
1.66816104836819));
#53320=CARTESIAN_POINT('Ctrl Pts',(0.527124374801314,0.606179122110405,
1.67210723495168));
#53321=CARTESIAN_POINT('Ctrl Pts',(0.415611162294765,0.674854833615329,
1.67605342153518));
#53322=CARTESIAN_POINT('Ctrl Pts',(0.304097949788216,0.743530545120253,
1.67999960811867));
#53323=CARTESIAN_POINT('Ctrl Pts',(0.175199111802263,0.783976087528131,
1.68394579470216));
#53324=CARTESIAN_POINT('Ctrl Pts',(0.0444412318028534,0.791319569828665,
1.68789198128565));
#53325=CARTESIAN_POINT('Ctrl Pts',(-0.0863166481965564,0.7986630521292,
1.69183816786914));
#53326=CARTESIAN_POINT('Ctrl Pts',(-0.218933570209423,0.772904474322392,
1.69578435445264));
#53327=CARTESIAN_POINT('Ctrl Pts',(-0.337435086825647,0.717146600673075,
1.69973054103613));
#53328=CARTESIAN_POINT('Ctrl Pts',(-0.455936603441873,0.661388727023757,
1.70367672761962));
#53329=CARTESIAN_POINT('Ctrl Pts',(-0.560322714661454,0.575631557531931,
1.70762291420311));
#53330=CARTESIAN_POINT('Ctrl Pts',(-0.638019531581584,0.470205021239029,
1.7115691007866));
#53331=CARTESIAN_POINT('Ctrl Pts',(-0.715716348501714,0.364778484946126,
1.71551528737009));
#53332=CARTESIAN_POINT('Ctrl Pts',(-0.766723871122392,0.239682581852148,
1.71946147395359));
#53333=CARTESIAN_POINT('Ctrl Pts',(-0.784897959048439,0.109985810719267,
1.72340766053708));
#53334=CARTESIAN_POINT('Ctrl Pts',(-0.790000305490033,0.0735736473485991,
1.72451554617921));
#53335=CARTESIAN_POINT('Ctrl Pts',(-0.792514731297942,0.0367988450569207,
1.72562343182135));
#53336=CARTESIAN_POINT('Ctrl Pts',(-0.792480310976121,1.93743401778285E-5,
1.72673131746348));
#53337=CARTESIAN_POINT('Origin',(0.,0.,1.095));
#53338=CARTESIAN_POINT('',(-0.792561345414955,-6.95798684707816E-6,1.89826868253652));
#53339=CARTESIAN_POINT('',(-0.792562019808975,-6.48812038781812E-6,1.87673131746348));
#53340=CARTESIAN_POINT('',(-0.7925,-9.70532588324277E-17,1.095));
#53341=CARTESIAN_POINT('Ctrl Pts',(-0.792561345414955,-6.95798684707816E-6,
1.89826868253652));
#53342=CARTESIAN_POINT('Ctrl Pts',(-0.792503577448366,0.124083294659953,
1.89452968352086));
#53343=CARTESIAN_POINT('Ctrl Pts',(-0.762860507627894,0.248200183905096,
1.8907906845052));
#53344=CARTESIAN_POINT('Ctrl Pts',(-0.706678680884356,0.358841081198739,
1.88705168548954));
#53345=CARTESIAN_POINT('Ctrl Pts',(-0.647383674385861,0.475612875643471,
1.88310549890605));
#53346=CARTESIAN_POINT('Ctrl Pts',(-0.558527260508677,0.577373820519587,
1.87915931232256));
#53347=CARTESIAN_POINT('Ctrl Pts',(-0.450812689552982,0.651866242813804,
1.87521312573907));
#53348=CARTESIAN_POINT('Ctrl Pts',(-0.343098118597287,0.726358665108021,
1.87126693915557));
#53349=CARTESIAN_POINT('Ctrl Pts',(-0.21652539056308,0.773582564820339,
1.86732075257208));
#53350=CARTESIAN_POINT('Ctrl Pts',(-0.0863408960085328,0.78784956003754,
1.86337456598859));
#53351=CARTESIAN_POINT('Ctrl Pts',(0.0438435985460143,0.80211655525474,
1.8594283794051));
#53352=CARTESIAN_POINT('Ctrl Pts',(0.177639859620902,0.783426645976824,
1.85548219282161));
#53353=CARTESIAN_POINT('Ctrl Pts',(0.298931381843208,0.734031135939183,
1.85153600623812));
#53354=CARTESIAN_POINT('Ctrl Pts',(0.420222904065518,0.684635625901541,
1.84758981965462));
#53355=CARTESIAN_POINT('Ctrl Pts',(0.529009687435246,0.604534515104173,
1.84364363307113));
#53356=CARTESIAN_POINT('Ctrl Pts',(0.612187757561329,0.503376428797804,
1.83969744648764));
#53357=CARTESIAN_POINT('Ctrl Pts',(0.695365827687409,0.402218342491439,
1.83575125990415));
#53358=CARTESIAN_POINT('Ctrl Pts',(0.752935184569847,0.280003280676073,
1.83180507332066));
#53359=CARTESIAN_POINT('Ctrl Pts',(0.777961278303689,0.151452728723369,
1.82785888673717));
#53360=CARTESIAN_POINT('Ctrl Pts',(0.802987372037531,0.0229021767706633,
1.82391270015367));
#53361=CARTESIAN_POINT('Ctrl Pts',(0.795470202622776,-0.111983865319381,
1.81996651357018));
#53362=CARTESIAN_POINT('Ctrl Pts',(0.75631525501308,-0.236957621975268,
1.81602032698669));
#53363=CARTESIAN_POINT('Ctrl Pts',(0.717160307403383,-0.361931378631156,
1.8120741404032));
#53364=CARTESIAN_POINT('Ctrl Pts',(0.646367581598744,-0.476992849852886,
1.80812795381971));
#53365=CARTESIAN_POINT('Ctrl Pts',(0.552464455992677,-0.568282240125679,
1.80418176723621));
#53366=CARTESIAN_POINT('Ctrl Pts',(0.458561330386612,-0.659571630398471,
1.80023558065272));
#53367=CARTESIAN_POINT('Ctrl Pts',(0.341547804979119,-0.727088939722326,
1.79628939406923));
#53368=CARTESIAN_POINT('Ctrl Pts',(0.215518811092083,-0.762701331874485,
1.79234320748574));
#53369=CARTESIAN_POINT('Ctrl Pts',(0.0894898172050466,-0.798313724026643,
1.78839702090225));
#53370=CARTESIAN_POINT('Ctrl Pts',(-0.0455546451615332,-0.802021199007106,
1.78445083431876));
#53371=CARTESIAN_POINT('Ctrl Pts',(-0.173347717831807,-0.773377170790614,
1.78050464773526));
#53372=CARTESIAN_POINT('Ctrl Pts',(-0.301140790502082,-0.744733142574123,
1.77655846115177));
#53373=CARTESIAN_POINT('Ctrl Pts',(-0.42168247347605,-0.683737611160677,
1.77261227456828));
#53374=CARTESIAN_POINT('Ctrl Pts',(-0.5204528491884,-0.597737828273649,
1.76866608798479));
#53375=CARTESIAN_POINT('Ctrl Pts',(-0.61922322490075,-0.51173804538662,
1.7647199014013));
#53376=CARTESIAN_POINT('Ctrl Pts',(-0.696222293351481,-0.400734011026008,
1.7607737148178));
#53377=CARTESIAN_POINT('Ctrl Pts',(-0.742175087583709,-0.278096779822644,
1.75682752823431));
#53378=CARTESIAN_POINT('Ctrl Pts',(-0.775397277065014,-0.189434547186454,
1.75397457966838));
#53379=CARTESIAN_POINT('Ctrl Pts',(-0.792392320611665,-0.0946919204416087,
1.75112163110245));
#53380=CARTESIAN_POINT('Ctrl Pts',(-0.792481714638565,1.94816894887317E-5,
1.74826868253652));
#53381=CARTESIAN_POINT('Ctrl Pts',(-0.792480310976121,1.93743401778285E-5,
1.72673131746348));
#53382=CARTESIAN_POINT('Ctrl Pts',(-0.792392129282894,-0.0942062410012334,
1.72956961840484));
#53383=CARTESIAN_POINT('Ctrl Pts',(-0.775574922487285,-0.188462496952598,
1.73240791934619));
#53384=CARTESIAN_POINT('Ctrl Pts',(-0.742685718766298,-0.276730207636548,
1.73524622028755));
#53385=CARTESIAN_POINT('Ctrl Pts',(-0.696958737326693,-0.399451815687699,
1.73919240687104));
#53386=CARTESIAN_POINT('Ctrl Pts',(-0.620164121216066,-0.510597392618217,
1.74313859345454));
#53387=CARTESIAN_POINT('Ctrl Pts',(-0.5215522099674,-0.596778834205856,
1.74708478003803));
#53388=CARTESIAN_POINT('Ctrl Pts',(-0.422940298718735,-0.682960275793493,
1.75103096662152));
#53389=CARTESIAN_POINT('Ctrl Pts',(-0.302511092332032,-0.744177582038251,
1.75497715320501));
#53390=CARTESIAN_POINT('Ctrl Pts',(-0.174770959940769,-0.773056787202183,
1.7589233397885));
#53391=CARTESIAN_POINT('Ctrl Pts',(-0.0470308275495023,-0.801935992366116,
1.762869526372));
#53392=CARTESIAN_POINT('Ctrl Pts',(0.088020230846324,-0.79847709644922,
1.76681571295549));
#53393=CARTESIAN_POINT('Ctrl Pts',(0.21411456254238,-0.763096742743189,
1.77076189953898));
#53394=CARTESIAN_POINT('Ctrl Pts',(0.340208894238434,-0.727716389037158,
1.77470808612247));
#53395=CARTESIAN_POINT('Ctrl Pts',(0.457346499234716,-0.660414577541993,
1.77865427270596));
#53396=CARTESIAN_POINT('Ctrl Pts',(0.551417500131295,-0.569298186565646,
1.78260045928945));
#53397=CARTESIAN_POINT('Ctrl Pts',(0.645488501027873,-0.478181795589299,
1.78654664587295));
#53398=CARTESIAN_POINT('Ctrl Pts',(0.716492897824747,-0.363250825131771,
1.79049283245644));
#53399=CARTESIAN_POINT('Ctrl Pts',(0.755877815177639,-0.238349351163912,
1.79443901903993));
#53400=CARTESIAN_POINT('Ctrl Pts',(0.795262732530532,-0.113447877196051,
1.79838520562342));
#53401=CARTESIAN_POINT('Ctrl Pts',(0.803028170439441,0.021424100282145,
1.80233139220691));
#53402=CARTESIAN_POINT('Ctrl Pts',(0.778238738626799,0.150020499861006,
1.80627757879041));
#53403=CARTESIAN_POINT('Ctrl Pts',(0.753449306814156,0.278616899439865,
1.8102237653739));
#53404=CARTESIAN_POINT('Ctrl Pts',(0.696105005279964,0.400937721119394,
1.81416995195739));
#53405=CARTESIAN_POINT('Ctrl Pts',(0.613113274758198,0.502248740160955,
1.81811613854088));
#53406=CARTESIAN_POINT('Ctrl Pts',(0.53012154423643,0.603559759202518,1.82206232512437));
#53407=CARTESIAN_POINT('Ctrl Pts',(0.421482384727094,0.683860975606109,
1.82600851170787));
#53408=CARTESIAN_POINT('Ctrl Pts',(0.300281988504285,0.733479660289139,
1.82995469829136));
#53409=CARTESIAN_POINT('Ctrl Pts',(0.179081592281479,0.783098344972167,
1.83390088487485));
#53410=CARTESIAN_POINT('Ctrl Pts',(0.0453199593452004,0.802034497934631,
1.83784707145834));
#53411=CARTESIAN_POINT('Ctrl Pts',(-0.0848905760835689,0.788007154009545,
1.84179325804183));
#53412=CARTESIAN_POINT('Ctrl Pts',(-0.21510111151234,0.773979810084459,
1.84573944462532));
#53413=CARTESIAN_POINT('Ctrl Pts',(-0.341760549433607,0.726988969271823,
1.84968563120882));
#53414=CARTESIAN_POINT('Ctrl Pts',(-0.449612054600708,0.652694940255893,
1.85363181779231));
#53415=CARTESIAN_POINT('Ctrl Pts',(-0.557463559767808,0.578400911239963,
1.8575780043758));
#53416=CARTESIAN_POINT('Ctrl Pts',(-0.646507132180743,0.476803694020739,
1.86152419095929));
#53417=CARTESIAN_POINT('Ctrl Pts',(-0.706016977249189,0.360141239674046,
1.86547037754278));
#53418=CARTESIAN_POINT('Ctrl Pts',(-0.762623254037114,0.249170909068881,
1.86922402418301));
#53419=CARTESIAN_POINT('Ctrl Pts',(-0.79250747892361,0.124569584863353,
1.87297767082325));
#53420=CARTESIAN_POINT('Ctrl Pts',(-0.792562019808975,-6.48812038781812E-6,
1.87673131746348));
#53421=CARTESIAN_POINT('Origin',(0.,0.,1.095));
#53422=CARTESIAN_POINT('',(-0.792448351156449,-1.30718296499355E-5,2.04826868253652));
#53423=CARTESIAN_POINT('',(-0.792449256123249,-1.33074723724148E-5,2.02673131746348));
#53424=CARTESIAN_POINT('',(-0.7925,-9.70532588324277E-17,1.095));
#53425=CARTESIAN_POINT('Ctrl Pts',(-0.792448351156449,-1.30718296499355E-5,
2.04826868253652));
#53426=CARTESIAN_POINT('Ctrl Pts',(-0.792400580040907,0.0809518333973197,
2.04583010910626));
#53427=CARTESIAN_POINT('Ctrl Pts',(-0.780057502508409,0.161931022031344,
2.04339153567599));
#53428=CARTESIAN_POINT('Ctrl Pts',(-0.755643607895046,0.239090868906411,
2.04095296224572));
#53429=CARTESIAN_POINT('Ctrl Pts',(-0.716136172040015,0.363953687775635,
2.03700677566223));
#53430=CARTESIAN_POINT('Ctrl Pts',(-0.645019047037377,0.478814846861572,
2.03306058907874));
#53431=CARTESIAN_POINT('Ctrl Pts',(-0.550858697000239,0.569838878089452,
2.02911440249525));
#53432=CARTESIAN_POINT('Ctrl Pts',(-0.456698346963102,0.660862909317332,
2.02516821591175));
#53433=CARTESIAN_POINT('Ctrl Pts',(-0.339494771891465,0.728049812687156,
2.02122202932826));
#53434=CARTESIAN_POINT('Ctrl Pts',(-0.213365790576425,0.7633064507015,2.01727584274477));
#53435=CARTESIAN_POINT('Ctrl Pts',(-0.087236809261385,0.798563088715845,
2.01332965616128));
#53436=CARTESIAN_POINT('Ctrl Pts',(0.0478175782970594,0.801889461374709,
2.00938346957779));
#53437=CARTESIAN_POINT('Ctrl Pts',(0.175529315812979,0.772884939389923,
2.0054372829943));
#53438=CARTESIAN_POINT('Ctrl Pts',(0.303241053328903,0.743880417405136,
2.0014910964108));
#53439=CARTESIAN_POINT('Ctrl Pts',(0.423610140802298,0.682545000776699,
1.99754490982731));
#53440=CARTESIAN_POINT('Ctrl Pts',(0.522137452055428,0.596266856583147,
1.99359872324382));
#53441=CARTESIAN_POINT('Ctrl Pts',(0.620664763308554,0.509988712389599,
1.98965253666033));
#53442=CARTESIAN_POINT('Ctrl Pts',(0.697350298341415,0.398767840630934,
1.98570635007684));
#53443=CARTESIAN_POINT('Ctrl Pts',(0.742956856388529,0.276001428216633,
1.98176016349334));
#53444=CARTESIAN_POINT('Ctrl Pts',(0.788563414435643,0.153235015802332,
1.97781397690985));
#53445=CARTESIAN_POINT('Ctrl Pts',(0.803090995497015,0.0189230627323887,
1.97386779032636));
#53446=CARTESIAN_POINT('Ctrl Pts',(0.784789671794817,-0.110755814222861,
1.96992160374287));
#53447=CARTESIAN_POINT('Ctrl Pts',(0.76648834809262,-0.240434691178112,
1.96597541715938));
#53448=CARTESIAN_POINT('Ctrl Pts',(0.715358119626854,-0.365480492018664,
1.96202923057589));
#53449=CARTESIAN_POINT('Ctrl Pts',(0.63755790722776,-0.470830749750958,
1.95808304399239));
#53450=CARTESIAN_POINT('Ctrl Pts',(0.559757694828668,-0.576181007483251,
1.9541368574089));
#53451=CARTESIAN_POINT('Ctrl Pts',(0.455287498496249,-0.66183572210728,
1.95019067082541));
#53452=CARTESIAN_POINT('Ctrl Pts',(0.336731335738727,-0.717477307524271,
1.94624448424192));
#53453=CARTESIAN_POINT('Ctrl Pts',(0.218175172981203,-0.773118892941263,
1.94229829765843));
#53454=CARTESIAN_POINT('Ctrl Pts',(0.0855330437985741,-0.798747349151216,
1.93835211107493));
#53455=CARTESIAN_POINT('Ctrl Pts',(-0.0452175680979145,-0.791275584909749,
1.93440592449144));
#53456=CARTESIAN_POINT('Ctrl Pts',(-0.175968179994401,-0.783803820668283,
1.93045973790795));
#53457=CARTESIAN_POINT('Ctrl Pts',(-0.304827274604749,-0.743231835975397,
1.92651355132446));
#53458=CARTESIAN_POINT('Ctrl Pts',(-0.416273055752392,-0.674446752949849,
1.92256736474097));
#53459=CARTESIAN_POINT('Ctrl Pts',(-0.527718836900035,-0.605661669924301,
1.91862117815748));
#53460=CARTESIAN_POINT('Ctrl Pts',(-0.621751304584975,-0.508663488566089,
1.91467499157398));
#53461=CARTESIAN_POINT('Ctrl Pts',(-0.687043723986203,-0.39513618023112,
1.91072880499049));
#53462=CARTESIAN_POINT('Ctrl Pts',(-0.752336143387432,-0.281608871896149,
1.906782618407));
#53463=CARTESIAN_POINT('Ctrl Pts',(-0.78888851450495,-0.151552436584419,
1.90283643182351));
#53464=CARTESIAN_POINT('Ctrl Pts',(-0.792297900503804,-0.0206328969218787,
1.89889024524002));
#53465=CARTESIAN_POINT('Ctrl Pts',(-0.792476904303538,-0.013759197356366,
1.89868305767219));
#53466=CARTESIAN_POINT('Ctrl Pts',(-0.792564546486805,-0.00688311856615801,
1.89847587010435));
#53467=CARTESIAN_POINT('Ctrl Pts',(-0.792561345414955,-6.95798684707816E-6,
1.89826868253652));
#53468=CARTESIAN_POINT('Ctrl Pts',(-0.792562019808975,-6.48812038781812E-6,
1.87673131746348));
#53469=CARTESIAN_POINT('Ctrl Pts',(-0.792564817434852,-0.0063965062341521,
1.87692385740674));
#53470=CARTESIAN_POINT('Ctrl Pts',(-0.792489130621737,-0.0127864579098014,
1.87711639735));
#53471=CARTESIAN_POINT('Ctrl Pts',(-0.79233453996622,-0.0191745001120404,
1.87730893729326));
#53472=CARTESIAN_POINT('Ctrl Pts',(-0.789166139890846,-0.150100094077262,
1.88125512387675));
#53473=CARTESIAN_POINT('Ctrl Pts',(-0.752853222016141,-0.280223590533543,
1.88520131046024));
#53474=CARTESIAN_POINT('Ctrl Pts',(-0.687769879693997,-0.393870889078232,
1.88914749704373));
#53475=CARTESIAN_POINT('Ctrl Pts',(-0.622686537371856,-0.507518187622918,
1.89309368362722));
#53476=CARTESIAN_POINT('Ctrl Pts',(-0.528832770602275,-0.604689288256013,
1.89703987021072));
#53477=CARTESIAN_POINT('Ctrl Pts',(-0.417513788695573,-0.673679390309865,
1.90098605679421));
#53478=CARTESIAN_POINT('Ctrl Pts',(-0.306194806788868,-0.742669492363719,
1.9049322433777));
#53479=CARTESIAN_POINT('Ctrl Pts',(-0.177410609745039,-0.783478595838328,
1.90887842996119));
#53480=CARTESIAN_POINT('Ctrl Pts',(-0.0466739718904146,-0.791191016773624,
1.91282461654468));
#53481=CARTESIAN_POINT('Ctrl Pts',(0.0840626659642058,-0.798903437708921,
1.91677080312818));
#53482=CARTESIAN_POINT('Ctrl Pts',(0.216751744629622,-0.773519176104906,
1.92071698971167));
#53483=CARTESIAN_POINT('Ctrl Pts',(0.335410125026388,-0.718095907739533,
1.92466317629516));
#53484=CARTESIAN_POINT('Ctrl Pts',(0.454068505423155,-0.66267263937416,
1.92860936287865));
#53485=CARTESIAN_POINT('Ctrl Pts',(0.558696187551273,-0.577210364247426,
1.93255554946214));
#53486=CARTESIAN_POINT('Ctrl Pts',(0.636690183942362,-0.472003489758499,
1.93650173604564));
#53487=CARTESIAN_POINT('Ctrl Pts',(0.714684180333452,-0.36679661526957,
1.94044792262913));
#53488=CARTESIAN_POINT('Ctrl Pts',(0.766044490987512,-0.241845141418452,
1.94439410921262));
#53489=CARTESIAN_POINT('Ctrl Pts',(0.78458448023081,-0.112200169605353,
1.94834029579611));
#53490=CARTESIAN_POINT('Ctrl Pts',(0.803124469474107,0.0174448022077428,
1.9522864823796));
#53491=CARTESIAN_POINT('Ctrl Pts',(0.788844137306641,0.151783271982819,
1.95623266896309));
#53492=CARTESIAN_POINT('Ctrl Pts',(0.743463629318252,0.274633422178461,
1.96017885554659));
#53493=CARTESIAN_POINT('Ctrl Pts',(0.698083121329863,0.397483572374106,
1.96412504213008));
#53494=CARTESIAN_POINT('Ctrl Pts',(0.621602437520548,0.508845402990322,
1.96807122871357));
#53495=CARTESIAN_POINT('Ctrl Pts',(0.523234102552766,0.595304761057008,
1.97201741529706));
#53496=CARTESIAN_POINT('Ctrl Pts',(0.424865767584983,0.681764119123695,
1.97596360188055));
#53497=CARTESIAN_POINT('Ctrl Pts',(0.304609781458736,0.74332100464085,1.97990978846404));
#53498=CARTESIAN_POINT('Ctrl Pts',(0.176951647912409,0.772560547231348,
1.98385597504754));
#53499=CARTESIAN_POINT('Ctrl Pts',(0.0492935143660849,0.801800089821845,
1.98780216163103));
#53500=CARTESIAN_POINT('Ctrl Pts',(-0.0857667666003156,0.798722289485685,
1.99174834821452));
#53501=CARTESIAN_POINT('Ctrl Pts',(-0.211960431274993,0.763697885264852,
1.99569453479801));
#53502=CARTESIAN_POINT('Ctrl Pts',(-0.338154095949671,0.728673481044019,
1.9996407213815));
#53503=CARTESIAN_POINT('Ctrl Pts',(-0.455481144332627,0.661702472938513,
2.00358690796499));
#53504=CARTESIAN_POINT('Ctrl Pts',(-0.549808879704876,0.570851890488339,
2.00753309454849));
#53505=CARTESIAN_POINT('Ctrl Pts',(-0.644136615077125,0.480001308038165,
2.01147928113198));
#53506=CARTESIAN_POINT('Ctrl Pts',(-0.715465037438667,0.365271151243323,
2.01542546771547));
#53507=CARTESIAN_POINT('Ctrl Pts',(-0.75520224037866,0.240481310225466,
2.01937165429896));
#53508=CARTESIAN_POINT('Ctrl Pts',(-0.779905619413149,0.162903360238067,
2.0218248753538));
#53509=CARTESIAN_POINT('Ctrl Pts',(-0.792399873864259,0.0814376230681167,
2.02427809640864));
#53510=CARTESIAN_POINT('Ctrl Pts',(-0.792449256123249,-1.33074723724148E-5,
2.02673131746348));
#53511=CARTESIAN_POINT('Origin',(0.,0.,0.522718733092613));
#53512=CARTESIAN_POINT('',(-0.706803933141875,-1.1659082385242E-5,2.09771873309261));
#53513=CARTESIAN_POINT('',(-0.706829164831431,1.42933870884709E-5,2.12728126690739));
#53514=CARTESIAN_POINT('',(-0.70685,-2.56204009907072E-14,0.522718733092613));
#53515=CARTESIAN_POINT('',(0.347825520797267,-0.615372974259066,2.1475));
#53516=CARTESIAN_POINT('Ctrl Pts',(-0.706803933141875,-1.16590823852313E-5,
2.09771873309261));
#53517=CARTESIAN_POINT('Ctrl Pts',(-0.706830275063582,-0.0446572816595,
2.09922634624584));
#53518=CARTESIAN_POINT('Ctrl Pts',(-0.691762579617961,-0.206145477660671,
2.10468014598255));
#53519=CARTESIAN_POINT('Ctrl Pts',(-0.570183826489577,-0.466147172833569,
2.11408013230277));
#53520=CARTESIAN_POINT('Ctrl Pts',(-0.279700959344392,-0.681302019989293,
2.12591869205323));
#53521=CARTESIAN_POINT('Ctrl Pts',(0.0570467425526827,-0.729307650008237,
2.13705864795232));
#53522=CARTESIAN_POINT('Ctrl Pts',(0.264076432689668,-0.662598430928655,
2.1442524172679));
#53523=CARTESIAN_POINT('Ctrl Pts',(0.347825520797267,-0.615372974259065,
2.1475));
#53524=CARTESIAN_POINT('',(-0.468142317532551,-0.529603335559031,2.1475));
#53525=CARTESIAN_POINT('Origin',(0.,0.,2.1475));
#53526=CARTESIAN_POINT('Ctrl Pts',(-0.706829164831431,1.42933870884675E-5,
2.12728126690739));
#53527=CARTESIAN_POINT('Ctrl Pts',(-0.706754789907476,-0.0827061914899486,
2.13007465802143));
#53528=CARTESIAN_POINT('Ctrl Pts',(-0.671726507282576,-0.282346804235477,
2.13681423571897));
#53529=CARTESIAN_POINT('Ctrl Pts',(-0.555684412749315,-0.452220591560317,
2.14355381341651));
#53530=CARTESIAN_POINT('Ctrl Pts',(-0.468142317532544,-0.529603335559038,
2.1475));
#53531=CARTESIAN_POINT('Origin',(0.,0.,0.522718733092613));
#53532=CARTESIAN_POINT('',(-0.706904715465692,-6.20599748763955E-6,1.94771873309261));
#53533=CARTESIAN_POINT('',(-0.706804740303746,-1.18692578732482E-5,1.97728126690739));
#53534=CARTESIAN_POINT('',(-0.70685,-2.56204009907072E-14,0.522718733092613));
#53535=CARTESIAN_POINT('Ctrl Pts',(-0.706904715465692,-6.20599748754613E-6,
1.94771873309261));
#53536=CARTESIAN_POINT('Ctrl Pts',(-0.70690757057943,-0.00613922064163216,
1.94792592066044));
#53537=CARTESIAN_POINT('Ctrl Pts',(-0.705340536134816,-0.129082898063355,
1.95207929481177));
#53538=CARTESIAN_POINT('Ctrl Pts',(-0.638424933033424,-0.367174286939925,
1.96017885554658));
#53539=CARTESIAN_POINT('Ctrl Pts',(-0.386815407040617,-0.626719389121822,
1.97201741529706));
#53540=CARTESIAN_POINT('Ctrl Pts',(-0.0420177375441198,-0.735280805071978,
1.98385597504754));
#53541=CARTESIAN_POINT('Ctrl Pts',(0.312902473229659,-0.666704877228424,
1.99569453479801));
#53542=CARTESIAN_POINT('Ctrl Pts',(0.592440990368726,-0.437512315593109,
2.00753309454849));
#53543=CARTESIAN_POINT('Ctrl Pts',(0.729253868568196,-0.102918154113688,
2.01937165429896));
#53544=CARTESIAN_POINT('Ctrl Pts',(0.690381361287827,0.256470126116556,
2.03121021404944));
#53545=CARTESIAN_POINT('Ctrl Pts',(0.485188287074669,0.554071917419808,
2.04304877379991));
#53546=CARTESIAN_POINT('Ctrl Pts',(0.163107948346954,0.718191561244962,
2.05488733355038));
#53547=CARTESIAN_POINT('Ctrl Pts',(-0.198266917945865,0.709290943526656,
2.06672589330087));
#53548=CARTESIAN_POINT('Ctrl Pts',(-0.511877064467201,0.529514050225861,
2.07856445305133));
#53549=CARTESIAN_POINT('Ctrl Pts',(-0.677936930706799,0.261311015960508,
2.08889539964859));
#53550=CARTESIAN_POINT('Ctrl Pts',(-0.706761324923553,0.0722029065449757,
2.09528015966235));
#53551=CARTESIAN_POINT('Ctrl Pts',(-0.706803933141875,-1.16590823852313E-5,
2.09771873309261));
#53552=CARTESIAN_POINT('Ctrl Pts',(-0.706804740303746,-1.18692578732899E-5,
1.97728126690739));
#53553=CARTESIAN_POINT('Ctrl Pts',(-0.706831545071039,-0.0442235615473762,
1.97877423243604));
#53554=CARTESIAN_POINT('Ctrl Pts',(-0.691952157749641,-0.205277190188198,
1.98421338454819));
#53555=CARTESIAN_POINT('Ctrl Pts',(-0.571040857364167,-0.465097524278119,
1.99359872324382));
#53556=CARTESIAN_POINT('Ctrl Pts',(-0.280954601492375,-0.680784722238707,
2.0054372829943));
#53557=CARTESIAN_POINT('Ctrl Pts',(0.0768167392428667,-0.732463381911148,
2.01727584274477));
#53558=CARTESIAN_POINT('Ctrl Pts',(0.416082091960603,-0.607683269644344,
2.02911440249525));
#53559=CARTESIAN_POINT('Ctrl Pts',(0.655108589511754,-0.336505836512168,
2.04095296224572));
#53560=CARTESIAN_POINT('Ctrl Pts',(0.736312206455239,0.0157403015675272,
2.0527915219962));
#53561=CARTESIAN_POINT('Ctrl Pts',(0.640129844349537,0.364193045069704,
2.06463008174667));
#53562=CARTESIAN_POINT('Ctrl Pts',(0.389733384979782,0.624910355165805,
2.07646864149715));
#53563=CARTESIAN_POINT('Ctrl Pts',(0.0454451798068112,0.735074392267673,
2.08830720124762));
#53564=CARTESIAN_POINT('Ctrl Pts',(-0.309790030899746,0.668161503213349,
2.1001457609981));
#53565=CARTESIAN_POINT('Ctrl Pts',(-0.590395841023348,0.440259893769033,
2.11198432074857));
#53566=CARTESIAN_POINT('Ctrl Pts',(-0.696114850406353,0.185128362892587,
2.12102948938501));
#53567=CARTESIAN_POINT('Ctrl Pts',(-0.706859858376257,0.0341519405347402,
2.12612847143794));
#53568=CARTESIAN_POINT('Ctrl Pts',(-0.706829164831431,1.42933870884675E-5,
2.12728126690739));
#53569=CARTESIAN_POINT('Origin',(0.,0.,0.522718733092613));
#53570=CARTESIAN_POINT('',(-0.70683369084198,1.7376192061708E-5,1.79771873309261));
#53571=CARTESIAN_POINT('',(-0.7069053169741,-5.78691218949823E-6,1.82728126690739));
#53572=CARTESIAN_POINT('',(-0.70685,-2.56204009907072E-14,0.522718733092613));
#53573=CARTESIAN_POINT('Ctrl Pts',(-0.70683369084198,1.73761920617202E-5,
1.79771873309261));
#53574=CARTESIAN_POINT('Ctrl Pts',(-0.706753958137987,-0.0844580239295342,
1.80057168165854));
#53575=CARTESIAN_POINT('Ctrl Pts',(-0.670628779363002,-0.285845817928073,
1.80737081680797));
#53576=CARTESIAN_POINT('Ctrl Pts',(-0.483622895882263,-0.55543878746919,
1.81811613854088));
#53577=CARTESIAN_POINT('Ctrl Pts',(-0.161080730796523,-0.718648975656924,
1.82995469829136));
#53578=CARTESIAN_POINT('Ctrl Pts',(0.200267577937169,-0.708728614685542,
1.84179325804183));
#53579=CARTESIAN_POINT('Ctrl Pts',(0.513369194723111,-0.528067630096644,
1.85363181779231));
#53580=CARTESIAN_POINT('Ctrl Pts',(0.702794449871408,-0.22018926694303,
1.86547037754278));
#53581=CARTESIAN_POINT('Ctrl Pts',(0.722908687855579,0.140735145112547,
1.87730893729326));
#53582=CARTESIAN_POINT('Ctrl Pts',(0.568866164528063,0.467754891904443,
1.88914749704373));
#53583=CARTESIAN_POINT('Ctrl Pts',(0.277777440900717,0.68208727108596,1.90098605679421));
#53584=CARTESIAN_POINT('Ctrl Pts',(-0.0802309646795408,0.732097223286951,
1.91282461654468));
#53585=CARTESIAN_POINT('Ctrl Pts',(-0.418910836519209,0.605736793589845,
1.92466317629516));
#53586=CARTESIAN_POINT('Ctrl Pts',(-0.652509368967175,0.338212972333276,
1.9362945484778));
#53587=CARTESIAN_POINT('Ctrl Pts',(-0.706853190813096,0.110672904517833,
1.94397973407695));
#53588=CARTESIAN_POINT('Ctrl Pts',(-0.706904715465692,-6.20599748754613E-6,
1.94771873309261));
#53589=CARTESIAN_POINT('Ctrl Pts',(-0.7069053169741,-5.78691218945833E-6,
1.82728126690739));
#53590=CARTESIAN_POINT('Ctrl Pts',(-0.706907812244574,-0.00570519928280016,
1.82747380685065));
#53591=CARTESIAN_POINT('Ctrl Pts',(-0.705456723071662,-0.128215175728052,
1.8316125333774));
#53592=CARTESIAN_POINT('Ctrl Pts',(-0.639099702185964,-0.365998534307576,
1.83969744648764));
#53593=CARTESIAN_POINT('Ctrl Pts',(-0.387968339254434,-0.626006329194029,
1.85153600623812));
#53594=CARTESIAN_POINT('Ctrl Pts',(-0.043371078634514,-0.735202221147443,
1.86337456598859));
#53595=CARTESIAN_POINT('Ctrl Pts',(0.311674758291609,-0.667279702605622,
1.87521312573907));
#53596=CARTESIAN_POINT('Ctrl Pts',(0.591634671650319,-0.438602065356417,
1.88705168548954));
#53597=CARTESIAN_POINT('Ctrl Pts',(0.729063197527252,-0.104260301476294,
1.89889024524002));
#53598=CARTESIAN_POINT('Ctrl Pts',(0.690852272129496,0.255198931434154,
1.91072880499049));
#53599=CARTESIAN_POINT('Ctrl Pts',(0.486207333262819,0.553177896624332,
1.92256736474097));
#53600=CARTESIAN_POINT('Ctrl Pts',(0.16442962805144,0.71789014089361,1.93440592449145));
#53601=CARTESIAN_POINT('Ctrl Pts',(-0.196961007662504,0.709654646252797,
1.94624448424192));
#53602=CARTESIAN_POINT('Ctrl Pts',(-0.51090154072052,0.530455439643165,
1.9580830439924));
#53603=CARTESIAN_POINT('Ctrl Pts',(-0.677690936174323,0.262178463108642,
1.96842863821422));
#53604=CARTESIAN_POINT('Ctrl Pts',(-0.706760695067449,0.0726361941522846,
1.97482804585255));
#53605=CARTESIAN_POINT('Ctrl Pts',(-0.706804740303746,-1.18692578732899E-5,
1.97728126690739));
#53606=CARTESIAN_POINT('Origin',(0.,0.,0.522718733092613));
#53607=CARTESIAN_POINT('',(-0.706801622057775,-1.06151464860647E-5,1.64771873309261));
#53608=CARTESIAN_POINT('',(-0.706832438881351,1.728044458367E-5,1.67728126690739));
#53609=CARTESIAN_POINT('',(-0.70685,-2.56204009907072E-14,0.522718733092613));
#53610=CARTESIAN_POINT('Ctrl Pts',(-0.706801622057775,-1.06151464860232E-5,
1.64771873309261));
#53611=CARTESIAN_POINT('Ctrl Pts',(-0.706826402300104,-0.0459865831122182,
1.64927125607315));
#53612=CARTESIAN_POINT('Ctrl Pts',(-0.691176049341311,-0.208807130958488,
1.65476996563718));
#53613=CARTESIAN_POINT('Ctrl Pts',(-0.567544005886828,-0.469358235709884,
1.6642148617847));
#53614=CARTESIAN_POINT('Ctrl Pts',(-0.275851645761568,-0.682868377930474,
1.67605342153517));
#53615=CARTESIAN_POINT('Ctrl Pts',(0.0822964508010132,-0.731867915837495,
1.68789198128565));
#53616=CARTESIAN_POINT('Ctrl Pts',(0.420618414990665,-0.604552314541516,
1.69973054103613));
#53617=CARTESIAN_POINT('Ctrl Pts',(0.657608714291634,-0.331593321607157,
1.7115691007866));
#53618=CARTESIAN_POINT('Ctrl Pts',(0.736173743824141,0.0212501988393111,
1.72340766053708));
#53619=CARTESIAN_POINT('Ctrl Pts',(0.637386312193742,0.36897430950518,1.73524622028755));
#53620=CARTESIAN_POINT('Ctrl Pts',(0.38504541288342,0.627808395980971,1.74708478003803));
#53621=CARTESIAN_POINT('Ctrl Pts',(0.0399427814314016,0.735396441559441,
1.7589233397885));
#53622=CARTESIAN_POINT('Ctrl Pts',(-0.314782511317597,0.665819286755307,
1.77076189953898));
#53623=CARTESIAN_POINT('Ctrl Pts',(-0.5936731881467,0.435838843751334,1.78260045928945));
#53624=CARTESIAN_POINT('Ctrl Pts',(-0.696798799331513,0.181585790695073,
1.791586070474));
#53625=CARTESIAN_POINT('Ctrl Pts',(-0.706864244082333,0.0323879979636773,
1.79662549507505));
#53626=CARTESIAN_POINT('Ctrl Pts',(-0.70683369084198,1.73761920617202E-5,
1.79771873309261));
#53627=CARTESIAN_POINT('Ctrl Pts',(-0.706832438881352,1.72804445836769E-5,
1.67728126690739));
#53628=CARTESIAN_POINT('Ctrl Pts',(-0.706753787487206,-0.0840248346394162,
1.68011956784875));
#53629=CARTESIAN_POINT('Ctrl Pts',(-0.670899552291929,-0.284978893811032,
1.6869040553736));
#53630=CARTESIAN_POINT('Ctrl Pts',(-0.484644460168804,-0.554547656814542,
1.69763472948194));
#53631=CARTESIAN_POINT('Ctrl Pts',(-0.162403256883848,-0.718351264079303,
1.70947328923241));
#53632=CARTESIAN_POINT('Ctrl Pts',(0.198962701325951,-0.709096044222425,
1.72131184898289));
#53633=CARTESIAN_POINT('Ctrl Pts',(0.512396326909379,-0.529011682877222,
1.73315040873336));
#53634=CARTESIAN_POINT('Ctrl Pts',(0.702387965556207,-0.221482510128057,
1.74498896848384));
#53635=CARTESIAN_POINT('Ctrl Pts',(0.723166513641681,0.139404268220684,
1.75682752823431));
#53636=CARTESIAN_POINT('Ctrl Pts',(0.569726187309398,0.46670700438791,1.76866608798479));
#53637=CARTESIAN_POINT('Ctrl Pts',(0.279032471602733,0.681574820721842,
1.78050464773527));
#53638=CARTESIAN_POINT('Ctrl Pts',(-0.0788832769436621,0.732243665093515,
1.79234320748574));
#53639=CARTESIAN_POINT('Ctrl Pts',(-0.417795164746744,0.606506848077444,
1.80418176723622));
#53640=CARTESIAN_POINT('Ctrl Pts',(-0.652180521522544,0.339077101493092,
1.81582778704343));
#53641=CARTESIAN_POINT('Ctrl Pts',(-0.706856670633635,0.111106638562335,
1.82352762026716));
#53642=CARTESIAN_POINT('Ctrl Pts',(-0.7069053169741,-5.78691218945833E-6,
1.82728126690739));
#53643=CARTESIAN_POINT('Origin',(0.,0.,0.522718733092613));
#53644=CARTESIAN_POINT('',(-0.706902657837619,-7.46222082938423E-6,1.49771873309261));
#53645=CARTESIAN_POINT('',(-0.706802357132712,-1.09322218498076E-5,1.52728126690739));
#53646=CARTESIAN_POINT('',(-0.70685,-2.56204009907072E-14,0.522718733092613));
#53647=CARTESIAN_POINT('Ctrl Pts',(-0.706902657837619,-7.46222082939445E-6,
1.49771873309261));
#53648=CARTESIAN_POINT('Ctrl Pts',(-0.706906730846225,-0.00746992783842311,
1.49797083048776));
#53649=CARTESIAN_POINT('Ctrl Pts',(-0.704979296674476,-0.13174339950389,
1.50216911446639));
#53650=CARTESIAN_POINT('Ctrl Pts',(-0.636342616245341,-0.370771394253652,
1.51031358502852));
#53651=CARTESIAN_POINT('Ctrl Pts',(-0.383272352862338,-0.628892403816528,
1.522152144779));
#53652=CARTESIAN_POINT('Ctrl Pts',(-0.0378675072613757,-0.735506222910841,
1.53399070452947));
#53653=CARTESIAN_POINT('Ctrl Pts',(0.316660042955515,-0.664928394071252,
1.54582926427995));
#53654=CARTESIAN_POINT('Ctrl Pts',(0.594900658951714,-0.434161903010362,
1.55766782403042));
#53655=CARTESIAN_POINT('Ctrl Pts',(0.729823074730051,-0.0988009698248782,
1.5695063837809));
#53656=CARTESIAN_POINT('Ctrl Pts',(0.688922976322423,0.260362218345552,
1.58134494353137));
#53657=CARTESIAN_POINT('Ctrl Pts',(0.482053653356788,0.556801245806918,
1.59318350328185));
#53658=CARTESIAN_POINT('Ctrl Pts',(0.159052231749204,0.719100646378767,
1.60502206303232));
#53659=CARTESIAN_POINT('Ctrl Pts',(-0.202266645473739,0.708160685279523,
1.6168606227828));
#53660=CARTESIAN_POINT('Ctrl Pts',(-0.514857233095386,0.526616921087925,
1.62869918253327));
#53661=CARTESIAN_POINT('Ctrl Pts',(-0.678685547138705,0.25865074554612,
1.63898521930321));
#53662=CARTESIAN_POINT('Ctrl Pts',(-0.706763416140776,0.070874648717395,
1.64532506948966));
#53663=CARTESIAN_POINT('Ctrl Pts',(-0.706801622057775,-1.06151464860232E-5,
1.64771873309261));
#53664=CARTESIAN_POINT('Ctrl Pts',(-0.706802357132712,-1.09322218498076E-5,
1.52728126690739));
#53665=CARTESIAN_POINT('Ctrl Pts',(-0.70682767132918,-0.0455529946936496,
1.52881914226335));
#53666=CARTESIAN_POINT('Ctrl Pts',(-0.691368236317636,-0.2079389765849,
1.53430320420281));
#53667=CARTESIAN_POINT('Ctrl Pts',(-0.568406982135528,-0.468312779144872,
1.54373345272576));
#53668=CARTESIAN_POINT('Ctrl Pts',(-0.277108117480876,-0.682359471009978,
1.55557201247623));
#53669=CARTESIAN_POINT('Ctrl Pts',(0.0809491816544183,-0.732018159911551,
1.56741057222671));
#53670=CARTESIAN_POINT('Ctrl Pts',(0.419504920572478,-0.605325514137882,
1.57924913197718));
#53671=CARTESIAN_POINT('Ctrl Pts',(0.656997247819542,-0.33280320432406,
1.59108769172766));
#53672=CARTESIAN_POINT('Ctrl Pts',(0.736211614387408,0.0198951072351811,
1.60292625147813));
#53673=CARTESIAN_POINT('Ctrl Pts',(0.638064396351524,0.367800465686733,
1.61476481122861));
#53674=CARTESIAN_POINT('Ctrl Pts',(0.386200352603368,0.62709859200914,1.62660337097908));
#53675=CARTESIAN_POINT('Ctrl Pts',(0.0412963388606396,0.735321677123366,
1.63844193072956));
#53676=CARTESIAN_POINT('Ctrl Pts',(-0.313556423252151,0.666397573441058,
1.65028049048004));
#53677=CARTESIAN_POINT('Ctrl Pts',(-0.59286994772746,0.436930865850026,
1.66211905023051));
#53678=CARTESIAN_POINT('Ctrl Pts',(-0.696632251283717,0.18245391022506,
1.67111930903963));
#53679=CARTESIAN_POINT('Ctrl Pts',(-0.706863139202462,0.0328217837583204,
1.67617338126525));
#53680=CARTESIAN_POINT('Ctrl Pts',(-0.706832438881352,1.72804445836769E-5,
1.67728126690739));
#53681=CARTESIAN_POINT('Origin',(0.,0.,0.522718733092613));
#53682=CARTESIAN_POINT('',(-0.706837600175146,1.76134468301129E-5,1.34771873309261));
#53683=CARTESIAN_POINT('',(-0.706903367591914,-7.0575322025368E-6,1.37728126690739));
#53684=CARTESIAN_POINT('',(-0.70685,-2.56204009907072E-14,0.522718733092613));
#53685=CARTESIAN_POINT('Ctrl Pts',(-0.706837600175146,1.76134468300899E-5,
1.34771873309261));
#53686=CARTESIAN_POINT('Ctrl Pts',(-0.706754721657063,-0.0857861962986243,
1.35061659148585));
#53687=CARTESIAN_POINT('Ctrl Pts',(-0.669792860630747,-0.288503634206156,
1.35746063646259));
#53688=CARTESIAN_POINT('Ctrl Pts',(-0.480480572542965,-0.558159270688526,
1.36825086802282));
#53689=CARTESIAN_POINT('Ctrl Pts',(-0.157022466269567,-0.719546591356936,
1.38008942777329));
#53690=CARTESIAN_POINT('Ctrl Pts',(0.204264102488947,-0.707587117237976,
1.39192798752377));
#53691=CARTESIAN_POINT('Ctrl Pts',(0.516341171985148,-0.525162018961544,
1.40376654727424));
#53692=CARTESIAN_POINT('Ctrl Pts',(0.704025897392014,-0.216219536231424,
1.41560510702472));
#53693=CARTESIAN_POINT('Ctrl Pts',(0.722102936199932,0.144812643019176,
1.42744366677519));
#53694=CARTESIAN_POINT('Ctrl Pts',(0.566217328251717,0.470957842311017,
1.43928222652567));
#53695=CARTESIAN_POINT('Ctrl Pts',(0.273923654190083,0.683644047529059,
1.45112078627614));
#53696=CARTESIAN_POINT('Ctrl Pts',(-0.0843612816475947,0.73163278098069,
1.46295934602662));
#53697=CARTESIAN_POINT('Ctrl Pts',(-0.422322644344321,0.603363021837419,
1.4747979057771));
#53698=CARTESIAN_POINT('Ctrl Pts',(-0.653511582405244,0.335563154723619,
1.48638436813243));
#53699=CARTESIAN_POINT('Ctrl Pts',(-0.706842974329004,0.109343185930717,
1.49402464390426));
#53700=CARTESIAN_POINT('Ctrl Pts',(-0.706902657837619,-7.46222082939445E-6,
1.49771873309261));
#53701=CARTESIAN_POINT('Ctrl Pts',(-0.706903367591914,-7.05753220258103E-6,
1.37728126690739));
#53702=CARTESIAN_POINT('Ctrl Pts',(-0.706907025380322,-0.00703591082257907,
1.37751871667796));
#53703=CARTESIAN_POINT('Ctrl Pts',(-0.705097952042887,-0.130875652267875,
1.38170235303202));
#53704=CARTESIAN_POINT('Ctrl Pts',(-0.637024010013693,-0.3695994685019,
1.38983217596958));
#53705=CARTESIAN_POINT('Ctrl Pts',(-0.384429290883511,-0.62818586163779,
1.40167073572005));
#53706=CARTESIAN_POINT('Ctrl Pts',(-0.0392212702694481,-0.735435278191946,
1.41350929547053));
#53707=CARTESIAN_POINT('Ctrl Pts',(0.315435591559856,-0.665510138185811,
1.425347855221));
#53708=CARTESIAN_POINT('Ctrl Pts',(0.594100503158886,-0.435256187316358,
1.43718641497148));
#53709=CARTESIAN_POINT('Ctrl Pts',(0.729639980990038,-0.100144169034792,
1.44902497472195));
#53710=CARTESIAN_POINT('Ctrl Pts',(0.689401053958178,0.259093695894295,
1.46086353447243));
#53711=CARTESIAN_POINT('Ctrl Pts',(0.483077728136633,0.555913001313301,
1.47270209422291));
#53712=CARTESIAN_POINT('Ctrl Pts',(0.160375592643109,0.718806667842741,
1.48454065397338));
#53713=CARTESIAN_POINT('Ctrl Pts',(-0.200962810856885,0.708531795407456,
1.49637921372385));
#53714=CARTESIAN_POINT('Ctrl Pts',(-0.51388703304889,0.527563715313158,
1.50821777347433));
#53715=CARTESIAN_POINT('Ctrl Pts',(-0.678442306952803,0.259518385311895,
1.51851845786884));
#53716=CARTESIAN_POINT('Ctrl Pts',(-0.706762715127049,0.0713078908220291,
1.52487295567986));
#53717=CARTESIAN_POINT('Ctrl Pts',(-0.706802357132712,-1.09322218498076E-5,
1.52728126690739));
#53718=CARTESIAN_POINT('Origin',(0.,0.,0.522718733092613));
#53719=CARTESIAN_POINT('',(-0.70679951935905,-9.6117180550407E-6,1.19771873309261));
#53720=CARTESIAN_POINT('',(-0.70683631828199,1.75454709868683E-5,1.22728126690739));
#53721=CARTESIAN_POINT('',(-0.70685,-2.56204009907072E-14,0.522718733092613));
#53722=CARTESIAN_POINT('Ctrl Pts',(-0.70679951935905,-9.61171805506644E-6,
1.19771873309261));
#53723=CARTESIAN_POINT('Ctrl Pts',(-0.706822516721899,-0.0473159294520395,
1.19931616590046));
#53724=CARTESIAN_POINT('Ctrl Pts',(-0.690581482598579,-0.211468896388643,
1.2048597852918));
#53725=CARTESIAN_POINT('Ctrl Pts',(-0.564886142186152,-0.472553698972733,
1.21434959126664));
#53726=CARTESIAN_POINT('Ctrl Pts',(-0.271993481537794,-0.684414273702493,
1.22618815101711));
#53727=CARTESIAN_POINT('Ctrl Pts',(0.0864254407786529,-0.731391820594802,
1.23802671076759));
#53728=CARTESIAN_POINT('Ctrl Pts',(0.42402351100988,-0.602168924935201,
1.24986527051806));
#53729=CARTESIAN_POINT('Ctrl Pts',(0.65946959076411,-0.327876822761505,
1.26170383026854));
#53730=CARTESIAN_POINT('Ctrl Pts',(0.7360420948641,0.02540446092383,1.27354239001901));
#53731=CARTESIAN_POINT('Ctrl Pts',(0.635293853503172,0.372565526784018,
1.28538094976949));
#53732=CARTESIAN_POINT('Ctrl Pts',(0.381496241085932,0.62997140417964,1.29721950951997));
#53733=CARTESIAN_POINT('Ctrl Pts',(0.0357919315763396,0.735610147891393,
1.30905806927044));
#53734=CARTESIAN_POINT('Ctrl Pts',(-0.318535053229798,0.664032206982953,
1.32089662902092));
#53735=CARTESIAN_POINT('Ctrl Pts',(-0.596123392939055,0.432481505312761,
1.33273518877139));
#53736=CARTESIAN_POINT('Ctrl Pts',(-0.697304244243687,0.178924149227873,
1.34167589012862));
#53737=CARTESIAN_POINT('Ctrl Pts',(-0.706867582277473,0.0310579682124794,
1.34667040490236));
#53738=CARTESIAN_POINT('Ctrl Pts',(-0.706837600175146,1.76134468300899E-5,
1.34771873309261));
#53739=CARTESIAN_POINT('Ctrl Pts',(-0.70683631828199,1.75454709868614E-5,
1.22728126690739));
#53740=CARTESIAN_POINT('Ctrl Pts',(-0.706754436578726,-0.0853530034866889,
1.23016447767606));
#53741=CARTESIAN_POINT('Ctrl Pts',(-0.670066454565782,-0.287636803571761,
1.23699387502822));
#53742=CARTESIAN_POINT('Ctrl Pts',(-0.481507149662053,-0.557273919428443,
1.24776945896388));
#53743=CARTESIAN_POINT('Ctrl Pts',(-0.158346651432958,-0.719256348203324,
1.25960801871435));
#53744=CARTESIAN_POINT('Ctrl Pts',(0.202961320248067,-0.707961905001939,
1.27144657846483));
#53745=CARTESIAN_POINT('Ctrl Pts',(0.515373647430983,-0.526111547092912,
1.2832851382153));
#53746=CARTESIAN_POINT('Ctrl Pts',(0.703626717974851,-0.217515052818769,
1.29512369796578));
#53747=CARTESIAN_POINT('Ctrl Pts',(0.722368268691099,0.143483242363127,
1.30696225771625));
#53748=CARTESIAN_POINT('Ctrl Pts',(0.567083251096378,0.469914825023403,
1.31880081746673));
#53749=CARTESIAN_POINT('Ctrl Pts',(0.275181556922342,0.683138688101186,
1.3306393772172));
#53750=CARTESIAN_POINT('Ctrl Pts',(-0.0830144418180345,0.731786826132074,
1.34247793696768));
#53751=CARTESIAN_POINT('Ctrl Pts',(-0.421211336145891,0.604139360373918,
1.35431649671815));
#53752=CARTESIAN_POINT('Ctrl Pts',(-0.653185707793217,0.336427474765252,
1.36591760669806));
#53753=CARTESIAN_POINT('Ctrl Pts',(-0.70684623645849,0.109776863875274,
1.37357253009447));
#53754=CARTESIAN_POINT('Ctrl Pts',(-0.706903367591914,-7.05753220258103E-6,
1.37728126690739));
#53755=CARTESIAN_POINT('Origin',(0.,0.,0.522718733092613));
#53756=CARTESIAN_POINT('',(-0.706900287114882,-8.66958556023345E-6,1.04771873309261));
#53757=CARTESIAN_POINT('',(-0.706800184200881,-9.94400265103002E-6,1.07728126690739));
#53758=CARTESIAN_POINT('',(-0.70685,-2.56204009907072E-14,0.522718733092613));
#53759=CARTESIAN_POINT('Ctrl Pts',(-0.706900287114882,-8.66958556019516E-6,
1.04771873309261));
#53760=CARTESIAN_POINT('Ctrl Pts',(-0.706905729970906,-0.0088006199353823,
1.04801574031507));
#53761=CARTESIAN_POINT('Ctrl Pts',(-0.70461048072898,-0.134403976845368,
1.05225893412102));
#53762=CARTESIAN_POINT('Ctrl Pts',(-0.634240032318171,-0.374356692787108,
1.06044831451046));
#53763=CARTESIAN_POINT('Ctrl Pts',(-0.379717091696098,-0.631045388490867,
1.07228687426093));
#53764=CARTESIAN_POINT('Ctrl Pts',(-0.0337160709028718,-0.73570821566756,
1.08412543401141));
#53765=CARTESIAN_POINT('Ctrl Pts',(0.320407527210959,-0.663130732629247,
1.09596399376188));
#53766=CARTESIAN_POINT('Ctrl Pts',(0.597341380372839,-0.430797664036932,
1.10780255351236));
#53767=CARTESIAN_POINT('Ctrl Pts',(0.730369036319385,-0.094680635997126,
1.11964111326283));
#53768=CARTESIAN_POINT('Ctrl Pts',(0.687442649847106,0.264246012681654,
1.13147967301331));
#53769=CARTESIAN_POINT('Ctrl Pts',(0.478903665966244,0.559512851300696,
1.14331823276378));
#53770=CARTESIAN_POINT('Ctrl Pts',(0.154991450519341,0.719986807040808,
1.15515679251426));
#53771=CARTESIAN_POINT('Ctrl Pts',(-0.206259933078302,0.707007915127706,
1.16699535226474));
#53772=CARTESIAN_POINT('Ctrl Pts',(-0.51782099957674,0.523702935302196,
1.17883391201521));
#53773=CARTESIAN_POINT('Ctrl Pts',(-0.679425760049597,0.255990445315929,
1.18907503895784));
#53774=CARTESIAN_POINT('Ctrl Pts',(-0.706765705640842,0.0695462981414409,
1.19536997931697));
#53775=CARTESIAN_POINT('Ctrl Pts',(-0.70679951935905,-9.61171805506644E-6,
1.19771873309261));
#53776=CARTESIAN_POINT('Ctrl Pts',(-0.706800184200881,-9.94400265104389E-6,
1.07728126690739));
#53777=CARTESIAN_POINT('Ctrl Pts',(-0.706823787147948,-0.0468823619700862,
1.07886405209067));
#53778=CARTESIAN_POINT('Ctrl Pts',(-0.690776290670716,-0.21060074762263,
1.08439302385743));
#53779=CARTESIAN_POINT('Ctrl Pts',(-0.565755004731942,-0.471513129267208,
1.09386818220769));
#53780=CARTESIAN_POINT('Ctrl Pts',(-0.273252805267132,-0.683912465791199,
1.10570674195817));
#53781=CARTESIAN_POINT('Ctrl Pts',(0.0850790409901614,-0.7315496655969,
1.11754530170865));
#53782=CARTESIAN_POINT('Ctrl Pts',(0.422914397879838,-0.602948396230368,
1.12938386145912));
#53783=CARTESIAN_POINT('Ctrl Pts',(0.658864962009067,-0.329090137025705,
1.14122242120959));
#53784=CARTESIAN_POINT('Ctrl Pts',(0.736087612291053,0.0240496046218443,
1.15306098096007));
#53785=CARTESIAN_POINT('Ctrl Pts',(0.635978551456582,0.371395528430276,
1.16489954071055));
#53786=CARTESIAN_POINT('Ctrl Pts',(0.382655168196356,0.629268129419748,
1.17673810046102));
#53787=CARTESIAN_POINT('Ctrl Pts',(0.0371458893840861,0.735543023454563,
1.1885766602115));
#53788=CARTESIAN_POINT('Ctrl Pts',(-0.317312248253455,0.664617403894264,
1.20041521996197));
#53789=CARTESIAN_POINT('Ctrl Pts',(-0.595326328143767,0.433578043112969,
1.21225377971245));
#53790=CARTESIAN_POINT('Ctrl Pts',(-0.697140254592215,0.179792257193208,
1.22120912869425));
#53791=CARTESIAN_POINT('Ctrl Pts',(-0.706866506248542,0.0314917719916984,
1.22621829109257));
#53792=CARTESIAN_POINT('Ctrl Pts',(-0.70683631828199,1.75454709868614E-5,
1.22728126690739));
#53793=CARTESIAN_POINT('Origin',(0.,0.,0.522718733092613));
#53794=CARTESIAN_POINT('',(-0.706841592163942,1.78676093792155E-5,0.897718733092612));
#53795=CARTESIAN_POINT('',(-0.70690109581483,-8.28105672090462E-6,0.927281266907388));
#53796=CARTESIAN_POINT('',(-0.70685,-2.56204009907072E-14,0.522718733092613));
#53797=CARTESIAN_POINT('Ctrl Pts',(-0.706841592163942,1.7867609379222E-5,
0.897718733092612));
#53798=CARTESIAN_POINT('Ctrl Pts',(-0.706755847239672,-0.0871142953232393,
0.900661501313167));
#53799=CARTESIAN_POINT('Ctrl Pts',(-0.668948275249204,-0.291161300644555,
0.907550456117214));
#53800=CARTESIAN_POINT('Ctrl Pts',(-0.47732294727357,-0.560861892554869,
0.918385597504754));
#53801=CARTESIAN_POINT('Ctrl Pts',(-0.152959200118396,-0.720421332568536,
0.930224157255227));
#53802=CARTESIAN_POINT('Ctrl Pts',(0.20825412107116,-0.70642306199211,0.942062717005705));
#53803=CARTESIAN_POINT('Ctrl Pts',(0.519296704228398,-0.522239692636662,
0.953901276756179));
#53804=CARTESIAN_POINT('Ctrl Pts',(0.705234922034154,-0.212242913538608,
0.965739836506655));
#53805=CARTESIAN_POINT('Ctrl Pts',(0.721274186030318,0.148885525939063,
0.97757839625713));
#53806=CARTESIAN_POINT('Ctrl Pts',(0.563550458271255,0.474145794399759,
0.989416956007605));
#53807=CARTESIAN_POINT('Ctrl Pts',(0.270061143182683,0.68517904960402,1.00125551575808));
#53808=CARTESIAN_POINT('Ctrl Pts',(-0.0884889117632597,0.731145036959546,
1.01309407550856));
#53809=CARTESIAN_POINT('Ctrl Pts',(-0.425721001442049,0.600970033160064,
1.02493263525903));
#53810=CARTESIAN_POINT('Ctrl Pts',(-0.654504697899648,0.332912764005127,
1.03647418778705));
#53811=CARTESIAN_POINT('Ctrl Pts',(-0.706833413462098,0.108013632008419,
1.04406955373158));
#53812=CARTESIAN_POINT('Ctrl Pts',(-0.706900287114882,-8.66958556019516E-6,
1.04771873309261));
#53813=CARTESIAN_POINT('Ctrl Pts',(-0.70690109581483,-8.28105672094105E-6,
0.927281266907388));
#53814=CARTESIAN_POINT('Ctrl Pts',(-0.706906076802844,-0.00836660754601505,
0.927563626505272));
#53815=CARTESIAN_POINT('Ctrl Pts',(-0.704731608357342,-0.133536203475843,
0.931792172686647));
#53816=CARTESIAN_POINT('Ctrl Pts',(-0.63492802922278,-0.373188632550485,
0.939966905451515));
#53817=CARTESIAN_POINT('Ctrl Pts',(-0.380877998557793,-0.630345386040242,
0.951805465201989));
#53818=CARTESIAN_POINT('Ctrl Pts',(-0.0350702127852755,-0.735644912405828,
0.963644024952465));
#53819=CARTESIAN_POINT('Ctrl Pts',(0.319186378418513,-0.663719377496494,
0.97548258470294));
#53820=CARTESIAN_POINT('Ctrl Pts',(0.596547412907388,-0.43189644669194,
0.987321144453416));
#53821=CARTESIAN_POINT('Ctrl Pts',(0.730193525854251,-0.0960248470611938,
0.99915970420389));
#53822=CARTESIAN_POINT('Ctrl Pts',(0.68792787877927,0.262980208441528,1.01099826395437));
#53823=CARTESIAN_POINT('Ctrl Pts',(0.47993273725243,0.558630400335474,1.02283682370484));
#53824=CARTESIAN_POINT('Ctrl Pts',(0.156316449407645,0.71970030157465,1.03467538345532));
#53825=CARTESIAN_POINT('Ctrl Pts',(-0.204958213586156,0.707386377546527,
1.04651394320579));
#53826=CARTESIAN_POINT('Ctrl Pts',(-0.516856158218931,0.524655189777677,
1.05835250295627));
#53827=CARTESIAN_POINT('Ctrl Pts',(-0.679185260542492,0.256858137567063,
1.06860827752347));
#53828=CARTESIAN_POINT('Ctrl Pts',(-0.706764940480673,0.0699795526303456,
1.07491786550717));
#53829=CARTESIAN_POINT('Ctrl Pts',(-0.706800184200881,-9.94400265104389E-6,
1.07728126690739));
#53830=CARTESIAN_POINT('Origin',(1.87600653078293E-16,4.24518889064203E-17,
2.1475));
#53831=CARTESIAN_POINT('',(0.418139433688265,0.673212941048267,2.1475));
#53832=CARTESIAN_POINT('Ctrl Pts',(0.347825520797284,-0.615372974259056,
2.1475));
#53833=CARTESIAN_POINT('Ctrl Pts',(0.366504384047157,-0.606234343800672,
2.1475));
#53834=CARTESIAN_POINT('Ctrl Pts',(0.384749844785911,-0.596282384617426,
2.1475));
#53835=CARTESIAN_POINT('Ctrl Pts',(0.402505152806889,-0.585540595271413,
2.1475));
#53836=CARTESIAN_POINT('Ctrl Pts',(0.428009251227577,-0.570110862800913,
2.1475));
#53837=CARTESIAN_POINT('Ctrl Pts',(0.452502861659596,-0.553052634814332,
2.1475));
#53838=CARTESIAN_POINT('Ctrl Pts',(0.475875172607634,-0.534507449294233,
2.1475));
#53839=CARTESIAN_POINT('Ctrl Pts',(0.483690013455006,-0.528306621586319,
2.1475));
#53840=CARTESIAN_POINT('Ctrl Pts',(0.49137937742968,-0.52193932807035,2.1475));
#53841=CARTESIAN_POINT('Ctrl Pts',(0.498938722077998,-0.515410220415254,
2.1475));
#53842=CARTESIAN_POINT('Ctrl Pts',(0.506291908151787,-0.509059174694062,
2.1475));
#53843=CARTESIAN_POINT('Ctrl Pts',(0.513516097025268,-0.502560044328262,
2.1475));
#53844=CARTESIAN_POINT('Ctrl Pts',(0.520602202220868,-0.495922947505538,
2.1475));
#53845=CARTESIAN_POINT('Ctrl Pts',(0.546097282072312,-0.472043353736282,
2.1475));
#53846=CARTESIAN_POINT('Ctrl Pts',(0.569829953644379,-0.446361692321662,
2.1475));
#53847=CARTESIAN_POINT('Ctrl Pts',(0.591620827976965,-0.419094425996583,
2.1475));
#53848=CARTESIAN_POINT('Ctrl Pts',(0.602803004994532,-0.4051019907148,2.1475));
#53849=CARTESIAN_POINT('Ctrl Pts',(0.613473370194027,-0.390691282161003,
2.1475));
#53850=CARTESIAN_POINT('Ctrl Pts',(0.623603958795138,-0.375887559258075,
2.1475));
#53851=CARTESIAN_POINT('Ctrl Pts',(0.628606813990278,-0.368576939416676,
2.1475));
#53852=CARTESIAN_POINT('Ctrl Pts',(0.633473720251848,-0.361176490586554,
2.1475));
#53853=CARTESIAN_POINT('Ctrl Pts',(0.638197570377914,-0.353696641187965,
2.1475));
#53854=CARTESIAN_POINT('Ctrl Pts',(0.642548760340772,-0.34680687018375,
2.1475));
#53855=CARTESIAN_POINT('Ctrl Pts',(0.646779785634514,-0.339847969614829,
2.1475));
#53856=CARTESIAN_POINT('Ctrl Pts',(0.650888589541644,-0.332822744658013,
2.1475));
#53857=CARTESIAN_POINT('Ctrl Pts',(0.668513875925227,-0.30268706416031,
2.1475));
#53858=CARTESIAN_POINT('Ctrl Pts',(0.683893435765135,-0.271333802424689,
2.1475));
#53859=CARTESIAN_POINT('Ctrl Pts',(0.696998727473395,-0.239040247593054,
2.1475));
#53860=CARTESIAN_POINT('Ctrl Pts',(0.706401272193133,-0.215870859209857,
2.1475));
#53861=CARTESIAN_POINT('Ctrl Pts',(0.714632351997429,-0.192216505193648,
2.1475));
#53862=CARTESIAN_POINT('Ctrl Pts',(0.721667468561761,-0.168170826670213,
2.1475));
#53863=CARTESIAN_POINT('Ctrl Pts',(0.724957297731772,-0.156926354187669,
2.1475));
#53864=CARTESIAN_POINT('Ctrl Pts',(0.727985421385293,-0.1455962292866,2.1475));
#53865=CARTESIAN_POINT('Ctrl Pts',(0.730748372576983,-0.13418971384335,
2.1475));
#53866=CARTESIAN_POINT('Ctrl Pts',(0.732573304081957,-0.126655701133689,
2.1475));
#53867=CARTESIAN_POINT('Ctrl Pts',(0.734282538299918,-0.119088358725395,
2.1475));
#53868=CARTESIAN_POINT('Ctrl Pts',(0.735874921113159,-0.111490329588116,
2.1475));
#53869=CARTESIAN_POINT('Ctrl Pts',(0.737355097989788,-0.104427689283639,
2.1475));
#53870=CARTESIAN_POINT('Ctrl Pts',(0.738732308322656,-0.0973480380322194,
2.1475));
#53871=CARTESIAN_POINT('Ctrl Pts',(0.74000621129757,-0.090254603420933,
2.1475));
#53872=CARTESIAN_POINT('Ctrl Pts',(0.746406749010265,-0.0546146868526241,
2.1475));
#53873=CARTESIAN_POINT('Ctrl Pts',(0.750204865999736,-0.0186215654781291,
2.1475));
#53874=CARTESIAN_POINT('Ctrl Pts',(0.751350950426485,0.0174402270492316,
2.1475));
#53875=CARTESIAN_POINT('Ctrl Pts',(0.75235059886048,0.0488943796278962,
2.1475));
#53876=CARTESIAN_POINT('Ctrl Pts',(0.751332104048278,0.0804017898196976,
2.1475));
#53877=CARTESIAN_POINT('Ctrl Pts',(0.748351764615436,0.111783286065349,
2.1475));
#53878=CARTESIAN_POINT('Ctrl Pts',(0.746587659322543,0.130358439960856,
2.1475));
#53879=CARTESIAN_POINT('Ctrl Pts',(0.744135577432054,0.148889565682442,
2.1475));
#53880=CARTESIAN_POINT('Ctrl Pts',(0.741001939024339,0.167339239948629,
2.1475));
#53881=CARTESIAN_POINT('Ctrl Pts',(0.739443648103443,0.176513865786667,
2.1475));
#53882=CARTESIAN_POINT('Ctrl Pts',(0.737715946431412,0.185671312975827,
2.1475));
#53883=CARTESIAN_POINT('Ctrl Pts',(0.735824903550453,0.194782575820964,
2.1475));
#53884=CARTESIAN_POINT('Ctrl Pts',(0.728435000820851,0.23038798003859,2.1475));
#53885=CARTESIAN_POINT('Ctrl Pts',(0.718543897721654,0.265363085334939,
2.1475));
#53886=CARTESIAN_POINT('Ctrl Pts',(0.706253565541109,0.29944106174563,2.1475));
#53887=CARTESIAN_POINT('Ctrl Pts',(0.695958937871222,0.327985455317563,
2.1475));
#53888=CARTESIAN_POINT('Ctrl Pts',(0.683979973451509,0.355900995416786,
2.1475));
#53889=CARTESIAN_POINT('Ctrl Pts',(0.670348680947668,0.383027498229693,
2.1475));
#53890=CARTESIAN_POINT('Ctrl Pts',(0.662930091155104,0.397790617487756,
2.1475));
#53891=CARTESIAN_POINT('Ctrl Pts',(0.655021659947315,0.412319921069258,
2.1475));
#53892=CARTESIAN_POINT('Ctrl Pts',(0.646640126270176,0.426597056225371,
2.1475));
#53893=CARTESIAN_POINT('Ctrl Pts',(0.641911494744018,0.434651824481754,
2.1475));
#53894=CARTESIAN_POINT('Ctrl Pts',(0.637032242582384,0.44262631047491,2.1475));
#53895=CARTESIAN_POINT('Ctrl Pts',(0.632005108758899,0.450517044624497,
2.1475));
#53896=CARTESIAN_POINT('Ctrl Pts',(0.628031056722689,0.456754831247137,
2.1475));
#53897=CARTESIAN_POINT('Ctrl Pts',(0.623965446459039,0.462938715871801,
2.1475));
#53898=CARTESIAN_POINT('Ctrl Pts',(0.619816661607203,0.469057313504708,
2.1475));
#53899=CARTESIAN_POINT('Ctrl Pts',(0.599259679759847,0.499374600364076,
2.1475));
#53900=CARTESIAN_POINT('Ctrl Pts',(0.576621974739516,0.52815831445839,2.1475));
#53901=CARTESIAN_POINT('Ctrl Pts',(0.552123780088927,0.555233296369141,
2.1475));
#53902=CARTESIAN_POINT('Ctrl Pts',(0.527504999689496,0.582441547568308,
2.1475));
#53903=CARTESIAN_POINT('Ctrl Pts',(0.501006647273973,0.607925183051395,
2.1475));
#53904=CARTESIAN_POINT('Ctrl Pts',(0.472807519465647,0.631480354457914,
2.1475));
#53905=CARTESIAN_POINT('Ctrl Pts',(0.455234045944165,0.646159751062663,
2.1475));
#53906=CARTESIAN_POINT('Ctrl Pts',(0.436999200557785,0.66008962575319,2.1475));
#53907=CARTESIAN_POINT('Ctrl Pts',(0.418139433688274,0.673212941048261,
2.1475));
#53908=CARTESIAN_POINT('',(-0.7925,-9.70532588324278E-17,2.1475));
#53909=CARTESIAN_POINT('Origin',(0.,0.,2.1475));
#53910=CARTESIAN_POINT('',(-0.269045505528518,0.74544573781992,2.1475));
#53911=CARTESIAN_POINT('Origin',(0.,0.,2.1475));
#53912=CARTESIAN_POINT('Ctrl Pts',(-0.26905776807643,0.745453775914814,
2.1475));
#53913=CARTESIAN_POINT('Ctrl Pts',(-0.290441959207503,0.736475484699571,
2.1475));
#53914=CARTESIAN_POINT('Ctrl Pts',(-0.311396350827975,0.726569175411544,
2.1475));
#53915=CARTESIAN_POINT('Ctrl Pts',(-0.331855269122231,0.715747333928717,
2.1475));
#53916=CARTESIAN_POINT('Ctrl Pts',(-0.360321255985201,0.700690115699845,
2.1475));
#53917=CARTESIAN_POINT('Ctrl Pts',(-0.387829046120874,0.683861250117464,
2.1475));
#53918=CARTESIAN_POINT('Ctrl Pts',(-0.414237112173797,0.665381488245243,
2.1475));
#53919=CARTESIAN_POINT('Ctrl Pts',(-0.423486150408677,0.658909222393396,
2.1475));
#53920=CARTESIAN_POINT('Ctrl Pts',(-0.432600109161616,0.652234251657612,
2.1475));
#53921=CARTESIAN_POINT('Ctrl Pts',(-0.441572263629033,0.645361178051106,
2.1475));
#53922=CARTESIAN_POINT('Ctrl Pts',(-0.448544286378795,0.64002029524315,
2.1475));
#53923=CARTESIAN_POINT('Ctrl Pts',(-0.455427404303372,0.634562177123534,
2.1475));
#53924=CARTESIAN_POINT('Ctrl Pts',(-0.462212578349833,0.628994443678651,
2.1475));
#53925=CARTESIAN_POINT('Ctrl Pts',(-0.491850576505366,0.604674290291282,
2.1475));
#53926=CARTESIAN_POINT('Ctrl Pts',(-0.51966025566805,0.578238020468965,
2.1475));
#53927=CARTESIAN_POINT('Ctrl Pts',(-0.545395837156543,0.549886756197395,
2.1475));
#53928=CARTESIAN_POINT('Ctrl Pts',(-0.556375006365601,0.537791699092607,
2.1475));
#53929=CARTESIAN_POINT('Ctrl Pts',(-0.56697609741352,0.525347612886411,
2.1475));
#53930=CARTESIAN_POINT('Ctrl Pts',(-0.577177055036603,0.512568207937034,
2.1475));
#53931=CARTESIAN_POINT('Ctrl Pts',(-0.583958944968145,0.504072092085993,
2.1475));
#53932=CARTESIAN_POINT('Ctrl Pts',(-0.590566362811514,0.495424056770332,
2.1475));
#53933=CARTESIAN_POINT('Ctrl Pts',(-0.596976043364239,0.486651310852331,
2.1475));
#53934=CARTESIAN_POINT('Ctrl Pts',(-0.603524360378642,0.477688817185865,
2.1475));
#53935=CARTESIAN_POINT('Ctrl Pts',(-0.609869779183852,0.468592114455762,
2.1475));
#53936=CARTESIAN_POINT('Ctrl Pts',(-0.616006748809266,0.459366327752623,
2.1475));
#53937=CARTESIAN_POINT('Ctrl Pts',(-0.636008881653145,0.429296859841088,
2.1475));
#53938=CARTESIAN_POINT('Ctrl Pts',(-0.653800269885214,0.397857951627114,
2.1475));
#53939=CARTESIAN_POINT('Ctrl Pts',(-0.66930133326429,0.365313993663925,
2.1475));
#53940=CARTESIAN_POINT('Ctrl Pts',(-0.679860140869924,0.343146134436731,
2.1475));
#53941=CARTESIAN_POINT('Ctrl Pts',(-0.689355332541431,0.320464886542413,
2.1475));
#53942=CARTESIAN_POINT('Ctrl Pts',(-0.697748537607775,0.2973497108852,2.1475));
#53943=CARTESIAN_POINT('Ctrl Pts',(-0.70436467793553,0.279128632686827,
2.1475));
#53944=CARTESIAN_POINT('Ctrl Pts',(-0.710295869028216,0.26063783511346,
2.1475));
#53945=CARTESIAN_POINT('Ctrl Pts',(-0.715518243297554,0.241916050684857,
2.1475));
#53946=CARTESIAN_POINT('Ctrl Pts',(-0.717479128438073,0.23488643790785,
2.1475));
#53947=CARTESIAN_POINT('Ctrl Pts',(-0.719339678282086,0.2278250821791,2.1475));
#53948=CARTESIAN_POINT('Ctrl Pts',(-0.721095798426092,0.220746636408961,
2.1475));
#53949=CARTESIAN_POINT('Ctrl Pts',(-0.729648138435318,0.186274464804014,
2.1475));
#53950=CARTESIAN_POINT('Ctrl Pts',(-0.735750164426192,0.151319796048384,
2.1475));
#53951=CARTESIAN_POINT('Ctrl Pts',(-0.739309420613415,0.116128196525184,
2.1475));
#53952=CARTESIAN_POINT('Ctrl Pts',(-0.739584191889496,0.113411437685793,
2.1475));
#53953=CARTESIAN_POINT('Ctrl Pts',(-0.739843783453088,0.110693263463404,
2.1475));
#53954=CARTESIAN_POINT('Ctrl Pts',(-0.740088139783114,0.107973785712775,
2.1475));
#53955=CARTESIAN_POINT('Ctrl Pts',(-0.742817047135923,0.0776033720276509,
2.1475));
#53956=CARTESIAN_POINT('Ctrl Pts',(-0.74364816402632,0.0470699923217768,
2.1475));
#53957=CARTESIAN_POINT('Ctrl Pts',(-0.742599986958386,0.0165488238822319,
2.1475));
#53958=CARTESIAN_POINT('Ctrl Pts',(-0.7419704156394,-0.00178324315047445,
2.1475));
#53959=CARTESIAN_POINT('Ctrl Pts',(-0.740662321376881,-0.020110842121331,
2.1475));
#53960=CARTESIAN_POINT('Ctrl Pts',(-0.738674988083457,-0.038394449672262,
2.1475));
#53961=CARTESIAN_POINT('Ctrl Pts',(-0.737624385864582,-0.0480600647583613,
2.1475));
#53962=CARTESIAN_POINT('Ctrl Pts',(-0.736383083229925,-0.0577174697986878,
2.1475));
#53963=CARTESIAN_POINT('Ctrl Pts',(-0.734955315195305,-0.0673329290467907,
2.1475));
#53964=CARTESIAN_POINT('Ctrl Pts',(-0.729825818210465,-0.101878084859947,
2.1475));
#53965=CARTESIAN_POINT('Ctrl Pts',(-0.722288379849397,-0.13594922305856,
2.1475));
#53966=CARTESIAN_POINT('Ctrl Pts',(-0.712387643908391,-0.169286210566026,
2.1475));
#53967=CARTESIAN_POINT('Ctrl Pts',(-0.704219970383048,-0.196787765188011,
2.1475));
#53968=CARTESIAN_POINT('Ctrl Pts',(-0.694442927041613,-0.223789957726689,
2.1475));
#53969=CARTESIAN_POINT('Ctrl Pts',(-0.683056846723072,-0.250136548529342,
2.1475));
#53970=CARTESIAN_POINT('Ctrl Pts',(-0.676729068714859,-0.264778582768371,
2.1475));
#53971=CARTESIAN_POINT('Ctrl Pts',(-0.669903919231193,-0.279217909485822,
2.1475));
#53972=CARTESIAN_POINT('Ctrl Pts',(-0.662594838107065,-0.293431932187759,
2.1475));
#53973=CARTESIAN_POINT('Ctrl Pts',(-0.658703530129136,-0.300999386837555,
2.1475));
#53974=CARTESIAN_POINT('Ctrl Pts',(-0.654675027469965,-0.308502953737097,
2.1475));
#53975=CARTESIAN_POINT('Ctrl Pts',(-0.650511183593094,-0.315939021603285,
2.1475));
#53976=CARTESIAN_POINT('Ctrl Pts',(-0.647373225960974,-0.321542993943189,
2.1475));
#53977=CARTESIAN_POINT('Ctrl Pts',(-0.644159097881625,-0.327107209853852,
2.1475));
#53978=CARTESIAN_POINT('Ctrl Pts',(-0.640874688920018,-0.332622176281529,
2.1475));
#53979=CARTESIAN_POINT('Ctrl Pts',(-0.623260408432555,-0.36219893321759,
2.1475));
#53980=CARTESIAN_POINT('Ctrl Pts',(-0.60359160098753,-0.390427811114693,
2.1475));
#53981=CARTESIAN_POINT('Ctrl Pts',(-0.58204045909045,-0.417108106849397,
2.1475));
#53982=CARTESIAN_POINT('Ctrl Pts',(-0.560812811764996,-0.443387916573627,
2.1475));
#53983=CARTESIAN_POINT('Ctrl Pts',(-0.537758021946897,-0.46816609483233,
2.1475));
#53984=CARTESIAN_POINT('Ctrl Pts',(-0.513006243791438,-0.491215307380577,
2.1475));
#53985=CARTESIAN_POINT('Ctrl Pts',(-0.498618300449934,-0.504613567583442,
2.1475));
#53986=CARTESIAN_POINT('Ctrl Pts',(-0.483656376131934,-0.517426889096619,
2.1475));
#53987=CARTESIAN_POINT('Ctrl Pts',(-0.468142317532559,-0.529603335559025,
2.1475));
#53988=CARTESIAN_POINT('Ctrl Pts',(-0.308141029750816,0.636149375763356,
0.750549949443909));
#53989=CARTESIAN_POINT('Ctrl Pts',(-0.413294916605362,0.585214440963209,
0.7544961360274));
#53990=CARTESIAN_POINT('Ctrl Pts',(-0.597758033783181,0.430253045149882,
0.762388509194384));
#53991=CARTESIAN_POINT('Ctrl Pts',(-0.730464614175445,0.0939443613281403,
0.774227068944859));
#53992=CARTESIAN_POINT('Ctrl Pts',(-0.687181523831969,-0.264910506517124,
0.786065628695335));
#53993=CARTESIAN_POINT('Ctrl Pts',(-0.478355287135876,-0.559987389938686,
0.79790418844581));
#53994=CARTESIAN_POINT('Ctrl Pts',(-0.154284606478325,-0.720136019609621,
0.809742748196285));
#53995=CARTESIAN_POINT('Ctrl Pts',(0.206953274654826,-0.706806483749897,
0.821581307946761));
#53996=CARTESIAN_POINT('Ctrl Pts',(0.518334654870034,-0.523194014936019,
0.833419867697235));
#53997=CARTESIAN_POINT('Ctrl Pts',(0.704843009111363,-0.213540991323109,
0.845258427447713));
#53998=CARTESIAN_POINT('Ctrl Pts',(0.72154704261594,0.147557810200025,0.857096987198186));
#53999=CARTESIAN_POINT('Ctrl Pts',(0.564422240537776,0.473107596474913,
0.868935546948663));
#54000=CARTESIAN_POINT('Ctrl Pts',(0.271321884484909,0.684680839711599,
0.880774106699136));
#54001=CARTESIAN_POINT('Ctrl Pts',(-0.0871429660742197,0.731306659067973,
0.892612666449614));
#54002=CARTESIAN_POINT('Ctrl Pts',(-0.424614090524265,0.601752641869639,
0.904451226200088));
#54003=CARTESIAN_POINT('Ctrl Pts',(-0.659790954477945,0.327229660076594,
0.916289785950563));
#54004=CARTESIAN_POINT('Ctrl Pts',(-0.736016819052472,-0.026126571618046,
0.928128345701039));
#54005=CARTESIAN_POINT('Ctrl Pts',(-0.63492802922278,-0.373188632550485,
0.939966905451515));
#54006=CARTESIAN_POINT('Ctrl Pts',(-0.380877998557793,-0.630345386040242,
0.951805465201989));
#54007=CARTESIAN_POINT('Ctrl Pts',(-0.0350702127852755,-0.735644912405828,
0.963644024952465));
#54008=CARTESIAN_POINT('Ctrl Pts',(0.319186378418513,-0.663719377496494,
0.97548258470294));
#54009=CARTESIAN_POINT('Ctrl Pts',(0.596547412907388,-0.43189644669194,
0.987321144453416));
#54010=CARTESIAN_POINT('Ctrl Pts',(0.730193525854251,-0.0960248470611938,
0.99915970420389));
#54011=CARTESIAN_POINT('Ctrl Pts',(0.68792787877927,0.262980208441528,1.01099826395437));
#54012=CARTESIAN_POINT('Ctrl Pts',(0.47993273725243,0.558630400335474,1.02283682370484));
#54013=CARTESIAN_POINT('Ctrl Pts',(0.156316449407645,0.71970030157465,1.03467538345532));
#54014=CARTESIAN_POINT('Ctrl Pts',(-0.204958213586156,0.707386377546527,
1.04651394320579));
#54015=CARTESIAN_POINT('Ctrl Pts',(-0.516856158218931,0.524655189777677,
1.05835250295627));
#54016=CARTESIAN_POINT('Ctrl Pts',(-0.704237692836986,0.215528718361633,
1.07019106270674));
#54017=CARTESIAN_POINT('Ctrl Pts',(-0.721960516972989,-0.145521023852598,
1.08202962245722));
#54018=CARTESIAN_POINT('Ctrl Pts',(-0.565755004731942,-0.471513129267208,
1.09386818220769));
#54019=CARTESIAN_POINT('Ctrl Pts',(-0.273252805267132,-0.683912465791199,
1.10570674195817));
#54020=CARTESIAN_POINT('Ctrl Pts',(0.0850790409901614,-0.7315496655969,
1.11754530170865));
#54021=CARTESIAN_POINT('Ctrl Pts',(0.422914397879838,-0.602948396230368,
1.12938386145912));
#54022=CARTESIAN_POINT('Ctrl Pts',(0.658864962009067,-0.329090137025705,
1.14122242120959));
#54023=CARTESIAN_POINT('Ctrl Pts',(0.736087612291053,0.0240496046218443,
1.15306098096007));
#54024=CARTESIAN_POINT('Ctrl Pts',(0.635978551456582,0.371395528430276,
1.16489954071055));
#54025=CARTESIAN_POINT('Ctrl Pts',(0.382655168196356,0.629268129419748,
1.17673810046102));
#54026=CARTESIAN_POINT('Ctrl Pts',(0.0371458893840861,0.735543023454563,
1.1885766602115));
#54027=CARTESIAN_POINT('Ctrl Pts',(-0.317312248253455,0.664617403894264,
1.20041521996197));
#54028=CARTESIAN_POINT('Ctrl Pts',(-0.595326328143767,0.433578043112969,
1.21225377971245));
#54029=CARTESIAN_POINT('Ctrl Pts',(-0.729919659362832,0.0980848985647673,
1.22409233946292));
#54030=CARTESIAN_POINT('Ctrl Pts',(-0.688667208081245,-0.26103799141963,
1.2359308992134));
#54031=CARTESIAN_POINT('Ctrl Pts',(-0.481507149662053,-0.557273919428443,
1.24776945896388));
#54032=CARTESIAN_POINT('Ctrl Pts',(-0.158346651432958,-0.719256348203324,
1.25960801871435));
#54033=CARTESIAN_POINT('Ctrl Pts',(0.202961320248067,-0.707961905001939,
1.27144657846483));
#54034=CARTESIAN_POINT('Ctrl Pts',(0.515373647430983,-0.526111547092912,
1.2832851382153));
#54035=CARTESIAN_POINT('Ctrl Pts',(0.703626717974851,-0.217515052818769,
1.29512369796578));
#54036=CARTESIAN_POINT('Ctrl Pts',(0.722368268691099,0.143483242363127,
1.30696225771625));
#54037=CARTESIAN_POINT('Ctrl Pts',(0.567083251096378,0.469914825023403,
1.31880081746673));
#54038=CARTESIAN_POINT('Ctrl Pts',(0.275181556922342,0.683138688101186,
1.3306393772172));
#54039=CARTESIAN_POINT('Ctrl Pts',(-0.0830144418180345,0.731786826132074,
1.34247793696768));
#54040=CARTESIAN_POINT('Ctrl Pts',(-0.421211336145891,0.604139360373918,
1.35431649671815));
#54041=CARTESIAN_POINT('Ctrl Pts',(-0.657933724269358,0.33094798823964,
1.36615505646863));
#54042=CARTESIAN_POINT('Ctrl Pts',(-0.736152544097779,-0.0219724434048499,
1.3779936162191));
#54043=CARTESIAN_POINT('Ctrl Pts',(-0.637024010013693,-0.3695994685019,
1.38983217596958));
#54044=CARTESIAN_POINT('Ctrl Pts',(-0.384429290883511,-0.62818586163779,
1.40167073572005));
#54045=CARTESIAN_POINT('Ctrl Pts',(-0.0392212702694481,-0.735435278191946,
1.41350929547053));
#54046=CARTESIAN_POINT('Ctrl Pts',(0.315435591559856,-0.665510138185811,
1.425347855221));
#54047=CARTESIAN_POINT('Ctrl Pts',(0.594100503158886,-0.435256187316358,
1.43718641497148));
#54048=CARTESIAN_POINT('Ctrl Pts',(0.729639980990038,-0.100144169034792,
1.44902497472195));
#54049=CARTESIAN_POINT('Ctrl Pts',(0.689401053958178,0.259093695894295,
1.46086353447243));
#54050=CARTESIAN_POINT('Ctrl Pts',(0.483077728136633,0.555913001313301,
1.47270209422291));
#54051=CARTESIAN_POINT('Ctrl Pts',(0.160375592643109,0.718806667842741,
1.48454065397338));
#54052=CARTESIAN_POINT('Ctrl Pts',(-0.200962810856885,0.708531795407456,
1.49637921372385));
#54053=CARTESIAN_POINT('Ctrl Pts',(-0.51388703304889,0.527563715313158,
1.50821777347433));
#54054=CARTESIAN_POINT('Ctrl Pts',(-0.70301014057808,0.219499655341875,
1.52005633322481));
#54055=CARTESIAN_POINT('Ctrl Pts',(-0.722770268647641,-0.141444318407737,
1.53189489297528));
#54056=CARTESIAN_POINT('Ctrl Pts',(-0.568406982135528,-0.468312779144872,
1.54373345272576));
#54057=CARTESIAN_POINT('Ctrl Pts',(-0.277108117480876,-0.682359471009978,
1.55557201247623));
#54058=CARTESIAN_POINT('Ctrl Pts',(0.0809491816544183,-0.732018159911551,
1.56741057222671));
#54059=CARTESIAN_POINT('Ctrl Pts',(0.419504920572478,-0.605325514137882,
1.57924913197718));
#54060=CARTESIAN_POINT('Ctrl Pts',(0.656997247819542,-0.33280320432406,
1.59108769172766));
#54061=CARTESIAN_POINT('Ctrl Pts',(0.736211614387408,0.0198951072351811,
1.60292625147813));
#54062=CARTESIAN_POINT('Ctrl Pts',(0.638064396351524,0.367800465686733,
1.61476481122861));
#54063=CARTESIAN_POINT('Ctrl Pts',(0.386200352603368,0.62709859200914,1.62660337097908));
#54064=CARTESIAN_POINT('Ctrl Pts',(0.0412963388606396,0.735321677123366,
1.63844193072956));
#54065=CARTESIAN_POINT('Ctrl Pts',(-0.313556423252151,0.666397573441058,
1.65028049048004));
#54066=CARTESIAN_POINT('Ctrl Pts',(-0.59286994772746,0.436930865850026,
1.66211905023051));
#54067=CARTESIAN_POINT('Ctrl Pts',(-0.729354492955569,0.102202642120141,
1.67395760998099));
#54068=CARTESIAN_POINT('Ctrl Pts',(-0.69012941057056,-0.257147337369736,
1.68579616973146));
#54069=CARTESIAN_POINT('Ctrl Pts',(-0.484644460168804,-0.554547656814542,
1.69763472948194));
#54070=CARTESIAN_POINT('Ctrl Pts',(-0.162403256883848,-0.718351264079303,
1.70947328923241));
#54071=CARTESIAN_POINT('Ctrl Pts',(0.198962701325951,-0.709096044222425,
1.72131184898289));
#54072=CARTESIAN_POINT('Ctrl Pts',(0.512396326909379,-0.529011682877222,
1.73315040873336));
#54073=CARTESIAN_POINT('Ctrl Pts',(0.702387965556207,-0.221482510128057,
1.74498896848384));
#54074=CARTESIAN_POINT('Ctrl Pts',(0.723166513641681,0.139404268220684,
1.75682752823431));
#54075=CARTESIAN_POINT('Ctrl Pts',(0.569726187309398,0.46670700438791,1.76866608798479));
#54076=CARTESIAN_POINT('Ctrl Pts',(0.279032471602733,0.681574820721842,
1.78050464773527));
#54077=CARTESIAN_POINT('Ctrl Pts',(-0.0788832769436621,0.732243665093515,
1.79234320748574));
#54078=CARTESIAN_POINT('Ctrl Pts',(-0.417795164746744,0.606506848077444,
1.80418176723622));
#54079=CARTESIAN_POINT('Ctrl Pts',(-0.656055540116142,0.334655770507442,
1.81602032698669));
#54080=CARTESIAN_POINT('Ctrl Pts',(-0.736264822689689,-0.0178176126541187,
1.82785888673717));
#54081=CARTESIAN_POINT('Ctrl Pts',(-0.639099702185964,-0.365998534307576,
1.83969744648764));
#54082=CARTESIAN_POINT('Ctrl Pts',(-0.387968339254434,-0.626006329194029,
1.85153600623812));
#54083=CARTESIAN_POINT('Ctrl Pts',(-0.043371078634514,-0.735202221147443,
1.86337456598859));
#54084=CARTESIAN_POINT('Ctrl Pts',(0.311674758291609,-0.667279702605622,
1.87521312573907));
#54085=CARTESIAN_POINT('Ctrl Pts',(0.591634671650319,-0.438602065356417,
1.88705168548954));
#54086=CARTESIAN_POINT('Ctrl Pts',(0.729063197527252,-0.104260301476294,
1.89889024524002));
#54087=CARTESIAN_POINT('Ctrl Pts',(0.690852272129496,0.255198931434154,
1.91072880499049));
#54088=CARTESIAN_POINT('Ctrl Pts',(0.486207333262819,0.553177896624332,
1.92256736474097));
#54089=CARTESIAN_POINT('Ctrl Pts',(0.16442962805144,0.71789014089361,1.93440592449145));
#54090=CARTESIAN_POINT('Ctrl Pts',(-0.196961007662504,0.709654646252797,
1.94624448424192));
#54091=CARTESIAN_POINT('Ctrl Pts',(-0.51090154072052,0.530455439643165,
1.9580830439924));
#54092=CARTESIAN_POINT('Ctrl Pts',(-0.701760198182685,0.223463598644677,
1.96992160374287));
#54093=CARTESIAN_POINT('Ctrl Pts',(-0.723556999886197,-0.137363102616563,
1.98176016349335));
#54094=CARTESIAN_POINT('Ctrl Pts',(-0.571040857364167,-0.465097524278119,
1.99359872324382));
#54095=CARTESIAN_POINT('Ctrl Pts',(-0.280954601492375,-0.680784722238707,
2.0054372829943));
#54096=CARTESIAN_POINT('Ctrl Pts',(0.0768167392428667,-0.732463381911148,
2.01727584274477));
#54097=CARTESIAN_POINT('Ctrl Pts',(0.416082091960603,-0.607683269644344,
2.02911440249525));
#54098=CARTESIAN_POINT('Ctrl Pts',(0.655108589511754,-0.336505836512168,
2.04095296224572));
#54099=CARTESIAN_POINT('Ctrl Pts',(0.736312206455239,0.0157403015675272,
2.0527915219962));
#54100=CARTESIAN_POINT('Ctrl Pts',(0.640129844349537,0.364193045069704,
2.06463008174667));
#54101=CARTESIAN_POINT('Ctrl Pts',(0.389733384979782,0.624910355165805,
2.07646864149715));
#54102=CARTESIAN_POINT('Ctrl Pts',(0.0454451798068112,0.735074392267673,
2.08830720124762));
#54103=CARTESIAN_POINT('Ctrl Pts',(-0.309790030899746,0.668161503213349,
2.1001457609981));
#54104=CARTESIAN_POINT('Ctrl Pts',(-0.590395841023348,0.440259893769033,
2.11198432074857));
#54105=CARTESIAN_POINT('Ctrl Pts',(-0.728763721120245,0.106336890902483,
2.12382288049905));
#54106=CARTESIAN_POINT('Ctrl Pts',(-0.691575347498768,-0.253290127215884,
2.13566144024952));
#54107=CARTESIAN_POINT('Ctrl Pts',(-0.555684412749315,-0.452220591560317,
2.14355381341651));
#54108=CARTESIAN_POINT('Ctrl Pts',(-0.468142317532544,-0.529603335559038,
2.1475));
#54109=CARTESIAN_POINT('Ctrl Pts',(-0.320586989147272,0.661843744693177,
0.767033299629272));
#54110=CARTESIAN_POINT('Ctrl Pts',(-0.429988090360872,0.608851524205057,
0.770979486212764));
#54111=CARTESIAN_POINT('Ctrl Pts',(-0.621901758568509,0.447631165598393,
0.778871859379747));
#54112=CARTESIAN_POINT('Ctrl Pts',(-0.759968419416597,0.0977388177416922,
0.790710419130224));
#54113=CARTESIAN_POINT('Ctrl Pts',(-0.714937104938856,-0.275610364989308,
0.802548978880698));
#54114=CARTESIAN_POINT('Ctrl Pts',(-0.497676279493137,-0.582605540865684,
0.814387538631174));
#54115=CARTESIAN_POINT('Ctrl Pts',(-0.160516233435894,-0.749222648116171,
0.826226098381648));
#54116=CARTESIAN_POINT('Ctrl Pts',(0.215312213597169,-0.735354726108332,
0.838064658132125));
#54117=CARTESIAN_POINT('Ctrl Pts',(0.539270432470003,-0.544326064347384,
0.8499032178826));
#54118=CARTESIAN_POINT('Ctrl Pts',(0.733311945816648,-0.222166011203247,
0.861741777633075));
#54119=CARTESIAN_POINT('Ctrl Pts',(0.75069066299747,0.153517738729713,0.873580337383551));
#54120=CARTESIAN_POINT('Ctrl Pts',(0.587219517141517,0.492216632167575,
0.885418897134026));
#54121=CARTESIAN_POINT('Ctrl Pts',(0.282280701492824,0.7123354170247,0.897257456884501));
#54122=CARTESIAN_POINT('Ctrl Pts',(-0.0906627109725972,0.760844474893665,
0.909096016634976));
#54123=CARTESIAN_POINT('Ctrl Pts',(-0.441764450974809,0.626057710732026,
0.920934576385453));
#54124=CARTESIAN_POINT('Ctrl Pts',(-0.686440217759186,0.34044661812312,
0.932773136135927));
#54125=CARTESIAN_POINT('Ctrl Pts',(-0.765744880428929,-0.0271818359877063,
0.944611695886403));
#54126=CARTESIAN_POINT('Ctrl Pts',(-0.660573067398221,-0.388261894854107,
0.956450255636878));
#54127=CARTESIAN_POINT('Ctrl Pts',(-0.396261837927992,-0.655805329127812,
0.968288815387354));
#54128=CARTESIAN_POINT('Ctrl Pts',(-0.0364867149781318,-0.765357952299986,
0.980127375137828));
#54129=CARTESIAN_POINT('Ctrl Pts',(0.33207846458085,-0.690527311609143,
0.991965934888305));
#54130=CARTESIAN_POINT('Ctrl Pts',(0.620642240152921,-0.449340944892484,
1.00380449463878));
#54131=CARTESIAN_POINT('Ctrl Pts',(0.759686381712126,-0.0999033352603849,
1.01564305438925));
#54132=CARTESIAN_POINT('Ctrl Pts',(0.715713605509338,0.273602101277356,
1.02748161413973));
#54133=CARTESIAN_POINT('Ctrl Pts',(0.499317443552999,0.581193741821753,
1.03932017389021));
#54134=CARTESIAN_POINT('Ctrl Pts',(0.162630143445403,0.748769331227273,
1.05115873364068));
#54135=CARTESIAN_POINT('Ctrl Pts',(-0.213236571084754,0.735958042084906,
1.06299729339116));
#54136=CARTESIAN_POINT('Ctrl Pts',(-0.53773221865205,0.545846256719961,
1.07483585314163));
#54137=CARTESIAN_POINT('Ctrl Pts',(-0.732682180536634,0.224234023460629,
1.08667441289211));
#54138=CARTESIAN_POINT('Ctrl Pts',(-0.751120837775958,-0.151398685635141,
1.09851297264258));
#54139=CARTESIAN_POINT('Ctrl Pts',(-0.588606112300871,-0.490557763688342,
1.11035153239306));
#54140=CARTESIAN_POINT('Ctrl Pts',(-0.284289613062813,-0.711536008124563,
1.12219009214353));
#54141=CARTESIAN_POINT('Ctrl Pts',(0.0885154229952094,-0.761097296569231,
1.13402865189401));
#54142=CARTESIAN_POINT('Ctrl Pts',(0.439996106954563,-0.627301762167098,
1.14586721164448));
#54143=CARTESIAN_POINT('Ctrl Pts',(0.685476824024146,-0.342382240600841,
1.15770577139496));
#54144=CARTESIAN_POINT('Ctrl Pts',(0.765818533039317,0.0250209793292831,
1.16954433114543));
#54145=CARTESIAN_POINT('Ctrl Pts',(0.661666020713264,0.386396366425159,
1.18138289089591));
#54146=CARTESIAN_POINT('Ctrl Pts',(0.398110788274175,0.654684561611774,
1.19322145064639));
#54147=CARTESIAN_POINT('Ctrl Pts',(0.0386462291194138,0.765251948006628,
1.20506001039686));
#54148=CARTESIAN_POINT('Ctrl Pts',(-0.330128637427446,0.691461609710464,
1.21689857014734));
#54149=CARTESIAN_POINT('Ctrl Pts',(-0.619371835208214,0.451090461774462,
1.22873712989781));
#54150=CARTESIAN_POINT('Ctrl Pts',(-0.759401453625842,0.102046593201571,
1.24057568964829));
#54151=CARTESIAN_POINT('Ctrl Pts',(-0.716482796665414,-0.271581437207322,
1.25241424939876));
#54152=CARTESIAN_POINT('Ctrl Pts',(-0.500955447211536,-0.57978247202048,
1.26425280914924));
#54153=CARTESIAN_POINT('Ctrl Pts',(-0.164742346274029,-0.748307446372957,
1.27609136889971));
#54154=CARTESIAN_POINT('Ctrl Pts',(0.211159022296708,-0.736556815361711,
1.28792992865019));
#54155=CARTESIAN_POINT('Ctrl Pts',(0.536189828564398,-0.547361436983983,
1.29976848840066));
#54156=CARTESIAN_POINT('Ctrl Pts',(0.732046528115873,-0.226300586889613,
1.31160704815114));
#54157=CARTESIAN_POINT('Ctrl Pts',(0.751545058775462,0.149278597204277,
1.32344560790161));
#54158=CARTESIAN_POINT('Ctrl Pts',(0.589988007153253,0.488894903193336,
1.33528416765209));
#54159=CARTESIAN_POINT('Ctrl Pts',(0.286296267893741,0.710730977194047,
1.34712272740256));
#54160=CARTESIAN_POINT('Ctrl Pts',(-0.0863674337030227,0.761344036128637,
1.35896128715304));
#54161=CARTESIAN_POINT('Ctrl Pts',(-0.438224257765704,0.628540829905892,
1.37079984690351));
#54162=CARTESIAN_POINT('Ctrl Pts',(-0.684507973159348,0.344315131288721,
1.38263840665399));
#54163=CARTESIAN_POINT('Ctrl Pts',(-0.765886087471892,-0.0228599206053984,
1.39447696640446));
#54164=CARTESIAN_POINT('Ctrl Pts',(-0.662753705827361,-0.38452776280158,
1.40631552615494));
#54165=CARTESIAN_POINT('Ctrl Pts',(-0.399956568601167,-0.653558580531132,
1.41815408590542));
#54166=CARTESIAN_POINT('Ctrl Pts',(-0.0408054356032438,-0.765139850862781,
1.42999264565589));
#54167=CARTESIAN_POINT('Ctrl Pts',(0.328176181697839,-0.692390401954935,
1.44183120540637));
#54168=CARTESIAN_POINT('Ctrl Pts',(0.618096498582505,-0.452836387002122,
1.45366976515684));
#54169=CARTESIAN_POINT('Ctrl Pts',(0.759110478913594,-0.104189038562902,
1.46550832490732));
#54170=CARTESIAN_POINT('Ctrl Pts',(0.717246282918362,0.269558610682131,
1.47734688465779));
#54171=CARTESIAN_POINT('Ctrl Pts',(0.502589462080611,0.578366585790198,
1.48918544440827));
#54172=CARTESIAN_POINT('Ctrl Pts',(0.166853237362585,0.747839603213625,
1.50102400415874));
#54173=CARTESIAN_POINT('Ctrl Pts',(-0.209079792182433,0.737149723905558,
1.51286256390922));
#54174=CARTESIAN_POINT('Ctrl Pts',(-0.534643169136526,0.548872258953521,
1.5247011236597));
#54175=CARTESIAN_POINT('Ctrl Pts',(-0.731405046871499,0.228365348430948,
1.53653968341017));
#54176=CARTESIAN_POINT('Ctrl Pts',(-0.751963295697072,-0.147157320162763,
1.54837824316065));
#54177=CARTESIAN_POINT('Ctrl Pts',(-0.591365204304262,-0.487228149937241,
1.56021680291112));
#54178=CARTESIAN_POINT('Ctrl Pts',(-0.288300643128581,-0.709920287162393,
1.5720553626616));
#54179=CARTESIAN_POINT('Ctrl Pts',(0.0842187567215935,-0.761584713586976,
1.58389392241207));
#54180=CARTESIAN_POINT('Ctrl Pts',(0.436448919274245,-0.629774892971634,
1.59573248216255));
#54181=CARTESIAN_POINT('Ctrl Pts',(0.683533671990508,-0.346245280412978,
1.60757104191302));
#54182=CARTESIAN_POINT('Ctrl Pts',(0.765947543637971,0.0206986798624194,
1.6194096016635));
#54183=CARTESIAN_POINT('Ctrl Pts',(0.663836113852885,0.382656097426644,
1.63124816141397));
#54184=CARTESIAN_POINT('Ctrl Pts',(0.401799164326967,0.652427395576886,
1.64308672116445));
#54185=CARTESIAN_POINT('Ctrl Pts',(0.042964317179197,0.765021661394247,
1.65492528091492));
#54186=CARTESIAN_POINT('Ctrl Pts',(-0.326221112908865,0.693313681132567,
1.6667638406654));
#54187=CARTESIAN_POINT('Ctrl Pts',(-0.616816240445319,0.454578706580051,
1.67860240041587));
#54188=CARTESIAN_POINT('Ctrl Pts',(-0.758813459884736,0.106330654332819,
1.69044096016635));
#54189=CARTESIAN_POINT('Ctrl Pts',(-0.718004058192813,-0.267533637832218,
1.70227951991683));
#54190=CARTESIAN_POINT('Ctrl Pts',(-0.504219475147683,-0.576946094392606,
1.7141180796673));
#54191=CARTESIAN_POINT('Ctrl Pts',(-0.168962799904339,-0.74736580548054,
1.72595663941778));
#54192=CARTESIAN_POINT('Ctrl Pts',(0.206998897298017,-0.73773676299239,
1.73779519916825));
#54193=CARTESIAN_POINT('Ctrl Pts',(0.533092252683253,-0.550378710600425,
1.74963375891873));
#54194=CARTESIAN_POINT('Ctrl Pts',(0.730757741911345,-0.230428291643451,
1.7614723186692));
#54195=CARTESIAN_POINT('Ctrl Pts',(0.752375545210572,0.145034871400566,
1.77331087841968));
#54196=CARTESIAN_POINT('Ctrl Pts',(0.592737692788189,0.485557517191581,
1.78514943817015));
#54197=CARTESIAN_POINT('Ctrl Pts',(0.29030272280774,0.709103944484463,1.79698799792063));
#54198=CARTESIAN_POINT('Ctrl Pts',(-0.0820694091594656,0.761819327028042,
1.8088265576711));
#54199=CARTESIAN_POINT('Ctrl Pts',(-0.434670105616121,0.631003941538025,
1.82066511742158));
#54200=CARTESIAN_POINT('Ctrl Pts',(-0.68255392827532,0.348172672605466,
1.83250367717205));
#54201=CARTESIAN_POINT('Ctrl Pts',(-0.76600290104831,-0.0185372743097382,
1.84434223692253));
#54202=CARTESIAN_POINT('Ctrl Pts',(-0.664913236171123,-0.380781385201656,
1.856180796673));
#54203=CARTESIAN_POINT('Ctrl Pts',(-0.403638560780521,-0.651291015759056,
1.86801935642348));
#54204=CARTESIAN_POINT('Ctrl Pts',(-0.045122856656748,-0.76489738053594,
1.87985791617396));
#54205=CARTESIAN_POINT('Ctrl Pts',(0.324263446626085,-0.694231439904046,
1.89169647592443));
#54206=CARTESIAN_POINT('Ctrl Pts',(0.615531070993343,-0.456317406611175,
1.90353503567491));
#54207=CARTESIAN_POINT('Ctrl Pts',(0.758510398898692,-0.108471423506639,
1.91537359542538));
#54208=CARTESIAN_POINT('Ctrl Pts',(0.718756116466056,0.2655065348754,1.92721215517586));
#54209=CARTESIAN_POINT('Ctrl Pts',(0.505845473412291,0.575521008951734,
1.93905071492633));
#54210=CARTESIAN_POINT('Ctrl Pts',(0.171071017145122,0.746886057315075,
1.95088927467681));
#54211=CARTESIAN_POINT('Ctrl Pts',(-0.204916354297241,0.738317927218373,
1.96272783442729));
#54212=CARTESIAN_POINT('Ctrl Pts',(-0.53153709138554,0.551880781373112,
1.97456639417776));
#54213=CARTESIAN_POINT('Ctrl Pts',(-0.73010461872186,0.232489397245945,
1.98640495392823));
#54214=CARTESIAN_POINT('Ctrl Pts',(-0.752781803375976,-0.142911262169087,
1.99824351367871));
#54215=CARTESIAN_POINT('Ctrl Pts',(-0.594105462977449,-0.483883029432169,
2.01008207342919));
#54216=CARTESIAN_POINT('Ctrl Pts',(-0.29230248841691,-0.708281933556404,
2.02192063317966));
#54217=CARTESIAN_POINT('Ctrl Pts',(0.0799194030405367,-0.76204791831005,
2.03375919293014));
#54218=CARTESIAN_POINT('Ctrl Pts',(0.432887841024017,-0.632227879318738,
2.04559775268061));
#54219=CARTESIAN_POINT('Ctrl Pts',(0.681568729895938,-0.35009746363592,
2.05743631243109));
#54220=CARTESIAN_POINT('Ctrl Pts',(0.76605219866617,0.0163760596629542,
2.06927487218156));
#54221=CARTESIAN_POINT('Ctrl Pts',(0.665984986255429,0.378902971414387,
2.08111343193203));
#54222=CARTESIAN_POINT('Ctrl Pts',(0.405474897523,0.650150774830491,2.09295199168251));
#54223=CARTESIAN_POINT('Ctrl Pts',(0.0472807317393077,0.764764388588309,
2.10479055143299));
#54224=CARTESIAN_POINT('Ctrl Pts',(-0.32230259421896,0.695148856848125,
2.11662911118346));
#54225=CARTESIAN_POINT('Ctrl Pts',(-0.614242203421617,0.458042195483833,
2.12846767093394));
#54226=CARTESIAN_POINT('Ctrl Pts',(-0.758198826500429,0.110631887344821,
2.14030623068441));
#54227=CARTESIAN_POINT('Ctrl Pts',(-0.719508397185533,-0.263520633167659,
2.15214479043489));
#54228=CARTESIAN_POINT('Ctrl Pts',(-0.578128764427879,-0.470485991417495,
2.16003716360187));
#54229=CARTESIAN_POINT('Ctrl Pts',(-0.487050803301172,-0.55099426040902,
2.16398335018536));
#54230=CARTESIAN_POINT('Ctrl Pts',(-0.333032948543728,0.687538113622998,
0.783516649814636));
#54231=CARTESIAN_POINT('Ctrl Pts',(-0.446681264116382,0.632488607446904,
0.787462836398128));
#54232=CARTESIAN_POINT('Ctrl Pts',(-0.646045483353837,0.465009286046903,
0.795355209565111));
#54233=CARTESIAN_POINT('Ctrl Pts',(-0.78947222465775,0.101533274155245,
0.807193769315587));
#54234=CARTESIAN_POINT('Ctrl Pts',(-0.742692686045743,-0.286310223461493,
0.819032329066061));
#54235=CARTESIAN_POINT('Ctrl Pts',(-0.516997271850398,-0.605223691792682,
0.830870888816538));
#54236=CARTESIAN_POINT('Ctrl Pts',(-0.166747860393462,-0.778309276622721,
0.842709448567012));
#54237=CARTESIAN_POINT('Ctrl Pts',(0.223671152539511,-0.763902968466767,
0.854548008317489));
#54238=CARTESIAN_POINT('Ctrl Pts',(0.560206210069973,-0.56545811375875,
0.866386568067964));
#54239=CARTESIAN_POINT('Ctrl Pts',(0.761780882521931,-0.230791031083385,
0.878225127818439));
#54240=CARTESIAN_POINT('Ctrl Pts',(0.779834283379,0.159477667259401,0.890063687568915));
#54241=CARTESIAN_POINT('Ctrl Pts',(0.610016793745258,0.511325667860236,
0.901902247319389));
#54242=CARTESIAN_POINT('Ctrl Pts',(0.293239518500739,0.739989994337803,
0.913740807069865));
#54243=CARTESIAN_POINT('Ctrl Pts',(-0.0941824558709746,0.790382290719356,
0.925579366820341));
#54244=CARTESIAN_POINT('Ctrl Pts',(-0.458914811425353,0.650362779594414,
0.937417926570816));
#54245=CARTESIAN_POINT('Ctrl Pts',(-0.713089481040427,0.353663576169647,
0.949256486321291));
#54246=CARTESIAN_POINT('Ctrl Pts',(-0.795472941805385,-0.0282371003573665,
0.961095046071767));
#54247=CARTESIAN_POINT('Ctrl Pts',(-0.686218105573663,-0.40333515715773,
0.972933605822241));
#54248=CARTESIAN_POINT('Ctrl Pts',(-0.411645677298192,-0.681265272215381,
0.984772165572718));
#54249=CARTESIAN_POINT('Ctrl Pts',(-0.0379032171709881,-0.795070992194145,
0.996610725323191));
#54250=CARTESIAN_POINT('Ctrl Pts',(0.344970550743188,-0.717335245721791,
1.00844928507367));
#54251=CARTESIAN_POINT('Ctrl Pts',(0.644737067398454,-0.46678544309303,
1.02028784482414));
#54252=CARTESIAN_POINT('Ctrl Pts',(0.789179237570002,-0.103781823459575,
1.03212640457462));
#54253=CARTESIAN_POINT('Ctrl Pts',(0.743499332239405,0.284223994113184,
1.04396496432509));
#54254=CARTESIAN_POINT('Ctrl Pts',(0.518702149853569,0.603757083308034,
1.05580352407557));
#54255=CARTESIAN_POINT('Ctrl Pts',(0.16894383748316,0.777838360879895,1.06764208382604));
#54256=CARTESIAN_POINT('Ctrl Pts',(-0.221514928583353,0.764529706623286,
1.07948064357652));
#54257=CARTESIAN_POINT('Ctrl Pts',(-0.558608279085167,0.567037323662244,
1.091319203327));
#54258=CARTESIAN_POINT('Ctrl Pts',(-0.761126668236282,0.232939328559625,
1.10315776307747));
#54259=CARTESIAN_POINT('Ctrl Pts',(-0.780281158578927,-0.157276347417685,
1.11499632282795));
#54260=CARTESIAN_POINT('Ctrl Pts',(-0.6114572198698,-0.509602398109476,
1.12683488257842));
#54261=CARTESIAN_POINT('Ctrl Pts',(-0.295326420858495,-0.739159550457927,
1.1386734423289));
#54262=CARTESIAN_POINT('Ctrl Pts',(0.0919518050002577,-0.790644927541561,
1.15051200207937));
#54263=CARTESIAN_POINT('Ctrl Pts',(0.457077816029287,-0.651655128103828,
1.16235056182985));
#54264=CARTESIAN_POINT('Ctrl Pts',(0.712088686039225,-0.355674344175977,
1.17418912158032));
#54265=CARTESIAN_POINT('Ctrl Pts',(0.79554945378758,0.0259923540367214,
1.1860276813308));
#54266=CARTESIAN_POINT('Ctrl Pts',(0.687353489969946,0.401397204420044,
1.19786624108127));
#54267=CARTESIAN_POINT('Ctrl Pts',(0.413566408351994,0.6801009938038,1.20970480083175));
#54268=CARTESIAN_POINT('Ctrl Pts',(0.0401465688547416,0.794960872558695,
1.22154336058222));
#54269=CARTESIAN_POINT('Ctrl Pts',(-0.342945026601437,0.718305815526664,
1.2333819203327));
#54270=CARTESIAN_POINT('Ctrl Pts',(-0.643417342272661,0.468602880435955,
1.24522048008317));
#54271=CARTESIAN_POINT('Ctrl Pts',(-0.788883247888852,0.106008287838375,
1.25705903983365));
#54272=CARTESIAN_POINT('Ctrl Pts',(-0.744298385249583,-0.282124882995013,
1.26889759958412));
#54273=CARTESIAN_POINT('Ctrl Pts',(-0.520403744761019,-0.602291024612518,
1.2807361593346));
#54274=CARTESIAN_POINT('Ctrl Pts',(-0.171138041115101,-0.777358544542589,
1.29257471908508));
#54275=CARTESIAN_POINT('Ctrl Pts',(0.219356724345348,-0.765151725721485,
1.30441327883555));
#54276=CARTESIAN_POINT('Ctrl Pts',(0.557006009697813,-0.568611326875053,
1.31625183858603));
#54277=CARTESIAN_POINT('Ctrl Pts',(0.760466338256896,-0.235086120960459,
1.3280903983365));
#54278=CARTESIAN_POINT('Ctrl Pts',(0.780721848859823,0.155073952045427,
1.33992895808698));
#54279=CARTESIAN_POINT('Ctrl Pts',(0.612892763210127,0.507874981363269,
1.35176751783745));
#54280=CARTESIAN_POINT('Ctrl Pts',(0.29741097886514,0.738323266286908,1.36360607758793));
#54281=CARTESIAN_POINT('Ctrl Pts',(-0.0897204255880114,0.7909012461252,
1.37544463733841));
#54282=CARTESIAN_POINT('Ctrl Pts',(-0.455237179385516,0.652942299437866,
1.38728319708888));
#54283=CARTESIAN_POINT('Ctrl Pts',(-0.711082222049339,0.357682274337801,
1.39912175683936));
#54284=CARTESIAN_POINT('Ctrl Pts',(-0.795619630846004,-0.0237473978059473,
1.41096031658983));
#54285=CARTESIAN_POINT('Ctrl Pts',(-0.68848340164103,-0.399456057101259,
1.42279887634031));
#54286=CARTESIAN_POINT('Ctrl Pts',(-0.415483846318822,-0.678931299424474,
1.43463743609078));
#54287=CARTESIAN_POINT('Ctrl Pts',(-0.0423896009370397,-0.794844423533616,
1.44647599584126));
#54288=CARTESIAN_POINT('Ctrl Pts',(0.340916771835822,-0.719270665724059,
1.45831455559173));
#54289=CARTESIAN_POINT('Ctrl Pts',(0.642092494006125,-0.470416586687887,
1.47015311534221));
#54290=CARTESIAN_POINT('Ctrl Pts',(0.78858097683715,-0.108233908091011,
1.48199167509268));
#54291=CARTESIAN_POINT('Ctrl Pts',(0.745091511878546,0.280023525469966,
1.49383023484316));
#54292=CARTESIAN_POINT('Ctrl Pts',(0.52210119602459,0.600820170267094,1.50566879459363));
#54293=CARTESIAN_POINT('Ctrl Pts',(0.173330882082061,0.77687253858451,1.51750735434411));
#54294=CARTESIAN_POINT('Ctrl Pts',(-0.217196773507981,0.765767652403659,
1.52934591409458));
#54295=CARTESIAN_POINT('Ctrl Pts',(-0.555399305224161,0.570180802593885,
1.54118447384506));
#54296=CARTESIAN_POINT('Ctrl Pts',(-0.75979995316492,0.237231041520021,
1.55302303359554));
#54297=CARTESIAN_POINT('Ctrl Pts',(-0.781156322746504,-0.152870321917789,
1.56486159334601));
#54298=CARTESIAN_POINT('Ctrl Pts',(-0.614323426472996,-0.506143520729609,
1.57670015309648));
#54299=CARTESIAN_POINT('Ctrl Pts',(-0.299493168776285,-0.737481103314809,
1.58853871284696));
#54300=CARTESIAN_POINT('Ctrl Pts',(0.0874883317887688,-0.791151267262402,
1.60037727259743));
#54301=CARTESIAN_POINT('Ctrl Pts',(0.453392917976011,-0.654224271805385,
1.61221583234791));
#54302=CARTESIAN_POINT('Ctrl Pts',(0.710070096161475,-0.359687356501897,
1.62405439209839));
#54303=CARTESIAN_POINT('Ctrl Pts',(0.795683472888534,0.0215022524896584,
1.63589295184886));
#54304=CARTESIAN_POINT('Ctrl Pts',(0.689607831354245,0.397511729166553,
1.64773151159934));
#54305=CARTESIAN_POINT('Ctrl Pts',(0.417397976050568,0.677756199144631,
1.65957007134981));
#54306=CARTESIAN_POINT('Ctrl Pts',(0.044632295497754,0.794721645665126,
1.67140863110029));
#54307=CARTESIAN_POINT('Ctrl Pts',(-0.338885802565579,0.720229788824076,
1.68324719085077));
#54308=CARTESIAN_POINT('Ctrl Pts',(-0.640762533163177,0.472226547310077,
1.69508575060124));
#54309=CARTESIAN_POINT('Ctrl Pts',(-0.788272426813903,0.110458666545496,
1.70692431035172));
#54310=CARTESIAN_POINT('Ctrl Pts',(-0.745878705815066,-0.2779199382947,
1.71876287010219));
#54311=CARTESIAN_POINT('Ctrl Pts',(-0.523794490126561,-0.59934453197067,
1.73060142985267));
#54312=CARTESIAN_POINT('Ctrl Pts',(-0.175522342924831,-0.776380346881776,
1.74243998960314));
#54313=CARTESIAN_POINT('Ctrl Pts',(0.215035093270084,-0.766377481762356,
1.75427854935362));
#54314=CARTESIAN_POINT('Ctrl Pts',(0.553788178457126,-0.571745738323627,
1.76611710910409));
#54315=CARTESIAN_POINT('Ctrl Pts',(0.759127518266483,-0.239374073158846,
1.77795566885457));
#54316=CARTESIAN_POINT('Ctrl Pts',(0.781584576779461,0.150665474580448,
1.78979422860504));
#54317=CARTESIAN_POINT('Ctrl Pts',(0.61574919826698,0.504408029995251,1.80163278835552));
#54318=CARTESIAN_POINT('Ctrl Pts',(0.301572974012746,0.736633068247083,
1.81347134810599));
#54319=CARTESIAN_POINT('Ctrl Pts',(-0.0852555413752697,0.791394988962569,
1.82530990785647));
#54320=CARTESIAN_POINT('Ctrl Pts',(-0.451545046485497,0.655501034998605,
1.83714846760694));
#54321=CARTESIAN_POINT('Ctrl Pts',(-0.7090523164345,0.36168957470349,1.84898702735742));
#54322=CARTESIAN_POINT('Ctrl Pts',(-0.795740979406929,-0.0192569359653573,
1.86082558710789));
#54323=CARTESIAN_POINT('Ctrl Pts',(-0.690726770156282,-0.395564236095736,
1.87266414685837));
#54324=CARTESIAN_POINT('Ctrl Pts',(-0.419308782306608,-0.676575702324082,
1.88450270660884));
#54325=CARTESIAN_POINT('Ctrl Pts',(-0.0468746346789825,-0.794592539924437,
1.89634126635932));
#54326=CARTESIAN_POINT('Ctrl Pts',(0.336852134960562,-0.721183177202469,
1.90817982610979));
#54327=CARTESIAN_POINT('Ctrl Pts',(0.639427470336365,-0.474032747865934,
1.92001838586027));
#54328=CARTESIAN_POINT('Ctrl Pts',(0.787957600270134,-0.112682545536983,
1.93185694561074));
#54329=CARTESIAN_POINT('Ctrl Pts',(0.746659960802614,0.275814138316646,
1.94369550536122));
#54330=CARTESIAN_POINT('Ctrl Pts',(0.525483613561763,0.597864121279136,
1.9555340651117));
#54331=CARTESIAN_POINT('Ctrl Pts',(0.177712406238804,0.77588197373654,1.96737262486217));
#54332=CARTESIAN_POINT('Ctrl Pts',(-0.212871700931978,0.766981208183949,
1.97921118461265));
#54333=CARTESIAN_POINT('Ctrl Pts',(-0.552172642050561,0.573306123103059,
1.99104974436312));
#54334=CARTESIAN_POINT('Ctrl Pts',(-0.758449039261035,0.241515195847213,
2.0028883041136));
#54335=CARTESIAN_POINT('Ctrl Pts',(-0.782006606865756,-0.148459421721612,
2.01472686386407));
#54336=CARTESIAN_POINT('Ctrl Pts',(-0.61717006859073,-0.502668534586218,
2.02656542361455));
#54337=CARTESIAN_POINT('Ctrl Pts',(-0.303650375341446,-0.735779144874103,
2.03840398336502));
#54338=CARTESIAN_POINT('Ctrl Pts',(0.0830220668382067,-0.79163245470895,
2.0502425431155));
#54339=CARTESIAN_POINT('Ctrl Pts',(0.449693590087432,-0.656772488993135,
2.06208110286597));
#54340=CARTESIAN_POINT('Ctrl Pts',(0.708028870280121,-0.36368909075967,
2.07391966261645));
#54341=CARTESIAN_POINT('Ctrl Pts',(0.795792190877101,0.0170118177583804,
2.08575822236693));
#54342=CARTESIAN_POINT('Ctrl Pts',(0.691840128161321,0.39361289775907,2.0975967821174));
#54343=CARTESIAN_POINT('Ctrl Pts',(0.421216410066217,0.675391194495178,
2.10943534186788));
#54344=CARTESIAN_POINT('Ctrl Pts',(0.0491162836718048,0.794454384908945,
2.12127390161835));
#54345=CARTESIAN_POINT('Ctrl Pts',(-0.334815157538176,0.722136210482901,
2.13311246136883));
#54346=CARTESIAN_POINT('Ctrl Pts',(-0.638088565819885,0.475824497198633,
2.1449510211193));
#54347=CARTESIAN_POINT('Ctrl Pts',(-0.787633931880613,0.114926883787159,
2.15678958086977));
#54348=CARTESIAN_POINT('Ctrl Pts',(-0.747441446872298,-0.273751139119435,
2.16862814062026));
#54349=CARTESIAN_POINT('Ctrl Pts',(-0.600573116106444,-0.488751391274673,
2.17652051378724));
#54350=CARTESIAN_POINT('Ctrl Pts',(-0.5059592890698,-0.572385185259003,
2.18046670037073));
#54351=CARTESIAN_POINT('Ctrl Pts',(-0.345478907940185,0.713232482552819,
0.8));
#54352=CARTESIAN_POINT('Ctrl Pts',(-0.463374437871893,0.656125690688752,
0.803946186583492));
#54353=CARTESIAN_POINT('Ctrl Pts',(-0.670189208139166,0.482387406495414,
0.811838559750475));
#54354=CARTESIAN_POINT('Ctrl Pts',(-0.818976029898903,0.105327730568796,
0.82367711950095));
#54355=CARTESIAN_POINT('Ctrl Pts',(-0.77044826715263,-0.297010081933676,
0.835515679251426));
#54356=CARTESIAN_POINT('Ctrl Pts',(-0.536318264207659,-0.627841842719682,
0.847354239001901));
#54357=CARTESIAN_POINT('Ctrl Pts',(-0.172979487351029,-0.807395905129269,
0.859192798752377));
#54358=CARTESIAN_POINT('Ctrl Pts',(0.232030091481853,-0.792451210825201,
0.871031358502853));
#54359=CARTESIAN_POINT('Ctrl Pts',(0.581141987669944,-0.586590163170117,
0.882869918253326));
#54360=CARTESIAN_POINT('Ctrl Pts',(0.790249819227213,-0.239416050963522,
0.894708478003804));
#54361=CARTESIAN_POINT('Ctrl Pts',(0.808977903760532,0.165437595789089,
0.906547037754277));
#54362=CARTESIAN_POINT('Ctrl Pts',(0.632814070348998,0.530434703552899,
0.918385597504754));
#54363=CARTESIAN_POINT('Ctrl Pts',(0.304198335508654,0.767644571650904,
0.930224157255228));
#54364=CARTESIAN_POINT('Ctrl Pts',(-0.0977022007693522,0.819920106545049,
0.942062717005705));
#54365=CARTESIAN_POINT('Ctrl Pts',(-0.476065171875897,0.674667848456801,
0.953901276756179));
#54366=CARTESIAN_POINT('Ctrl Pts',(-0.739738744321667,0.366880534216174,
0.965739836506655));
#54367=CARTESIAN_POINT('Ctrl Pts',(-0.825201003181842,-0.0292923647270269,
0.97757839625713));
#54368=CARTESIAN_POINT('Ctrl Pts',(-0.711863143749104,-0.418408419461353,
0.989416956007606));
#54369=CARTESIAN_POINT('Ctrl Pts',(-0.427029516668392,-0.70672521530295,
1.00125551575808));
#54370=CARTESIAN_POINT('Ctrl Pts',(-0.039319719363844,-0.824784032088305,
1.01309407550856));
#54371=CARTESIAN_POINT('Ctrl Pts',(0.357862636905524,-0.744143179834439,
1.02493263525903));
#54372=CARTESIAN_POINT('Ctrl Pts',(0.668831894643988,-0.484229941293575,
1.03677119500951));
#54373=CARTESIAN_POINT('Ctrl Pts',(0.818672093427876,-0.107660311658766,
1.04860975475998));
#54374=CARTESIAN_POINT('Ctrl Pts',(0.771285058969472,0.294845886949012,
1.06044831451046));
#54375=CARTESIAN_POINT('Ctrl Pts',(0.538086856154138,0.626320424794314,
1.07228687426093));
#54376=CARTESIAN_POINT('Ctrl Pts',(0.175257531520918,0.806907390532518,
1.08412543401141));
#54377=CARTESIAN_POINT('Ctrl Pts',(-0.229793286081951,0.793101371161665,
1.09596399376188));
#54378=CARTESIAN_POINT('Ctrl Pts',(-0.579484339518286,0.588228390604528,
1.10780255351236));
#54379=CARTESIAN_POINT('Ctrl Pts',(-0.789571155935928,0.241644633658621,
1.11964111326283));
#54380=CARTESIAN_POINT('Ctrl Pts',(-0.809441479381897,-0.163154009200229,
1.13147967301331));
#54381=CARTESIAN_POINT('Ctrl Pts',(-0.634308327438729,-0.528647032530609,
1.14331823276378));
#54382=CARTESIAN_POINT('Ctrl Pts',(-0.306363228654176,-0.766783092791291,
1.15515679251426));
#54383=CARTESIAN_POINT('Ctrl Pts',(0.0953881870053064,-0.820192558513891,
1.16699535226474));
#54384=CARTESIAN_POINT('Ctrl Pts',(0.474159525104011,-0.676008494040558,
1.17883391201521));
#54385=CARTESIAN_POINT('Ctrl Pts',(0.738700548054304,-0.368966447751112,
1.19067247176569));
#54386=CARTESIAN_POINT('Ctrl Pts',(0.825280374535842,0.0269637287441597,
1.20251103151616));
#54387=CARTESIAN_POINT('Ctrl Pts',(0.713040959226628,0.416398042414927,
1.21434959126664));
#54388=CARTESIAN_POINT('Ctrl Pts',(0.429022028429814,0.705517425995826,
1.22618815101711));
#54389=CARTESIAN_POINT('Ctrl Pts',(0.0416469085900688,0.82466979711076,
1.23802671076759));
#54390=CARTESIAN_POINT('Ctrl Pts',(-0.355761415775427,0.745150021342865,
1.24986527051806));
#54391=CARTESIAN_POINT('Ctrl Pts',(-0.667462849337108,0.486115299097447,
1.26170383026854));
#54392=CARTESIAN_POINT('Ctrl Pts',(-0.818365042151861,0.109969982475179,
1.27354239001902));
#54393=CARTESIAN_POINT('Ctrl Pts',(-0.772113973833753,-0.292668328782704,
1.28538094976949));
#54394=CARTESIAN_POINT('Ctrl Pts',(-0.539852042310501,-0.624799577204556,
1.29721950951997));
#54395=CARTESIAN_POINT('Ctrl Pts',(-0.177533735956174,-0.806409642712222,
1.30905806927044));
#54396=CARTESIAN_POINT('Ctrl Pts',(0.227554426393989,-0.793746636081258,
1.32089662902092));
#54397=CARTESIAN_POINT('Ctrl Pts',(0.577822190831226,-0.589861216766124,
1.33273518877139));
#54398=CARTESIAN_POINT('Ctrl Pts',(0.788886148397919,-0.243871655031303,
1.34457374852187));
#54399=CARTESIAN_POINT('Ctrl Pts',(0.809898638944184,0.160869306886576,
1.35641230827234));
#54400=CARTESIAN_POINT('Ctrl Pts',(0.635797519267003,0.526855059533203,
1.36825086802281));
#54401=CARTESIAN_POINT('Ctrl Pts',(0.308525689836539,0.765915555379768,
1.38008942777329));
#54402=CARTESIAN_POINT('Ctrl Pts',(-0.0930734174729996,0.820458456121764,
1.39192798752377));
#54403=CARTESIAN_POINT('Ctrl Pts',(-0.472250101005329,0.677343768969839,
1.40376654727424));
#54404=CARTESIAN_POINT('Ctrl Pts',(-0.737656470939329,0.371049417386882,
1.41560510702472));
#54405=CARTESIAN_POINT('Ctrl Pts',(-0.825353174220117,-0.0246348750064956,
1.42744366677519));
#54406=CARTESIAN_POINT('Ctrl Pts',(-0.714213097454698,-0.414384351400939,
1.43928222652567));
#54407=CARTESIAN_POINT('Ctrl Pts',(-0.431011124036478,-0.704304018317815,
1.45112078627615));
#54408=CARTESIAN_POINT('Ctrl Pts',(-0.0439737662708354,-0.824548996204452,
1.46295934602662));
#54409=CARTESIAN_POINT('Ctrl Pts',(0.353657361973805,-0.746150929493183,
1.4747979057771));
#54410=CARTESIAN_POINT('Ctrl Pts',(0.666088489429745,-0.487996786373651,
1.48663646552757));
#54411=CARTESIAN_POINT('Ctrl Pts',(0.818051474760706,-0.11227877761912,
1.49847502527805));
#54412=CARTESIAN_POINT('Ctrl Pts',(0.772936740838731,0.290488440257801,
1.51031358502852));
#54413=CARTESIAN_POINT('Ctrl Pts',(0.541612929968569,0.62327375474399,1.522152144779));
#54414=CARTESIAN_POINT('Ctrl Pts',(0.179808526801536,0.805905473955396,
1.53399070452947));
#54415=CARTESIAN_POINT('Ctrl Pts',(-0.225313754833528,0.794385580901761,
1.54582926427995));
#54416=CARTESIAN_POINT('Ctrl Pts',(-0.576155441311798,0.591489346234249,
1.55766782403042));
#54417=CARTESIAN_POINT('Ctrl Pts',(-0.788194859458339,0.246096734609094,
1.5695063837809));
#54418=CARTESIAN_POINT('Ctrl Pts',(-0.810349349795935,-0.158583323672815,
1.58134494353137));
#54419=CARTESIAN_POINT('Ctrl Pts',(-0.63728164864173,-0.525058891521977,
1.59318350328185));
#54420=CARTESIAN_POINT('Ctrl Pts',(-0.310685694423989,-0.765041919467224,
1.60502206303233));
#54421=CARTESIAN_POINT('Ctrl Pts',(0.0907579068559442,-0.820717820937828,
1.6168606227828));
#54422=CARTESIAN_POINT('Ctrl Pts',(0.470336916677778,-0.678673650639136,
1.62869918253328));
#54423=CARTESIAN_POINT('Ctrl Pts',(0.736606520332441,-0.373129432590817,
1.64053774228375));
#54424=CARTESIAN_POINT('Ctrl Pts',(0.825419402139098,0.022305825116897,
1.65237630203423));
#54425=CARTESIAN_POINT('Ctrl Pts',(0.715379548855604,0.412367360906464,
1.6642148617847));
#54426=CARTESIAN_POINT('Ctrl Pts',(0.432996787774168,0.703085002712376,
1.67605342153518));
#54427=CARTESIAN_POINT('Ctrl Pts',(0.0463002738163106,0.824421629936008,
1.68789198128565));
#54428=CARTESIAN_POINT('Ctrl Pts',(-0.351550492222292,0.747145896515582,
1.69973054103613));
#54429=CARTESIAN_POINT('Ctrl Pts',(-0.664708825881036,0.489874388040104,
1.7115691007866));
#54430=CARTESIAN_POINT('Ctrl Pts',(-0.817731393743069,0.114586678758172,
1.72340766053708));
#54431=CARTESIAN_POINT('Ctrl Pts',(-0.773753353437319,-0.288306238757181,
1.73524622028755));
#54432=CARTESIAN_POINT('Ctrl Pts',(-0.543369505105439,-0.621742969548736,
1.74708478003803));
#54433=CARTESIAN_POINT('Ctrl Pts',(-0.182081885945323,-0.805394888283011,
1.7589233397885));
#54434=CARTESIAN_POINT('Ctrl Pts',(0.223071289242151,-0.795018200532323,
1.77076189953898));
#54435=CARTESIAN_POINT('Ctrl Pts',(0.574484104230999,-0.593112766046828,
1.78260045928945));
#54436=CARTESIAN_POINT('Ctrl Pts',(0.787497294621621,-0.248319854674241,
1.79443901903993));
#54437=CARTESIAN_POINT('Ctrl Pts',(0.810793608348351,0.156296077760331,
1.80627757879041));
#54438=CARTESIAN_POINT('Ctrl Pts',(0.638760703745772,0.523258542798921,
1.81811613854088));
#54439=CARTESIAN_POINT('Ctrl Pts',(0.312843225217752,0.764162192009703,
1.82995469829136));
#54440=CARTESIAN_POINT('Ctrl Pts',(-0.0884416735910731,0.820970650897095,
1.84179325804183));
#54441=CARTESIAN_POINT('Ctrl Pts',(-0.468419987354874,0.679998128459186,
1.85363181779231));
#54442=CARTESIAN_POINT('Ctrl Pts',(-0.735550704593678,0.375206476801514,
1.86547037754278));
#54443=CARTESIAN_POINT('Ctrl Pts',(-0.82547905776555,-0.0199765976209763,
1.87730893729326));
#54444=CARTESIAN_POINT('Ctrl Pts',(-0.71654030414144,-0.410347086989817,
1.88914749704373));
#54445=CARTESIAN_POINT('Ctrl Pts',(-0.434979003832696,-0.701860388889109,
1.90098605679421));
#54446=CARTESIAN_POINT('Ctrl Pts',(-0.0486264127012158,-0.824287699312935,
1.91282461654468));
#54447=CARTESIAN_POINT('Ctrl Pts',(0.349440823295038,-0.748134914500893,
1.92466317629516));
#54448=CARTESIAN_POINT('Ctrl Pts',(0.66332386967939,-0.491748089120693,
1.93650173604564));
#54449=CARTESIAN_POINT('Ctrl Pts',(0.817404801641573,-0.116893667567328,
1.94834029579611));
#54450=CARTESIAN_POINT('Ctrl Pts',(0.774563805139175,0.286121741757891,
1.96017885554659));
#54451=CARTESIAN_POINT('Ctrl Pts',(0.545121753711234,0.620207233606538,
1.97201741529706));
#54452=CARTESIAN_POINT('Ctrl Pts',(0.184353795332487,0.804877890158005,
1.98385597504754));
#54453=CARTESIAN_POINT('Ctrl Pts',(-0.220827047566715,0.795644489149525,
1.99569453479801));
#54454=CARTESIAN_POINT('Ctrl Pts',(-0.572808192715582,0.594731464833006,
2.00753309454849));
#54455=CARTESIAN_POINT('Ctrl Pts',(-0.786793459800209,0.250540994448481,
2.01937165429896));
#54456=CARTESIAN_POINT('Ctrl Pts',(-0.811231410355536,-0.154007581274137,
2.03121021404944));
#54457=CARTESIAN_POINT('Ctrl Pts',(-0.64023467420401,-0.521454039740266,
2.04304877379992));
#54458=CARTESIAN_POINT('Ctrl Pts',(-0.314998262265981,-0.763276356191801,
2.05488733355038));
#54459=CARTESIAN_POINT('Ctrl Pts',(0.0861247306358769,-0.821216991107851,
2.06672589330087));
#54460=CARTESIAN_POINT('Ctrl Pts',(0.466499339150846,-0.681317098667531,
2.07856445305134));
#54461=CARTESIAN_POINT('Ctrl Pts',(0.734489010664305,-0.37728071788342,
2.09040301280181));
#54462=CARTESIAN_POINT('Ctrl Pts',(0.825532183088033,0.0176475758538063,
2.10224157255229));
#54463=CARTESIAN_POINT('Ctrl Pts',(0.717695270067213,0.408322824103754,
2.11408013230276));
#54464=CARTESIAN_POINT('Ctrl Pts',(0.436957922609435,0.700631614159863,
2.12591869205324));
#54465=CARTESIAN_POINT('Ctrl Pts',(0.0509518356043011,0.824144381229582,
2.13775725180371));
#54466=CARTESIAN_POINT('Ctrl Pts',(-0.34732772085739,0.749123564117677,
2.14959581155419));
#54467=CARTESIAN_POINT('Ctrl Pts',(-0.661934928218153,0.493606798913433,
2.16143437130467));
#54468=CARTESIAN_POINT('Ctrl Pts',(-0.817069037260797,0.119221880229497,
2.17327293105514));
#54469=CARTESIAN_POINT('Ctrl Pts',(-0.775374496559064,-0.283981645071211,
2.18511149080562));
#54470=CARTESIAN_POINT('Ctrl Pts',(-0.623017467785008,-0.507016791131852,
2.1930038639726));
#54471=CARTESIAN_POINT('Ctrl Pts',(-0.524867774838428,-0.593776110108985,
2.19695005055609));
#54472=CARTESIAN_POINT('Ctrl Pts',(-0.792449256123249,-1.33074723724148E-5,
2.02673131746348));
#54473=CARTESIAN_POINT('Ctrl Pts',(-0.792479308861568,-0.049582192157152,
2.02822428299213));
#54474=CARTESIAN_POINT('Ctrl Pts',(-0.787900256251548,-0.099145593031894,
2.02971724852078));
#54475=CARTESIAN_POINT('Ctrl Pts',(-0.778658962571061,-0.14782389506472,
2.03121021404944));
#54476=CARTESIAN_POINT('Ctrl Pts',(-0.754232498305028,-0.276489734096178,
2.03515640063293));
#54477=CARTESIAN_POINT('Ctrl Pts',(-0.697233586254521,-0.398971886918219,
2.03910258721642));
#54478=CARTESIAN_POINT('Ctrl Pts',(-0.61452806157293,-0.50051668273783,
2.04304877379991));
#54479=CARTESIAN_POINT('Ctrl Pts',(-0.531822536891337,-0.602061478557442,
2.04699496038341));
#54480=CARTESIAN_POINT('Ctrl Pts',(-0.423410399578662,-0.682668917374621,
2.0509411469669));
#54481=CARTESIAN_POINT('Ctrl Pts',(-0.302350498772013,-0.732629409269219,
2.05488733355039));
#54482=CARTESIAN_POINT('Ctrl Pts',(-0.181290597965366,-0.782589901163817,
2.05883352013388));
#54483=CARTESIAN_POINT('Ctrl Pts',(-0.0475829336647421,-0.801903446135835,
2.06277970671737));
#54484=CARTESIAN_POINT('Ctrl Pts',(0.0826666665713958,-0.78824356988179,
2.06672589330087));
#54485=CARTESIAN_POINT('Ctrl Pts',(0.212916266807534,-0.774583693627745,
2.07067207988436));
#54486=CARTESIAN_POINT('Ctrl Pts',(0.33970780297919,-0.727950396147638,
2.07461826646785));
#54487=CARTESIAN_POINT('Ctrl Pts',(0.447768516317261,-0.653961017276899,
2.07856445305134));
#54488=CARTESIAN_POINT('Ctrl Pts',(0.555829229655333,-0.57997163840616,
2.08251063963483));
#54489=CARTESIAN_POINT('Ctrl Pts',(0.645159120159819,-0.47862617814479,
2.08645682621832));
#54490=CARTESIAN_POINT('Ctrl Pts',(0.704997927482683,-0.362132065724567,
2.09040301280181));
#54491=CARTESIAN_POINT('Ctrl Pts',(0.764836734805548,-0.245637953304344,
2.09434919938531));
#54492=CARTESIAN_POINT('Ctrl Pts',(0.79518445894679,-0.113995188725269,
2.0982953859688));
#54493=CARTESIAN_POINT('Ctrl Pts',(0.792385502180608,0.01693873493926,2.10224157255229));
#54494=CARTESIAN_POINT('Ctrl Pts',(0.789586545414427,0.147872658603789,
2.10618775913578));
#54495=CARTESIAN_POINT('Ctrl Pts',(0.75364090774082,0.278097741353771,2.11013394571927));
#54496=CARTESIAN_POINT('Ctrl Pts',(0.688878530994387,0.391928414404781,
2.11408013230276));
#54497=CARTESIAN_POINT('Ctrl Pts',(0.624116154247955,0.50575908745579,2.11802631888626));
#54498=CARTESIAN_POINT('Ctrl Pts',(0.530537038428692,0.603195350807828,
2.12197250546975));
#54499=CARTESIAN_POINT('Ctrl Pts',(0.419413132684874,0.672498943662132,
2.12591869205324));
#54500=CARTESIAN_POINT('Ctrl Pts',(0.308289226941054,0.741802536516437,
2.12986487863673));
#54501=CARTESIAN_POINT('Ctrl Pts',(0.179620531272676,0.782973458873009,
2.13381106522022));
#54502=CARTESIAN_POINT('Ctrl Pts',(0.0489062573615377,0.791055450532645,
2.13775725180372));
#54503=CARTESIAN_POINT('Ctrl Pts',(-0.0586673228051905,0.797706665826054,
2.14100483453581));
#54504=CARTESIAN_POINT('Ctrl Pts',(-0.167626322520823,0.7819475667733,2.1442524172679));
#54505=CARTESIAN_POINT('Ctrl Pts',(-0.26905776807643,0.745453775914814,
2.1475));
#54506=CARTESIAN_POINT('',(-0.410244091002541,-0.575644225023336,0.8));
#54507=CARTESIAN_POINT('Ctrl Pts',(-0.410244091002539,-0.575644225023337,
0.8));
#54508=CARTESIAN_POINT('Ctrl Pts',(-0.427865382519306,-0.564603183918701,
0.8));
#54509=CARTESIAN_POINT('Ctrl Pts',(-0.444970629642914,-0.552798572830416,
0.8));
#54510=CARTESIAN_POINT('Ctrl Pts',(-0.461505849283383,-0.540259693735842,
0.8));
#54511=CARTESIAN_POINT('Ctrl Pts',(-0.485257387055636,-0.522248583698476,
0.8));
#54512=CARTESIAN_POINT('Ctrl Pts',(-0.507833747975836,-0.502723524946606,
0.8));
#54513=CARTESIAN_POINT('Ctrl Pts',(-0.529139522554897,-0.481836862385063,
0.8));
#54514=CARTESIAN_POINT('Ctrl Pts',(-0.536263390677962,-0.474853129920079,
0.8));
#54515=CARTESIAN_POINT('Ctrl Pts',(-0.543245068841058,-0.467716959459887,
0.8));
#54516=CARTESIAN_POINT('Ctrl Pts',(-0.55008052571286,-0.460433451983989,
0.8));
#54517=CARTESIAN_POINT('Ctrl Pts',(-0.556729564362481,-0.453348582074,0.8));
#54518=CARTESIAN_POINT('Ctrl Pts',(-0.563234833433516,-0.446129922658457,
0.8));
#54519=CARTESIAN_POINT('Ctrl Pts',(-0.569588353878728,-0.438788486260154,
0.8));
#54520=CARTESIAN_POINT('Ctrl Pts',(-0.592447670772818,-0.412374748784406,
0.8));
#54521=CARTESIAN_POINT('Ctrl Pts',(-0.613365866820692,-0.384353037236454,
0.8));
#54522=CARTESIAN_POINT('Ctrl Pts',(-0.632187162640585,-0.354957378738931,
0.8));
#54523=CARTESIAN_POINT('Ctrl Pts',(-0.641845472764862,-0.339872743292293,
0.8));
#54524=CARTESIAN_POINT('Ctrl Pts',(-0.650951053702501,-0.324425624633106,
0.8));
#54525=CARTESIAN_POINT('Ctrl Pts',(-0.659478734205941,-0.308644066268824,
0.8));
#54526=CARTESIAN_POINT('Ctrl Pts',(-0.663690016950242,-0.300850551444848,
0.8));
#54527=CARTESIAN_POINT('Ctrl Pts',(-0.667756705771111,-0.292981910079593,
0.8));
#54528=CARTESIAN_POINT('Ctrl Pts',(-0.671672822458712,-0.285049256379356,
0.8));
#54529=CARTESIAN_POINT('Ctrl Pts',(-0.675279999292623,-0.277742404479482,
0.8));
#54530=CARTESIAN_POINT('Ctrl Pts',(-0.678760443753924,-0.270379362225497,
0.8));
#54531=CARTESIAN_POINT('Ctrl Pts',(-0.682112403616848,-0.262963134400256,
0.8));
#54532=CARTESIAN_POINT('Ctrl Pts',(-0.696491101098182,-0.231150194892449,
0.8));
#54533=CARTESIAN_POINT('Ctrl Pts',(-0.708509103401211,-0.198361084298674,
0.8));
#54534=CARTESIAN_POINT('Ctrl Pts',(-0.71816700906694,-0.164874557004865,
0.8));
#54535=CARTESIAN_POINT('Ctrl Pts',(-0.725096186175765,-0.140849257275371,
0.8));
#54536=CARTESIAN_POINT('Ctrl Pts',(-0.730809623242255,-0.116464099854586,
0.8));
#54537=CARTESIAN_POINT('Ctrl Pts',(-0.73529274404788,-0.0918147743273888,
0.8));
#54538=CARTESIAN_POINT('Ctrl Pts',(-0.737389184126333,-0.0802880195994795,
0.8));
#54539=CARTESIAN_POINT('Ctrl Pts',(-0.739216399251251,-0.0687034374573978,
0.8));
#54540=CARTESIAN_POINT('Ctrl Pts',(-0.74077190957322,-0.0570706015003154,
0.8));
#54541=CARTESIAN_POINT('Ctrl Pts',(-0.741799324663645,-0.0493871094411838,
0.8));
#54542=CARTESIAN_POINT('Ctrl Pts',(-0.7427081925385,-0.0416825640362764,
0.8));
#54543=CARTESIAN_POINT('Ctrl Pts',(-0.743497641662436,-0.0339597144281698,
0.8));
#54544=CARTESIAN_POINT('Ctrl Pts',(-0.744231464389403,-0.0267810345265218,
0.8));
#54545=CARTESIAN_POINT('Ctrl Pts',(-0.744861106235136,-0.0195961998053866,
0.8));
#54546=CARTESIAN_POINT('Ctrl Pts',(-0.745386565611995,-0.0124084559110833,
0.8));
#54547=CARTESIAN_POINT('Ctrl Pts',(-0.748026655936726,0.0237052646687871,
0.8));
#54548=CARTESIAN_POINT('Ctrl Pts',(-0.74804166046495,0.0598982256610108,
0.8));
#54549=CARTESIAN_POINT('Ctrl Pts',(-0.74541198023048,0.0958822642309481,
0.8));
#54550=CARTESIAN_POINT('Ctrl Pts',(-0.743118296207274,0.127268595267087,
0.8));
#54551=CARTESIAN_POINT('Ctrl Pts',(-0.738811956202042,0.158496935357709,
0.8));
#54552=CARTESIAN_POINT('Ctrl Pts',(-0.732567679777806,0.189394981218774,
0.8));
#54553=CARTESIAN_POINT('Ctrl Pts',(-0.728871602747368,0.207683978987875,
0.8));
#54554=CARTESIAN_POINT('Ctrl Pts',(-0.724495919547074,0.225857276064614,
0.8));
#54555=CARTESIAN_POINT('Ctrl Pts',(-0.719450927062176,0.243878325627313,
0.8));
#54556=CARTESIAN_POINT('Ctrl Pts',(-0.716942162599312,0.25283979957633,
0.8));
#54557=CARTESIAN_POINT('Ctrl Pts',(-0.7142667112202,0.261766480726714,0.8));
#54558=CARTESIAN_POINT('Ctrl Pts',(-0.711433641154155,0.270630156805554,
0.8));
#54559=CARTESIAN_POINT('Ctrl Pts',(-0.700362437871719,0.305268043412969,
0.8));
#54560=CARTESIAN_POINT('Ctrl Pts',(-0.686869620567715,0.339017637772264,
0.8));
#54561=CARTESIAN_POINT('Ctrl Pts',(-0.671084494453807,0.371624233448503,
0.8));
#54562=CARTESIAN_POINT('Ctrl Pts',(-0.657862557602499,0.398936169118597,
0.8));
#54563=CARTESIAN_POINT('Ctrl Pts',(-0.643031245141321,0.425446637465682,
0.8));
#54564=CARTESIAN_POINT('Ctrl Pts',(-0.626639134868092,0.450999679702338,
0.8));
#54565=CARTESIAN_POINT('Ctrl Pts',(-0.617718019074226,0.464906470522983,
0.8));
#54566=CARTESIAN_POINT('Ctrl Pts',(-0.608334186215446,0.478529525381889,
0.8));
#54567=CARTESIAN_POINT('Ctrl Pts',(-0.598506201793284,0.491852341465841,
0.8));
#54568=CARTESIAN_POINT('Ctrl Pts',(-0.59296152296404,0.49936870831315,0.8));
#54569=CARTESIAN_POINT('Ctrl Pts',(-0.58727544055949,0.506789488860121,
0.8));
#54570=CARTESIAN_POINT('Ctrl Pts',(-0.581451041194421,0.514111518781399,
0.8));
#54571=CARTESIAN_POINT('Ctrl Pts',(-0.576846734062576,0.519899733577986,
0.8));
#54572=CARTESIAN_POINT('Ctrl Pts',(-0.572157004628658,0.525624771374302,
0.8));
#54573=CARTESIAN_POINT('Ctrl Pts',(-0.56739138065304,0.531276185837925,
0.8));
#54574=CARTESIAN_POINT('Ctrl Pts',(-0.543777984951897,0.55927862301791,
0.8));
#54575=CARTESIAN_POINT('Ctrl Pts',(-0.518255565866718,0.585538394849063,
0.8));
#54576=CARTESIAN_POINT('Ctrl Pts',(-0.491061458562882,0.609904318648996,
0.8));
#54577=CARTESIAN_POINT('Ctrl Pts',(-0.463733518954985,0.634390156211358,
0.8));
#54578=CARTESIAN_POINT('Ctrl Pts',(-0.434716576426148,0.656964357819938,
0.8));
#54579=CARTESIAN_POINT('Ctrl Pts',(-0.404209754469363,0.677442878107525,
0.8));
#54580=CARTESIAN_POINT('Ctrl Pts',(-0.385198137815666,0.690204934341835,
0.8));
#54581=CARTESIAN_POINT('Ctrl Pts',(-0.365607118174303,0.702152441062861,
0.8));
#54582=CARTESIAN_POINT('Ctrl Pts',(-0.345478907940185,0.713232482552819,
0.8));
#54583=CARTESIAN_POINT('Ctrl Pts',(-0.410244091002541,-0.575644225023336,
0.8));
#54584=CARTESIAN_POINT('Ctrl Pts',(-0.331890193452863,-0.631365139834126,
0.803247582732095));
#54585=CARTESIAN_POINT('Ctrl Pts',(-0.132967640534065,-0.719349431943114,
0.810441352047681));
#54586=CARTESIAN_POINT('Ctrl Pts',(0.206953274654826,-0.706806483749897,
0.821581307946761));
#54587=CARTESIAN_POINT('Ctrl Pts',(0.518334654870034,-0.523194014936019,
0.833419867697235));
#54588=CARTESIAN_POINT('Ctrl Pts',(0.704843009111363,-0.213540991323109,
0.845258427447713));
#54589=CARTESIAN_POINT('Ctrl Pts',(0.72154704261594,0.147557810200025,0.857096987198186));
#54590=CARTESIAN_POINT('Ctrl Pts',(0.564422240537776,0.473107596474913,
0.868935546948663));
#54591=CARTESIAN_POINT('Ctrl Pts',(0.271321884484909,0.684680839711599,
0.880774106699136));
#54592=CARTESIAN_POINT('Ctrl Pts',(-0.0871429660742197,0.731306659067973,
0.892612666449614));
#54593=CARTESIAN_POINT('Ctrl Pts',(-0.424614090524265,0.601752641869639,
0.904451226200088));
#54594=CARTESIAN_POINT('Ctrl Pts',(-0.654181788655658,0.333777263871536,
0.91600742635268));
#54595=CARTESIAN_POINT('Ctrl Pts',(-0.706836463769599,0.10844725711356,
0.92361743992178));
#54596=CARTESIAN_POINT('Ctrl Pts',(-0.70690109581483,-8.28105672094105E-6,
0.927281266907388));
#54597=CARTESIAN_POINT('Origin',(0.,0.,0.522718733092613));
#54598=CARTESIAN_POINT('',(0.410219162127156,-0.575636310115765,0.8));
#54599=CARTESIAN_POINT('Origin',(0.,0.,0.8));
#54600=CARTESIAN_POINT('Ctrl Pts',(0.410219162127157,-0.575636310115765,
0.8));
#54601=CARTESIAN_POINT('Ctrl Pts',(0.50537039190027,-0.507828117569598,
0.803946186583492));
#54602=CARTESIAN_POINT('Ctrl Pts',(0.661310874189135,-0.324192005087297,
0.811838559750475));
#54603=CARTESIAN_POINT('Ctrl Pts',(0.735886669498874,0.0295778738072663,
0.82367711950095));
#54604=CARTESIAN_POINT('Ctrl Pts',(0.633181296569113,0.376134898320248,
0.835515679251426));
#54605=CARTESIAN_POINT('Ctrl Pts',(0.377934853131171,0.632119386061258,
0.847354239001902));
#54606=CARTESIAN_POINT('Ctrl Pts',(0.0316399747779213,0.735797878194255,
0.859192798752376));
#54607=CARTESIAN_POINT('Ctrl Pts',(-0.322277466664887,0.662225266491492,
0.871031358502852));
#54608=CARTESIAN_POINT('Ctrl Pts',(-0.598554603122584,0.429109740989168,
0.882869918253328));
#54609=CARTESIAN_POINT('Ctrl Pts',(-0.697801857104019,0.176262631310262,
0.891765709783247));
#54610=CARTESIAN_POINT('Ctrl Pts',(-0.70687082927169,0.0297279928167443,
0.896715314729675));
#54611=CARTESIAN_POINT('Ctrl Pts',(-0.706841592163942,1.7867609379222E-5,
0.897718733092612));
#54612=CARTESIAN_POINT('Ctrl Pts',(0.459925989935304,-0.645386964372562,
0.750549949443908));
#54613=CARTESIAN_POINT('Ctrl Pts',(0.56660682688118,-0.569362358596461,
0.7544961360274));
#54614=CARTESIAN_POINT('Ctrl Pts',(0.741442834823356,-0.363474802336684,
0.762388509194383));
#54615=CARTESIAN_POINT('Ctrl Pts',(0.825055083225377,0.0331618660143685,
0.77422706894486));
#54616=CARTESIAN_POINT('Ctrl Pts',(0.709904757064473,0.421711688362163,
0.786065628695334));
#54617=CARTESIAN_POINT('Ctrl Pts',(0.423729746207052,0.708714173379848,
0.79790418844581));
#54618=CARTESIAN_POINT('Ctrl Pts',(0.0354738346346534,0.824955532954583,
0.809742748196284));
#54619=CARTESIAN_POINT('Ctrl Pts',(-0.361328276624348,0.742468025315849,
0.821581307946761));
#54620=CARTESIAN_POINT('Ctrl Pts',(-0.671082298896012,0.481105566575535,
0.833419867697235));
#54621=CARTESIAN_POINT('Ctrl Pts',(-0.819165154783747,0.103842512917493,
0.845258427447712));
#54622=CARTESIAN_POINT('Ctrl Pts',(-0.769901973202423,-0.298438927106654,
0.857096987198186));
#54623=CARTESIAN_POINT('Ctrl Pts',(-0.535160834284934,-0.628822310037111,
0.868935546948663));
#54624=CARTESIAN_POINT('Ctrl Pts',(-0.171493479654568,-0.807715789857204,
0.880774106699136));
#54625=CARTESIAN_POINT('Ctrl Pts',(0.233488563272111,-0.792021329318452,
0.892612666449614));
#54626=CARTESIAN_POINT('Ctrl Pts',(0.582220609890365,-0.585520204307218,
0.904451226200087));
#54627=CARTESIAN_POINT('Ctrl Pts',(0.790689220785267,-0.237960683284075,
0.916289785950564));
#54628=CARTESIAN_POINT('Ctrl Pts',(0.808671984762012,0.166926192695345,
0.928128345701038));
#54629=CARTESIAN_POINT('Ctrl Pts',(0.631836653009791,0.531598701367769,
0.939966905451514));
#54630=CARTESIAN_POINT('Ctrl Pts',(0.302784828425095,0.7682031503306,0.951805465201989));
#54631=CARTESIAN_POINT('Ctrl Pts',(-0.0992112365740696,0.819738900460409,
0.963644024952465));
#54632=CARTESIAN_POINT('Ctrl Pts',(-0.47730620873286,0.673790409958764,
0.97548258470294));
#54633=CARTESIAN_POINT('Ctrl Pts',(-0.740412794591558,0.365518299690486,
0.987321144453415));
#54634=CARTESIAN_POINT('Ctrl Pts',(-0.825145684698249,-0.0308112439180193,
0.999159704203891));
#54635=CARTESIAN_POINT('Ctrl Pts',(-0.71109178130035,-0.419718015185374,
1.01099826395437));
#54636=CARTESIAN_POINT('Ctrl Pts',(-0.425727941103712,-0.70751003802647,
1.02283682370484));
#54637=CARTESIAN_POINT('Ctrl Pts',(-0.0378014942215861,-0.824855005894519,
1.03467538345532));
#54638=CARTESIAN_POINT('Ctrl Pts',(0.359231753999693,-0.74348320804793,
1.04651394320579));
#54639=CARTESIAN_POINT('Ctrl Pts',(0.66972206825419,-0.482998017612323,
1.05835250295627));
#54640=CARTESIAN_POINT('Ctrl Pts',(0.818868870740767,-0.106153220665947,
1.07019106270674));
#54641=CARTESIAN_POINT('Ctrl Pts',(0.770741034171086,0.296265070453716,
1.08202962245722));
#54642=CARTESIAN_POINT('Ctrl Pts',(0.536933090865458,0.627309803573318,
1.09386818220769));
#54643=CARTESIAN_POINT('Ctrl Pts',(0.173771980669987,0.807228612265459,
1.10570674195817));
#54644=CARTESIAN_POINT('Ctrl Pts',(-0.231252736739835,0.792677049923898,
1.11754530170865));
#54645=CARTESIAN_POINT('Ctrl Pts',(-0.580566092048616,0.587160750126607,
1.12938386145912));
#54646=CARTESIAN_POINT('Ctrl Pts',(-0.790014604096767,0.240190880425609,
1.14122242120959));
#54647=CARTESIAN_POINT('Ctrl Pts',(-0.809139791567519,-0.164643649825546,
1.15306098096007));
#54648=CARTESIAN_POINT('Ctrl Pts',(-0.633334183606886,-0.529813689518128,
1.16489954071054));
#54649=CARTESIAN_POINT('Ctrl Pts',(-0.304951310912786,-0.767345705466825,
1.17673810046102));
#54650=CARTESIAN_POINT('Ctrl Pts',(0.0968977319333379,-0.820015587212819,
1.1885766602115));
#54651=CARTESIAN_POINT('Ctrl Pts',(0.475403031018361,-0.675134573121806,
1.20041521996197));
#54652=CARTESIAN_POINT('Ctrl Pts',(0.739378440518577,-0.3676061145059,1.21225377971245));
#54653=CARTESIAN_POINT('Ctrl Pts',(0.825229341698803,0.0284827548732166,
1.22409233946292));
#54654=CARTESIAN_POINT('Ctrl Pts',(0.712273295467589,0.41770981110042,1.2359308992134));
#54655=CARTESIAN_POINT('Ctrl Pts',(0.427722672505628,0.706305917538889,
1.24776945896387));
#54656=CARTESIAN_POINT('Ctrl Pts',(0.0401288898270517,0.824745055109187,
1.25960801871435));
#54657=CARTESIAN_POINT('Ctrl Pts',(-0.357132389735606,0.744493915305923,
1.27144657846482));
#54658=CARTESIAN_POINT('Ctrl Pts',(-0.668356495584918,0.484885892283179,
1.2832851382153));
#54659=CARTESIAN_POINT('Ctrl Pts',(-0.818566071344556,0.108463452689587,
1.29512369796577));
#54660=CARTESIAN_POINT('Ctrl Pts',(-0.771573955797898,-0.294089041720683,
1.30696225771625));
#54661=CARTESIAN_POINT('Ctrl Pts',(-0.538701073410628,-0.625792207711191,
1.31880081746672));
#54662=CARTESIAN_POINT('Ctrl Pts',(-0.176049097430337,-0.806735055033417,
1.3306393772172));
#54663=CARTESIAN_POINT('Ctrl Pts',(0.229015068575353,-0.793326434761401,
1.34247793696768));
#54664=CARTESIAN_POINT('Ctrl Pts',(0.578906951684556,-0.588796632987233,
1.35431649671815));
#54665=CARTESIAN_POINT('Ctrl Pts',(0.7893336969416,-0.242419158892843,1.36615505646863));
#54666=CARTESIAN_POINT('Ctrl Pts',(0.809601155745132,0.162359792873586,
1.3779936162191));
#54667=CARTESIAN_POINT('Ctrl Pts',(0.634826671343973,0.528024460679748,
1.38983217596958));
#54668=CARTESIAN_POINT('Ctrl Pts',(0.307115365276427,0.766482149914096,
1.40167073572005));
#54669=CARTESIAN_POINT('Ctrl Pts',(-0.0945834557624904,0.820285745104614,
1.41350929547053));
#54670=CARTESIAN_POINT('Ctrl Pts',(-0.473496067967565,0.676473360410492,
1.425347855221));
#54671=CARTESIAN_POINT('Ctrl Pts',(-0.738338199244068,0.369691002409899,
1.43718641497148));
#54672=CARTESIAN_POINT('Ctrl Pts',(-0.825306427919384,-0.0261540390906397,
1.44902497472195));
#54673=CARTESIAN_POINT('Ctrl Pts',(-0.713449138253425,-0.415698281029946,
1.46086353447243));
#54674=CARTESIAN_POINT('Ctrl Pts',(-0.429713998222261,-0.705096173197421,
1.4727020942229));
#54675=CARTESIAN_POINT('Ctrl Pts',(-0.0424559659116393,-0.824628537393848,
1.48454065397338));
#54676=CARTESIAN_POINT('Ctrl Pts',(0.355030181852222,-0.745498694633187,
1.49637921372386));
#54677=CARTESIAN_POINT('Ctrl Pts',(0.666985601215579,-0.486769906112632,
1.50821777347433));
#54678=CARTESIAN_POINT('Ctrl Pts',(0.818256754224468,-0.110772821088234,
1.52005633322481));
#54679=CARTESIAN_POINT('Ctrl Pts',(0.772400733869309,0.291910671343068,
1.53189489297528));
#54680=CARTESIAN_POINT('Ctrl Pts',(0.540464766619871,0.624269629061302,
1.54373345272576));
#54681=CARTESIAN_POINT('Ctrl Pts',(0.178324812423069,0.806235074280501,
1.55557201247623));
#54682=CARTESIAN_POINT('Ctrl Pts',(-0.22677557690873,0.793969502842219,
1.56741057222671));
#54683=CARTESIAN_POINT('Ctrl Pts',(-0.577243201850593,0.590427827632711,
1.57924913197718));
#54684=CARTESIAN_POINT('Ctrl Pts',(-0.788646504821451,0.244645507129634,
1.59108769172766));
#54685=CARTESIAN_POINT('Ctrl Pts',(-0.810056073580812,-0.160074643153275,
1.60292625147813));
#54686=CARTESIAN_POINT('Ctrl Pts',(-0.636314104357801,-0.526231027516561,
1.61476481122861));
#54687=CARTESIAN_POINT('Ctrl Pts',(-0.309276974274663,-0.765612491348801,
1.62660337097908));
#54688=CARTESIAN_POINT('Ctrl Pts',(0.0922684264834133,-0.820549371579847,
1.63844193072956));
#54689=CARTESIAN_POINT('Ctrl Pts',(0.471585334767065,-0.677806761369672,
1.65028049048004));
#54690=CARTESIAN_POINT('Ctrl Pts',(0.737292079049471,-0.371772946698273,
1.66211905023051));
#54691=CARTESIAN_POINT('Ctrl Pts',(0.82537694274688,0.0238251150599866,
1.67395760998099));
#54692=CARTESIAN_POINT('Ctrl Pts',(0.714619300295028,0.413683441016981,
1.68579616973146));
#54693=CARTESIAN_POINT('Ctrl Pts',(0.431701902398121,0.703880814621091,
1.69763472948194));
#54694=CARTESIAN_POINT('Ctrl Pts',(0.0447827039462235,0.824505453683039,
1.70947328923241));
#54695=CARTESIAN_POINT('Ctrl Pts',(-0.352925147088058,0.746497538025865,
1.72131184898289));
#54696=CARTESIAN_POINT('Ctrl Pts',(-0.665609396061764,0.4886500441012,1.73315040873336));
#54697=CARTESIAN_POINT('Ctrl Pts',(-0.817940921843388,0.113081307472958,
1.74498896848384));
#54698=CARTESIAN_POINT('Ctrl Pts',(-0.773221361802213,-0.289729976665395,
1.75682752823431));
#54699=CARTESIAN_POINT('Ctrl Pts',(-0.542224156450018,-0.622742079747232,
1.76866608798479));
#54700=CARTESIAN_POINT('Ctrl Pts',(-0.180599107528113,-0.805728673987568,
1.78050464773526));
#54701=CARTESIAN_POINT('Ctrl Pts',(0.224534279571627,-0.794606249046181,
1.79234320748574));
#54702=CARTESIAN_POINT('Ctrl Pts',(0.575574855794106,-0.592054321074615,
1.80418176723621));
#54703=CARTESIAN_POINT('Ctrl Pts',(0.787953033208021,-0.246869907409427,
1.81602032698669));
#54704=CARTESIAN_POINT('Ctrl Pts',(0.810504541452285,0.157788218860708,
1.82785888673717));
#54705=CARTESIAN_POINT('Ctrl Pts',(0.637796470804967,0.524433404306811,
1.83969744648764));
#54706=CARTESIAN_POINT('Ctrl Pts',(0.311436120695792,0.764736736698907,
1.85153600623812));
#54707=CARTESIAN_POINT('Ctrl Pts',(-0.0899526625288732,0.820806464532657,
1.86337456598859));
#54708=CARTESIAN_POINT('Ctrl Pts',(-0.469670846631493,0.679134765395703,
1.87521312573907));
#54709=CARTESIAN_POINT('Ctrl Pts',(-0.736240088263044,0.373851930767355,
1.88705168548954));
#54710=CARTESIAN_POINT('Ctrl Pts',(-0.825440885622466,-0.0214960012726903,
1.89889024524002));
#54711=CARTESIAN_POINT('Ctrl Pts',(-0.715783772269915,-0.411665307207877,
1.91072880499049));
#54712=CARTESIAN_POINT('Ctrl Pts',(-0.433686369215096,-0.702659851282511,
1.92256736474097));
#54713=CARTESIAN_POINT('Ctrl Pts',(-0.0471090853840522,-0.824375805361169,
1.93440592449144));
#54714=CARTESIAN_POINT('Ctrl Pts',(0.350817302163829,-0.747490436731311,
1.94624448424192));
#54715=CARTESIAN_POINT('Ctrl Pts',(0.664227891161086,-0.490526292859221,
1.95808304399239));
#54716=CARTESIAN_POINT('Ctrl Pts',(0.817618576558387,-0.115388890337554,
1.96992160374287));
#54717=CARTESIAN_POINT('Ctrl Pts',(0.774035833374271,0.287546968872276,
1.98176016349334));
#54718=CARTESIAN_POINT('Ctrl Pts',(0.543979228275698,0.621209584148259,
1.99359872324382));
#54719=CARTESIAN_POINT('Ctrl Pts',(0.182871965855505,0.805215834033574,
2.00543728299429));
#54720=CARTESIAN_POINT('Ctrl Pts',(-0.222291196819829,0.795236716056979,
2.01727584274477));
#54721=CARTESIAN_POINT('Ctrl Pts',(-0.573901922034738,0.593676005947508,
2.02911440249525));
#54722=CARTESIAN_POINT('Ctrl Pts',(-0.787253297042653,0.249092528689698,
2.04095296224572));
#54723=CARTESIAN_POINT('Ctrl Pts',(-0.810946537164922,-0.155500907267836,
2.0527915219962));
#54724=CARTESIAN_POINT('Ctrl Pts',(-0.63927379570346,-0.522630875674616,
2.06463008174667));
#54725=CARTESIAN_POINT('Ctrl Pts',(-0.313592714551083,-0.763856335632048,
2.07646864149715));
#54726=CARTESIAN_POINT('Ctrl Pts',(0.0876360384442657,-0.821054169383398,
2.08830720124762));
#54727=CARTESIAN_POINT('Ctrl Pts',(0.467752902891962,-0.680463003554431,
2.1001457609981));
#54728=CARTESIAN_POINT('Ctrl Pts',(0.735181678416232,-0.375916761963503,
2.11198432074857));
#54729=CARTESIAN_POINT('Ctrl Pts',(0.825499299349533,0.0191443591436184,
2.12382288049905));
#54730=CARTESIAN_POINT('Ctrl Pts',(0.716941133028235,0.409691128799217,
2.13566144024952));
#54731=CARTESIAN_POINT('Ctrl Pts',(0.529419834375704,0.604095547595317,
2.14355381341651));
#54732=CARTESIAN_POINT('Ctrl Pts',(0.418139433688274,0.673212941048261,
2.1475));
#54733=CARTESIAN_POINT('Ctrl Pts',(0.443357047332588,-0.622136746286963,
0.767033299629272));
#54734=CARTESIAN_POINT('Ctrl Pts',(0.546194681887543,-0.54885094492084,
0.770979486212764));
#54735=CARTESIAN_POINT('Ctrl Pts',(0.714732181278616,-0.350380536586888,
0.778871859379748));
#54736=CARTESIAN_POINT('Ctrl Pts',(0.795332278649875,0.0319672019453344,
0.790710419130223));
#54737=CARTESIAN_POINT('Ctrl Pts',(0.684330270232686,0.406519425014858,
0.802548978880699));
#54738=CARTESIAN_POINT('Ctrl Pts',(0.408464781848425,0.683182577606985,
0.814387538631174));
#54739=CARTESIAN_POINT('Ctrl Pts',(0.0341958813490759,0.795236314701139,
0.826226098381649));
#54740=CARTESIAN_POINT('Ctrl Pts',(-0.348311339971194,0.715720439041064,
0.838064658132124));
#54741=CARTESIAN_POINT('Ctrl Pts',(-0.64690640030487,0.463773624713412,
0.849903217882599));
#54742=CARTESIAN_POINT('Ctrl Pts',(-0.789654536273872,0.100101561821222,
0.861741777633075));
#54743=CARTESIAN_POINT('Ctrl Pts',(-0.742166072464343,-0.287687594149059,
0.873580337383551));
#54744=CARTESIAN_POINT('Ctrl Pts',(-0.515881538614479,-0.60616883754303,
0.885418897134026));
#54745=CARTESIAN_POINT('Ctrl Pts',(-0.165315386475844,-0.778617637427649,
0.8972574568845));
#54746=CARTESIAN_POINT('Ctrl Pts',(0.225077082538461,-0.763488573543004,
0.909096016634978));
#54747=CARTESIAN_POINT('Ctrl Pts',(0.561245974669709,-0.564426700417032,
0.920934576385451));
#54748=CARTESIAN_POINT('Ctrl Pts',(0.762204454534896,-0.229388093368919,
0.932773136135928));
#54749=CARTESIAN_POINT('Ctrl Pts',(0.779539385184779,0.160912637109918,
0.944611695886402));
#54750=CARTESIAN_POINT('Ctrl Pts',(0.609074588096946,0.512447732378433,
0.956450255636878));
#54751=CARTESIAN_POINT('Ctrl Pts',(0.291876933344291,0.740528450088406,
0.968288815387353));
#54752=CARTESIAN_POINT('Ctrl Pts',(-0.0956371283037994,0.790207612626788,
0.980127375137829));
#54753=CARTESIAN_POINT('Ctrl Pts',(-0.460111139635923,0.649516951025863,
0.991965934888304));
#54754=CARTESIAN_POINT('Ctrl Pts',(-0.713739248489869,0.352350416465043,
1.00380449463878));
#54755=CARTESIAN_POINT('Ctrl Pts',(-0.795419616183252,-0.0297012615661471,
1.01564305438926));
#54756=CARTESIAN_POINT('Ctrl Pts',(-0.685474531639624,-0.404597574385953,
1.02748161413973));
#54757=CARTESIAN_POINT('Ctrl Pts',(-0.410390991301174,-0.682021821514602,
1.03932017389021));
#54758=CARTESIAN_POINT('Ctrl Pts',(-0.0364396864486812,-0.795139409152199,
1.05115873364068));
#54759=CARTESIAN_POINT('Ctrl Pts',(0.346290345070115,-0.716699049575036,
1.06299729339116));
#54760=CARTESIAN_POINT('Ctrl Pts',(0.645595172293739,-0.465597899753859,
1.07483585314163));
#54761=CARTESIAN_POINT('Ctrl Pts',(0.789368925933639,-0.10232902577634,
1.08667441289211));
#54762=CARTESIAN_POINT('Ctrl Pts',(0.742974906063093,0.285592051196362,
1.09851297264258));
#54763=CARTESIAN_POINT('Ctrl Pts',(0.517589949232386,0.604710819482443,
1.11035153239306));
#54764=CARTESIAN_POINT('Ctrl Pts',(0.167511803953105,0.778148010523909,
1.12219009214353));
#54765=CARTESIAN_POINT('Ctrl Pts',(-0.222921802185991,0.7641206716585,1.13402865189401));
#54766=CARTESIAN_POINT('Ctrl Pts',(-0.559651061224657,0.566008145185137,
1.14586721164448));
#54767=CARTESIAN_POINT('Ctrl Pts',(-0.761554141072209,0.23153794713078,
1.15770577139496));
#54768=CARTESIAN_POINT('Ctrl Pts',(-0.779990339139439,-0.158712323387036,
1.16954433114543));
#54769=CARTESIAN_POINT('Ctrl Pts',(-0.610518169799975,-0.510727026002996,
1.18138289089591));
#54770=CARTESIAN_POINT('Ctrl Pts',(-0.293965367787789,-0.739701894878714,
1.19322145064639));
#54771=CARTESIAN_POINT('Ctrl Pts',(0.0934069682151096,-0.79047433167348,
1.20506001039686));
#54772=CARTESIAN_POINT('Ctrl Pts',(0.458276524348867,-0.650812690392937,
1.21689857014734));
#54773=CARTESIAN_POINT('Ctrl Pts',(0.712742157267088,-0.354363017257769,
1.22873712989781));
#54774=CARTESIAN_POINT('Ctrl Pts',(0.795500259420569,0.0274566568900879,
1.24057568964829));
#54775=CARTESIAN_POINT('Ctrl Pts',(0.68661348147945,0.402661716328286,1.25241424939876));
#54776=CARTESIAN_POINT('Ctrl Pts',(0.412313862032396,0.680861079752473,
1.26425280914924));
#54777=CARTESIAN_POINT('Ctrl Pts',(0.0386832370768144,0.795033419369922,
1.27609136889971));
#54778=CARTESIAN_POINT('Ctrl Pts',(-0.344266610900337,0.717673345864933,
1.28792992865019));
#54779=CARTESIAN_POINT('Ctrl Pts',(-0.644278794702964,0.46741776329304,
1.29976848840066));
#54780=CARTESIAN_POINT('Ctrl Pts',(-0.789077034957317,0.104556031144744,
1.31160704815114));
#54781=CARTESIAN_POINT('Ctrl Pts',(-0.743777821491236,-0.28349441441327,
1.32344560790161));
#54782=CARTESIAN_POINT('Ctrl Pts',(-0.519294239788073,-0.603247895370303,
1.33528416765209));
#54783=CARTESIAN_POINT('Ctrl Pts',(-0.169706887043414,-0.777672233807923,
1.34712272740256));
#54784=CARTESIAN_POINT('Ctrl Pts',(0.220764746546551,-0.764746662253593,
1.35896128715304));
#54785=CARTESIAN_POINT('Ctrl Pts',(0.558051691784754,-0.56758509497867,
1.37079984690351));
#54786=CARTESIAN_POINT('Ctrl Pts',(0.760897763758405,-0.233685951339037,
1.38263840665399));
#54787=CARTESIAN_POINT('Ctrl Pts',(0.780435082563398,0.156510742922116,
1.39447696640446));
#54788=CARTESIAN_POINT('Ctrl Pts',(0.611956890313221,0.509002254556838,
1.40631552615494));
#54789=CARTESIAN_POINT('Ctrl Pts',(0.296051461580979,0.738869449119083,
1.41815408590542));
#54790=CARTESIAN_POINT('Ctrl Pts',(-0.0911760643908585,0.790734757063307,
1.42999264565589));
#54791=CARTESIAN_POINT('Ctrl Pts',(-0.45643826009315,0.652103247552801,
1.44183120540637));
#54792=CARTESIAN_POINT('Ctrl Pts',(-0.711739390930608,0.356372796581756,
1.45366976515684));
#54793=CARTESIAN_POINT('Ctrl Pts',(-0.795574568591815,-0.0252118336445362,
1.46550832490732));
#54794=CARTESIAN_POINT('Ctrl Pts',(-0.687746964250731,-0.400722652104515,
1.47734688465779));
#54795=CARTESIAN_POINT('Ctrl Pts',(-0.414233449768953,-0.679694916737122,
1.48918544440827));
#54796=CARTESIAN_POINT('Ctrl Pts',(-0.0409264796948852,-0.794921099232845,
1.50102400415875));
#54797=CARTESIAN_POINT('Ctrl Pts',(0.34224013555332,-0.718641927779209,
1.51286256390922));
#54798=CARTESIAN_POINT('Ctrl Pts',(0.642957287127624,-0.469233905078542,
1.5247011236597));
#54799=CARTESIAN_POINT('Ctrl Pts',(0.788778861059663,-0.106782204000449,
1.53653968341017));
#54800=CARTESIAN_POINT('Ctrl Pts',(0.744574814687013,0.281394520343896,
1.54837824316065));
#54801=CARTESIAN_POINT('Ctrl Pts',(0.520994395532177,0.601780167976507,
1.56021680291112));
#54802=CARTESIAN_POINT('Ctrl Pts',(0.171900618865114,0.777190264979923,
1.5720553626616));
#54803=CARTESIAN_POINT('Ctrl Pts',(-0.218605933097067,0.765366563654654,
1.58389392241207));
#54804=CARTESIAN_POINT('Ctrl Pts',(-0.556447878932191,0.569157525451115,
1.59573248216255));
#54805=CARTESIAN_POINT('Ctrl Pts',(-0.760235327896969,0.235832094853859,
1.60757104191302));
#54806=CARTESIAN_POINT('Ctrl Pts',(-0.780873611876416,-0.15430791626113,
1.6194096016635));
#54807=CARTESIAN_POINT('Ctrl Pts',(-0.613390738200811,-0.507273430247668,
1.63124816141397));
#54808=CARTESIAN_POINT('Ctrl Pts',(-0.29813519810363,-0.73803112020936,
1.64308672116445));
#54809=CARTESIAN_POINT('Ctrl Pts',(0.0889444345892795,-0.790988886332396,
1.65492528091492));
#54810=CARTESIAN_POINT('Ctrl Pts',(0.454596361508265,-0.653388612426953,
1.6667638406654));
#54811=CARTESIAN_POINT('Ctrl Pts',(0.710730957463525,-0.358379738334567,
1.67860240041587));
#54812=CARTESIAN_POINT('Ctrl Pts',(0.795642543105968,0.0229668096530947,
1.69044096016635));
#54813=CARTESIAN_POINT('Ctrl Pts',(0.688874970927933,0.398780397179714,
1.70227951991682));
#54814=CARTESIAN_POINT('Ctrl Pts',(0.416149739226554,0.678523341741051,
1.7141180796673));
#54815=CARTESIAN_POINT('Ctrl Pts',(0.0431693964412828,0.79480244964184,
1.72595663941777));
#54816=CARTESIAN_POINT('Ctrl Pts',(-0.340210935164571,0.719604787602345,
1.73779519916825));
#54817=CARTESIAN_POINT('Ctrl Pts',(-0.641630660090076,0.471046310651245,
1.74963375891873));
#54818=CARTESIAN_POINT('Ctrl Pts',(-0.788474406614834,0.109007526616991,
1.7614723186692));
#54819=CARTESIAN_POINT('Ctrl Pts',(-0.745365879304481,-0.279292385707923,
1.77331087841968));
#54820=CARTESIAN_POINT('Ctrl Pts',(-0.522690402927433,-0.600307648987884,
1.78514943817015));
#54821=CARTESIAN_POINT('Ctrl Pts',(-0.174092981950916,-0.776702107877354,
1.79698799792063));
#54822=CARTESIAN_POINT('Ctrl Pts',(0.216445379026807,-0.765980370925967,
1.8088265576711));
#54823=CARTESIAN_POINT('Ctrl Pts',(0.554839635437107,-0.570725424081958,
1.82066511742158));
#54824=CARTESIAN_POINT('Ctrl Pts',(0.759566838762484,-0.237976360587295,
1.83250367717205));
#54825=CARTESIAN_POINT('Ctrl Pts',(0.781305923586716,0.152103860944654,
1.84434223692253));
#54826=CARTESIAN_POINT('Ctrl Pts',(0.614819702046,0.505540566839355,1.856180796673));
#54827=CARTESIAN_POINT('Ctrl Pts',(0.300216560764099,0.737186914827925,
1.86801935642348));
#54828=CARTESIAN_POINT('Ctrl Pts',(-0.086712096579095,0.791236717450754,
1.87985791617396));
#54829=CARTESIAN_POINT('Ctrl Pts',(-0.452750843260733,0.654668774793751,
1.89169647592443));
#54830=CARTESIAN_POINT('Ctrl Pts',(-0.709716864894072,0.360383826510688,
1.90353503567491));
#54831=CARTESIAN_POINT('Ctrl Pts',(-0.795704182424333,-0.0207216027410379,
1.91537359542538));
#54832=CARTESIAN_POINT('Ctrl Pts',(-0.689997492524418,-0.396834967118559,
1.92721215517585));
#54833=CARTESIAN_POINT('Ctrl Pts',(-0.418062715156936,-0.677346363895615,
1.93905071492633));
#54834=CARTESIAN_POINT('Ctrl Pts',(-0.045411969437408,-0.794677471931438,
1.95088927467681));
#54835=CARTESIAN_POINT('Ctrl Pts',(0.338179025852439,-0.720561916897015,
1.96272783442728));
#54836=CARTESIAN_POINT('Ctrl Pts',(0.640298924230299,-0.47285496710385,
1.97456639417776));
#54837=CARTESIAN_POINT('Ctrl Pts',(0.78816367389499,-0.111231978262933,
1.98640495392823));
#54838=CARTESIAN_POINT('Ctrl Pts',(0.746151009345457,0.277188021287037,
1.99824351367871));
#54839=CARTESIAN_POINT('Ctrl Pts',(0.524382247875355,0.598830361905442,
2.01008207342918));
#54840=CARTESIAN_POINT('Ctrl Pts',(0.176283960019321,0.776207743104037,
2.02192063317966));
#54841=CARTESIAN_POINT('Ctrl Pts',(-0.214283103861841,0.766588125213539,
2.03375919293014));
#54842=CARTESIAN_POINT('Ctrl Pts',(-0.553226969512226,0.572288687373625,
2.04559775268061));
#54843=CARTESIAN_POINT('Ctrl Pts',(-0.758892310758026,0.240118911410088,
2.05743631243109));
#54844=CARTESIAN_POINT('Ctrl Pts',(-0.781731996299233,-0.149898950293078,
2.06927487218156));
#54845=CARTESIAN_POINT('Ctrl Pts',(-0.616243805965499,-0.5038029747276,
2.08111343193204));
#54846=CARTESIAN_POINT('Ctrl Pts',(-0.302295462815519,-0.736338230417797,
2.09295199168251));
#54847=CARTESIAN_POINT('Ctrl Pts',(0.0844789294252334,-0.791475498675642,
2.10479055143299));
#54848=CARTESIAN_POINT('Ctrl Pts',(0.450901993898189,-0.655949162858557,
2.11662911118346));
#54849=CARTESIAN_POINT('Ctrl Pts',(0.708696584512405,-0.36237427167447,
2.12846767093394));
#54850=CARTESIAN_POINT('Ctrl Pts',(0.795760491783062,0.0184546790760481,
2.14030623068441));
#54851=CARTESIAN_POINT('Ctrl Pts',(0.691113159087595,0.394931908954148,
2.15214479043489));
#54852=CARTESIAN_POINT('Ctrl Pts',(0.51034735958526,0.582332862568382,2.16003716360187));
#54853=CARTESIAN_POINT('Ctrl Pts',(0.403075861660766,0.648960285569488,
2.16398335018536));
#54854=CARTESIAN_POINT('Ctrl Pts',(0.426788104729872,-0.598886528201364,
0.783516649814636));
#54855=CARTESIAN_POINT('Ctrl Pts',(0.525782536893907,-0.528339531245219,
0.787462836398128));
#54856=CARTESIAN_POINT('Ctrl Pts',(0.688021527733875,-0.337286270837092,
0.795355209565113));
#54857=CARTESIAN_POINT('Ctrl Pts',(0.765609474074376,0.0307725378763002,
0.807193769315585));
#54858=CARTESIAN_POINT('Ctrl Pts',(0.658755783400898,0.391327161667553,
0.819032329066062));
#54859=CARTESIAN_POINT('Ctrl Pts',(0.393199817489799,0.657650981834122,
0.830870888816538));
#54860=CARTESIAN_POINT('Ctrl Pts',(0.0329179280634981,0.765517096447697,
0.842709448567012));
#54861=CARTESIAN_POINT('Ctrl Pts',(-0.33529440331804,0.688972852766278,
0.854548008317488));
#54862=CARTESIAN_POINT('Ctrl Pts',(-0.622730501713728,0.44644168285129,
0.866386568067963));
#54863=CARTESIAN_POINT('Ctrl Pts',(-0.760143917763996,0.0963606107249503,
0.878225127818438));
#54864=CARTESIAN_POINT('Ctrl Pts',(-0.714430171726262,-0.276936261191463,
0.890063687568915));
#54865=CARTESIAN_POINT('Ctrl Pts',(-0.496602242944024,-0.583515365048949,
0.90190224731939));
#54866=CARTESIAN_POINT('Ctrl Pts',(-0.15913729329712,-0.749519484998093,
0.913740807069864));
#54867=CARTESIAN_POINT('Ctrl Pts',(0.21666560180481,-0.734955817767558,
0.925579366820341));
#54868=CARTESIAN_POINT('Ctrl Pts',(0.540271339449054,-0.543333196526847,
0.937417926570815));
#54869=CARTESIAN_POINT('Ctrl Pts',(0.733719688284525,-0.220815503453764,
0.949256486321292));
#54870=CARTESIAN_POINT('Ctrl Pts',(0.750406785607549,0.15489908152449,0.961095046071766));
#54871=CARTESIAN_POINT('Ctrl Pts',(0.586312523184101,0.493296763389096,
0.972933605822241));
#54872=CARTESIAN_POINT('Ctrl Pts',(0.280969038263487,0.712853749846213,
0.984772165572717));
#54873=CARTESIAN_POINT('Ctrl Pts',(-0.0920630200335293,0.760676324793167,
0.996610725323192));
#54874=CARTESIAN_POINT('Ctrl Pts',(-0.442916070538986,0.625243492092964,
1.00844928507367));
#54875=CARTESIAN_POINT('Ctrl Pts',(-0.68706570238818,0.3391825332396,1.02028784482414));
#54876=CARTESIAN_POINT('Ctrl Pts',(-0.765693547668255,-0.0285912792142752,
1.03212640457462));
#54877=CARTESIAN_POINT('Ctrl Pts',(-0.659857281978897,-0.38947713358653,
1.04396496432509));
#54878=CARTESIAN_POINT('Ctrl Pts',(-0.395054041498636,-0.656533605002734,
1.05580352407557));
#54879=CARTESIAN_POINT('Ctrl Pts',(-0.0350778786757769,-0.76542381240988,
1.06764208382604));
#54880=CARTESIAN_POINT('Ctrl Pts',(0.333348936140538,-0.689914891102141,
1.07948064357652));
#54881=CARTESIAN_POINT('Ctrl Pts',(0.621468276333288,-0.448197781895396,
1.091319203327));
#54882=CARTESIAN_POINT('Ctrl Pts',(0.759868981126513,-0.0985048308867328,
1.10315776307747));
#54883=CARTESIAN_POINT('Ctrl Pts',(0.715208777955099,0.274919031939008,
1.11499632282795));
#54884=CARTESIAN_POINT('Ctrl Pts',(0.498246807599315,0.582111835391569,
1.12683488257842));
#54885=CARTESIAN_POINT('Ctrl Pts',(0.161251627236223,0.749067408782359,
1.13867344232889));
#54886=CARTESIAN_POINT('Ctrl Pts',(-0.214590867632146,0.735564293393103,
1.15051200207937));
#54887=CARTESIAN_POINT('Ctrl Pts',(-0.538736030400698,0.544855540243667,
1.16235056182985));
#54888=CARTESIAN_POINT('Ctrl Pts',(-0.733093678047651,0.222885013835951,
1.17418912158032));
#54889=CARTESIAN_POINT('Ctrl Pts',(-0.75084088671136,-0.152780996948527,
1.1860276813308));
#54890=CARTESIAN_POINT('Ctrl Pts',(-0.587702155993064,-0.491640362487864,
1.19786624108127));
#54891=CARTESIAN_POINT('Ctrl Pts',(-0.28297942466279,-0.712058084290603,
1.20970480083175));
#54892=CARTESIAN_POINT('Ctrl Pts',(0.0899162044968808,-0.760933076134142,
1.22154336058222));
#54893=CARTESIAN_POINT('Ctrl Pts',(0.441150017679374,-0.626490807664069,
1.2333819203327));
#54894=CARTESIAN_POINT('Ctrl Pts',(0.686105874015599,-0.341119920009637,
1.24522048008317));
#54895=CARTESIAN_POINT('Ctrl Pts',(0.765771177142334,0.0264305589069589,
1.25705903983365));
#54896=CARTESIAN_POINT('Ctrl Pts',(0.660953667491311,0.387613621556152,
1.26889759958413));
#54897=CARTESIAN_POINT('Ctrl Pts',(0.396905051559164,0.655416241966056,
1.2807361593346));
#54898=CARTESIAN_POINT('Ctrl Pts',(0.0372375843265769,0.765321783630658,
1.29257471908508));
#54899=CARTESIAN_POINT('Ctrl Pts',(-0.331400832065067,0.690852776423943,
1.30441327883555));
#54900=CARTESIAN_POINT('Ctrl Pts',(-0.620201093821009,0.449949634302901,
1.31625183858603));
#54901=CARTESIAN_POINT('Ctrl Pts',(-0.759587998570078,0.1006486095999,1.3280903983365));
#54902=CARTESIAN_POINT('Ctrl Pts',(-0.715981687184573,-0.272899787105857,
1.33992895808698));
#54903=CARTESIAN_POINT('Ctrl Pts',(-0.49988740616552,-0.580703583029415,
1.35176751783745));
#54904=CARTESIAN_POINT('Ctrl Pts',(-0.163364676656491,-0.748609412582429,
1.36360607758793));
#54905=CARTESIAN_POINT('Ctrl Pts',(0.212514424517749,-0.736166889745784,
1.3754446373384));
#54906=CARTESIAN_POINT('Ctrl Pts',(0.537196431884951,-0.546373556970108,
1.38728319708888));
#54907=CARTESIAN_POINT('Ctrl Pts',(0.732461830575209,-0.22495274378523,
1.39912175683935));
#54908=CARTESIAN_POINT('Ctrl Pts',(0.751269009381666,0.150661692970645,
1.41096031658983));
#54909=CARTESIAN_POINT('Ctrl Pts',(0.589087109282469,0.489980048433928,
1.4227988763403));
#54910=CARTESIAN_POINT('Ctrl Pts',(0.284987557885531,0.711256748324071,
1.43463743609078));
#54911=CARTESIAN_POINT('Ctrl Pts',(-0.0877686730192269,0.761183769021999,
1.44647599584126));
#54912=CARTESIAN_POINT('Ctrl Pts',(-0.439380452218736,0.627733134695109,
1.45831455559173));
#54913=CARTESIAN_POINT('Ctrl Pts',(-0.685140582617146,0.343054590753614,
1.47015311534221));
#54914=CARTESIAN_POINT('Ctrl Pts',(-0.765842709264246,-0.0242696281984333,
1.48199167509268));
#54915=CARTESIAN_POINT('Ctrl Pts',(-0.662044790248036,-0.385747023179083,
1.49383023484316));
#54916=CARTESIAN_POINT('Ctrl Pts',(-0.398752901315645,-0.654293660276825,
1.50566879459363));
#54917=CARTESIAN_POINT('Ctrl Pts',(-0.0393969934781305,-0.765213661071844,
1.51750735434411));
#54918=CARTESIAN_POINT('Ctrl Pts',(0.329450089254417,-0.69178516092523,
1.52934591409458));
#54919=CARTESIAN_POINT('Ctrl Pts',(0.618928973039669,-0.451697904044452,
1.54118447384506));
#54920=CARTESIAN_POINT('Ctrl Pts',(0.759300967894857,-0.102791586912663,
1.55302303359553));
#54921=CARTESIAN_POINT('Ctrl Pts',(0.716748895504719,0.270878369344724,
1.56486159334601));
#54922=CARTESIAN_POINT('Ctrl Pts',(0.501524024444482,0.579290706891713,
1.57670015309648));
#54923=CARTESIAN_POINT('Ctrl Pts',(0.165476425307159,0.748145455679345,
1.58853871284696));
#54924=CARTESIAN_POINT('Ctrl Pts',(-0.210436289285403,0.736763624467089,
1.60037727259744));
#54925=CARTESIAN_POINT('Ctrl Pts',(-0.535652556013789,0.54788722326952,
1.61221583234791));
#54926=CARTESIAN_POINT('Ctrl Pts',(-0.731824150972487,0.227018682578084,
1.62405439209838));
#54927=CARTESIAN_POINT('Ctrl Pts',(-0.751691150172023,-0.148541189368984,
1.63589295184886));
#54928=CARTESIAN_POINT('Ctrl Pts',(-0.59046737204382,-0.488315832978776,
1.64773151159934));
#54929=CARTESIAN_POINT('Ctrl Pts',(-0.286993421932599,-0.710449749069916,
1.65957007134981));
#54930=CARTESIAN_POINT('Ctrl Pts',(0.0856204426951459,-0.761428401084946,
1.67140863110029));
#54931=CARTESIAN_POINT('Ctrl Pts',(0.437607388249466,-0.628970463484234,
1.68324719085076));
#54932=CARTESIAN_POINT('Ctrl Pts',(0.684169835877579,-0.344986529970863,
1.69508575060124));
#54933=CARTESIAN_POINT('Ctrl Pts',(0.765908143465054,0.0221085042462033,
1.70692431035171));
#54934=CARTESIAN_POINT('Ctrl Pts',(0.663130641560838,0.383877353342446,
1.71876287010219));
#54935=CARTESIAN_POINT('Ctrl Pts',(0.400597576054987,0.653165868861011,
1.73060142985266));
#54936=CARTESIAN_POINT('Ctrl Pts',(0.0415560889363424,0.765099445600639,
1.74243998960314));
#54937=CARTESIAN_POINT('Ctrl Pts',(-0.327496723241085,0.692712037178827,
1.75427854935361));
#54938=CARTESIAN_POINT('Ctrl Pts',(-0.617651924118387,0.453442577201289,
1.76611710910409));
#54939=CARTESIAN_POINT('Ctrl Pts',(-0.759007891386282,0.104933745761025,
1.77795566885456));
#54940=CARTESIAN_POINT('Ctrl Pts',(-0.717510396806747,-0.268854794750451,
1.78979422860504));
#54941=CARTESIAN_POINT('Ctrl Pts',(-0.503156649404848,-0.577873218228538,
1.80163278835552));
#54942=CARTESIAN_POINT('Ctrl Pts',(-0.16758685637372,-0.747675541767138,
1.81347134810599));
#54943=CARTESIAN_POINT('Ctrl Pts',(0.208356478481988,-0.737354492805756,
1.82530990785647));
#54944=CARTESIAN_POINT('Ctrl Pts',(0.534104415080109,-0.549396527089301,
1.83714846760694));
#54945=CARTESIAN_POINT('Ctrl Pts',(0.731180644316946,-0.229082813765163,
1.84898702735742));
#54946=CARTESIAN_POINT('Ctrl Pts',(0.752107305721148,0.146419503028601,
1.86082558710789));
#54947=CARTESIAN_POINT('Ctrl Pts',(0.591842933287032,0.486647729371899,
1.87266414685837));
#54948=CARTESIAN_POINT('Ctrl Pts',(0.288997000832408,0.709637092956943,
1.88450270660884));
#54949=CARTESIAN_POINT('Ctrl Pts',(-0.0834715306293183,0.761666970368852,
1.89634126635932));
#54950=CARTESIAN_POINT('Ctrl Pts',(-0.43583083988997,0.630202784191798,
1.90817982610979));
#54951=CARTESIAN_POINT('Ctrl Pts',(-0.683193641525102,0.346915722254021,
1.92001838586027));
#54952=CARTESIAN_POINT('Ctrl Pts',(-0.765967479226197,-0.0199472042093853,
1.93185694561075));
#54953=CARTESIAN_POINT('Ctrl Pts',(-0.664211212778921,-0.382004627029242,
1.94369550536122));
#54954=CARTESIAN_POINT('Ctrl Pts',(-0.402439061098776,-0.652032876508719,
1.9555340651117));
#54955=CARTESIAN_POINT('Ctrl Pts',(-0.043714853490764,-0.764979138501708,
1.96737262486217));
#54956=CARTESIAN_POINT('Ctrl Pts',(0.325540749541049,-0.69363339706272,
1.97921118461265));
#54957=CARTESIAN_POINT('Ctrl Pts',(0.616369957299513,-0.45518364134848,
1.99104974436312));
#54958=CARTESIAN_POINT('Ctrl Pts',(0.758708771231593,-0.10707506618831,
2.0028883041136));
#54959=CARTESIAN_POINT('Ctrl Pts',(0.718266185316642,0.266829073701797,
2.01472686386407));
#54960=CARTESIAN_POINT('Ctrl Pts',(0.504785267475012,0.576451139662625,
2.02656542361455));
#54961=CARTESIAN_POINT('Ctrl Pts',(0.169695954183138,0.747199652174499,
2.03840398336502));
#54962=CARTESIAN_POINT('Ctrl Pts',(-0.206275010903853,0.737939534370098,
2.0502425431155));
#54963=CARTESIAN_POINT('Ctrl Pts',(-0.532552016989714,0.550901368799743,
2.06208110286597));
#54964=CARTESIAN_POINT('Ctrl Pts',(-0.730531324473397,0.231145294130476,
2.07391966261645));
#54965=CARTESIAN_POINT('Ctrl Pts',(-0.752517455433544,-0.144296993318319,
2.08575822236692));
#54966=CARTESIAN_POINT('Ctrl Pts',(-0.593213816227538,-0.484975073780585,
2.09759678211741));
#54967=CARTESIAN_POINT('Ctrl Pts',(-0.290998211079956,-0.708820125203544,
2.10943534186787));
#54968=CARTESIAN_POINT('Ctrl Pts',(0.0813218204062015,-0.761896827967887,
2.12127390161836));
#54969=CARTESIAN_POINT('Ctrl Pts',(0.434051084904416,-0.631435322162685,
2.13311246136882));
#54970=CARTESIAN_POINT('Ctrl Pts',(0.682211490608578,-0.348831781385437,
2.1449510211193));
#54971=CARTESIAN_POINT('Ctrl Pts',(0.766021684216589,0.0177649990084773,
2.15678958086977));
#54972=CARTESIAN_POINT('Ctrl Pts',(0.665285185146957,0.38017268910908,2.16862814062025));
#54973=CARTESIAN_POINT('Ctrl Pts',(0.491274884794816,0.560570177541447,
2.17652051378724));
#54974=CARTESIAN_POINT('Ctrl Pts',(0.388012289633257,0.624707630090715,
2.18046670037073));
#54975=CARTESIAN_POINT('Ctrl Pts',(0.410219162127157,-0.575636310115765,
0.8));
#54976=CARTESIAN_POINT('Ctrl Pts',(0.50537039190027,-0.507828117569598,
0.803946186583492));
#54977=CARTESIAN_POINT('Ctrl Pts',(0.661310874189135,-0.324192005087297,
0.811838559750475));
#54978=CARTESIAN_POINT('Ctrl Pts',(0.735886669498874,0.0295778738072663,
0.82367711950095));
#54979=CARTESIAN_POINT('Ctrl Pts',(0.633181296569113,0.376134898320248,
0.835515679251426));
#54980=CARTESIAN_POINT('Ctrl Pts',(0.377934853131171,0.632119386061258,
0.847354239001902));
#54981=CARTESIAN_POINT('Ctrl Pts',(0.0316399747779213,0.735797878194255,
0.859192798752376));
#54982=CARTESIAN_POINT('Ctrl Pts',(-0.322277466664887,0.662225266491492,
0.871031358502852));
#54983=CARTESIAN_POINT('Ctrl Pts',(-0.598554603122584,0.429109740989168,
0.882869918253328));
#54984=CARTESIAN_POINT('Ctrl Pts',(-0.730633299254123,0.0926196596286783,
0.894708478003802));
#54985=CARTESIAN_POINT('Ctrl Pts',(-0.686694270988179,-0.266184928233867,
0.906547037754278));
#54986=CARTESIAN_POINT('Ctrl Pts',(-0.47732294727357,-0.560861892554869,
0.918385597504754));
#54987=CARTESIAN_POINT('Ctrl Pts',(-0.152959200118396,-0.720421332568536,
0.930224157255227));
#54988=CARTESIAN_POINT('Ctrl Pts',(0.20825412107116,-0.70642306199211,0.942062717005705));
#54989=CARTESIAN_POINT('Ctrl Pts',(0.519296704228398,-0.522239692636662,
0.953901276756179));
#54990=CARTESIAN_POINT('Ctrl Pts',(0.705234922034154,-0.212242913538608,
0.965739836506655));
#54991=CARTESIAN_POINT('Ctrl Pts',(0.721274186030318,0.148885525939063,
0.97757839625713));
#54992=CARTESIAN_POINT('Ctrl Pts',(0.563550458271255,0.474145794399759,
0.989416956007605));
#54993=CARTESIAN_POINT('Ctrl Pts',(0.270061143182683,0.68517904960402,1.00125551575808));
#54994=CARTESIAN_POINT('Ctrl Pts',(-0.0884889117632597,0.731145036959546,
1.01309407550856));
#54995=CARTESIAN_POINT('Ctrl Pts',(-0.425721001442049,0.600970033160064,
1.02493263525903));
#54996=CARTESIAN_POINT('Ctrl Pts',(-0.660392156286491,0.326014650014156,
1.03677119500951));
#54997=CARTESIAN_POINT('Ctrl Pts',(-0.735967479153258,-0.0274812968624031,
1.04860975475998));
#54998=CARTESIAN_POINT('Ctrl Pts',(-0.634240032318171,-0.374356692787108,
1.06044831451046));
#54999=CARTESIAN_POINT('Ctrl Pts',(-0.379717091696098,-0.631045388490867,
1.07228687426093));
#55000=CARTESIAN_POINT('Ctrl Pts',(-0.0337160709028718,-0.73570821566756,
1.08412543401141));
#55001=CARTESIAN_POINT('Ctrl Pts',(0.320407527210959,-0.663130732629247,
1.09596399376188));
#55002=CARTESIAN_POINT('Ctrl Pts',(0.597341380372839,-0.430797664036932,
1.10780255351236));
#55003=CARTESIAN_POINT('Ctrl Pts',(0.730369036319385,-0.094680635997126,
1.11964111326283));
#55004=CARTESIAN_POINT('Ctrl Pts',(0.687442649847106,0.264246012681654,
1.13147967301331));
#55005=CARTESIAN_POINT('Ctrl Pts',(0.478903665966244,0.559512851300696,
1.14331823276378));
#55006=CARTESIAN_POINT('Ctrl Pts',(0.154991450519341,0.719986807040808,
1.15515679251426));
#55007=CARTESIAN_POINT('Ctrl Pts',(-0.206259933078302,0.707007915127706,
1.16699535226474));
#55008=CARTESIAN_POINT('Ctrl Pts',(-0.51782099957674,0.523702935302196,
1.17883391201521));
#55009=CARTESIAN_POINT('Ctrl Pts',(-0.704633215023091,0.214232080541122,
1.19067247176569));
#55010=CARTESIAN_POINT('Ctrl Pts',(-0.721691434283282,-0.146849670510018,
1.20251103151616));
#55011=CARTESIAN_POINT('Ctrl Pts',(-0.564886142186152,-0.472553698972733,
1.21434959126664));
#55012=CARTESIAN_POINT('Ctrl Pts',(-0.271993481537794,-0.684414273702493,
1.22618815101711));
#55013=CARTESIAN_POINT('Ctrl Pts',(0.0864254407786529,-0.731391820594802,
1.23802671076759));
#55014=CARTESIAN_POINT('Ctrl Pts',(0.42402351100988,-0.602168924935201,
1.24986527051806));
#55015=CARTESIAN_POINT('Ctrl Pts',(0.65946959076411,-0.327876822761505,
1.26170383026854));
#55016=CARTESIAN_POINT('Ctrl Pts',(0.7360420948641,0.02540446092383,1.27354239001901));
#55017=CARTESIAN_POINT('Ctrl Pts',(0.635293853503172,0.372565526784018,
1.28538094976949));
#55018=CARTESIAN_POINT('Ctrl Pts',(0.381496241085932,0.62997140417964,1.29721950951997));
#55019=CARTESIAN_POINT('Ctrl Pts',(0.0357919315763396,0.735610147891393,
1.30905806927044));
#55020=CARTESIAN_POINT('Ctrl Pts',(-0.318535053229798,0.664032206982953,
1.32089662902092));
#55021=CARTESIAN_POINT('Ctrl Pts',(-0.596123392939055,0.432481505312761,
1.33273518877139));
#55022=CARTESIAN_POINT('Ctrl Pts',(-0.730098962182839,0.0967411880550564,
1.34457374852187));
#55023=CARTESIAN_POINT('Ctrl Pts',(-0.68818555287791,-0.262305159798444,
1.35641230827234));
#55024=CARTESIAN_POINT('Ctrl Pts',(-0.480480572542965,-0.558159270688526,
1.36825086802282));
#55025=CARTESIAN_POINT('Ctrl Pts',(-0.157022466269567,-0.719546591356936,
1.38008942777329));
#55026=CARTESIAN_POINT('Ctrl Pts',(0.204264102488947,-0.707587117237976,
1.39192798752377));
#55027=CARTESIAN_POINT('Ctrl Pts',(0.516341171985148,-0.525162018961544,
1.40376654727424));
#55028=CARTESIAN_POINT('Ctrl Pts',(0.704025897392014,-0.216219536231424,
1.41560510702472));
#55029=CARTESIAN_POINT('Ctrl Pts',(0.722102936199932,0.144812643019176,
1.42744366677519));
#55030=CARTESIAN_POINT('Ctrl Pts',(0.566217328251717,0.470957842311017,
1.43928222652567));
#55031=CARTESIAN_POINT('Ctrl Pts',(0.273923654190083,0.683644047529059,
1.45112078627614));
#55032=CARTESIAN_POINT('Ctrl Pts',(-0.0843612816475947,0.73163278098069,
1.46295934602662));
#55033=CARTESIAN_POINT('Ctrl Pts',(-0.422322644344321,0.603363021837419,
1.4747979057771));
#55034=CARTESIAN_POINT('Ctrl Pts',(-0.658541774303685,0.32973638492547,
1.48663646552757));
#55035=CARTESIAN_POINT('Ctrl Pts',(-0.736110849936677,-0.0233274227523295,
1.49847502527805));
#55036=CARTESIAN_POINT('Ctrl Pts',(-0.636342616245341,-0.370771394253652,
1.51031358502852));
#55037=CARTESIAN_POINT('Ctrl Pts',(-0.383272352862338,-0.628892403816528,
1.522152144779));
#55038=CARTESIAN_POINT('Ctrl Pts',(-0.0378675072613757,-0.735506222910841,
1.53399070452947));
#55039=CARTESIAN_POINT('Ctrl Pts',(0.316660042955515,-0.664928394071252,
1.54582926427995));
#55040=CARTESIAN_POINT('Ctrl Pts',(0.594900658951714,-0.434161903010362,
1.55766782403042));
#55041=CARTESIAN_POINT('Ctrl Pts',(0.729823074730051,-0.0988009698248782,
1.5695063837809));
#55042=CARTESIAN_POINT('Ctrl Pts',(0.688922976322423,0.260362218345552,
1.58134494353137));
#55043=CARTESIAN_POINT('Ctrl Pts',(0.482053653356788,0.556801245806918,
1.59318350328185));
#55044=CARTESIAN_POINT('Ctrl Pts',(0.159052231749204,0.719100646378767,
1.60502206303232));
#55045=CARTESIAN_POINT('Ctrl Pts',(-0.202266645473739,0.708160685279523,
1.6168606227828));
#55046=CARTESIAN_POINT('Ctrl Pts',(-0.514857233095386,0.526616921087925,
1.62869918253327));
#55047=CARTESIAN_POINT('Ctrl Pts',(-0.703412974048005,0.218205270302308,
1.64053774228375));
#55048=CARTESIAN_POINT('Ctrl Pts',(-0.722508688467628,-0.142774462476838,
1.65237630203423));
#55049=CARTESIAN_POINT('Ctrl Pts',(-0.567544005886828,-0.469358235709884,
1.6642148617847));
#55050=CARTESIAN_POINT('Ctrl Pts',(-0.275851645761568,-0.682868377930474,
1.67605342153517));
#55051=CARTESIAN_POINT('Ctrl Pts',(0.0822964508010132,-0.731867915837495,
1.68789198128565));
#55052=CARTESIAN_POINT('Ctrl Pts',(0.420618414990665,-0.604552314541516,
1.69973054103613));
#55053=CARTESIAN_POINT('Ctrl Pts',(0.657608714291634,-0.331593321607157,
1.7115691007866));
#55054=CARTESIAN_POINT('Ctrl Pts',(0.736173743824141,0.0212501988393111,
1.72340766053708));
#55055=CARTESIAN_POINT('Ctrl Pts',(0.637386312193742,0.36897430950518,1.73524622028755));
#55056=CARTESIAN_POINT('Ctrl Pts',(0.38504541288342,0.627808395980971,1.74708478003803));
#55057=CARTESIAN_POINT('Ctrl Pts',(0.0399427814314016,0.735396441559441,
1.7589233397885));
#55058=CARTESIAN_POINT('Ctrl Pts',(-0.314782511317597,0.665819286755307,
1.77076189953898));
#55059=CARTESIAN_POINT('Ctrl Pts',(-0.5936731881467,0.435838843751334,1.78260045928945));
#55060=CARTESIAN_POINT('Ctrl Pts',(-0.729541376157727,0.100859964905057,
1.79443901903993));
#55061=CARTESIAN_POINT('Ctrl Pts',(-0.689654914309015,-0.258417203792979,
1.8062775787904));
#55062=CARTESIAN_POINT('Ctrl Pts',(-0.483622895882263,-0.55543878746919,
1.81811613854088));
#55063=CARTESIAN_POINT('Ctrl Pts',(-0.161080730796523,-0.718648975656924,
1.82995469829136));
#55064=CARTESIAN_POINT('Ctrl Pts',(0.200267577937169,-0.708728614685542,
1.84179325804183));
#55065=CARTESIAN_POINT('Ctrl Pts',(0.513369194723111,-0.528067630096644,
1.85363181779231));
#55066=CARTESIAN_POINT('Ctrl Pts',(0.702794449871408,-0.22018926694303,
1.86547037754278));
#55067=CARTESIAN_POINT('Ctrl Pts',(0.722908687855579,0.140735145112547,
1.87730893729326));
#55068=CARTESIAN_POINT('Ctrl Pts',(0.568866164528063,0.467754891904443,
1.88914749704373));
#55069=CARTESIAN_POINT('Ctrl Pts',(0.277777440900717,0.68208727108596,1.90098605679421));
#55070=CARTESIAN_POINT('Ctrl Pts',(-0.0802309646795408,0.732097223286951,
1.91282461654468));
#55071=CARTESIAN_POINT('Ctrl Pts',(-0.418910836519209,0.605736793589845,
1.92466317629516));
#55072=CARTESIAN_POINT('Ctrl Pts',(-0.656670418156131,0.333447617997354,
1.93650173604563));
#55073=CARTESIAN_POINT('Ctrl Pts',(-0.736230776028063,-0.0191728056777326,
1.94834029579611));
#55074=CARTESIAN_POINT('Ctrl Pts',(-0.638424933033424,-0.367174286939925,
1.96017885554658));
#55075=CARTESIAN_POINT('Ctrl Pts',(-0.386815407040617,-0.626719389121822,
1.97201741529706));
#55076=CARTESIAN_POINT('Ctrl Pts',(-0.0420177375441198,-0.735280805071978,
1.98385597504754));
#55077=CARTESIAN_POINT('Ctrl Pts',(0.312902473229659,-0.666704877228424,
1.99569453479801));
#55078=CARTESIAN_POINT('Ctrl Pts',(0.592440990368726,-0.437512315593109,
2.00753309454849));
#55079=CARTESIAN_POINT('Ctrl Pts',(0.729253868568196,-0.102918154113688,
2.01937165429896));
#55080=CARTESIAN_POINT('Ctrl Pts',(0.690381361287827,0.256470126116556,
2.03121021404944));
#55081=CARTESIAN_POINT('Ctrl Pts',(0.485188287074669,0.554071917419808,
2.04304877379991));
#55082=CARTESIAN_POINT('Ctrl Pts',(0.163107948346954,0.718191561244962,
2.05488733355038));
#55083=CARTESIAN_POINT('Ctrl Pts',(-0.198266917945865,0.709290943526656,
2.06672589330087));
#55084=CARTESIAN_POINT('Ctrl Pts',(-0.511877064467201,0.529514050225861,
2.07856445305133));
#55085=CARTESIAN_POINT('Ctrl Pts',(-0.70217033818877,0.222171676850865,
2.09040301280182));
#55086=CARTESIAN_POINT('Ctrl Pts',(-0.723302914567855,-0.138695036343561,
2.10224157255228));
#55087=CARTESIAN_POINT('Ctrl Pts',(-0.570183826489577,-0.466147172833569,
2.11408013230277));
#55088=CARTESIAN_POINT('Ctrl Pts',(-0.279700959344392,-0.681302019989293,
2.12591869205323));
#55089=CARTESIAN_POINT('Ctrl Pts',(0.078164711387169,-0.732318157260131,
2.13775725180372));
#55090=CARTESIAN_POINT('Ctrl Pts',(0.417200175910644,-0.606921481466812,
2.14959581155419));
#55091=CARTESIAN_POINT('Ctrl Pts',(0.655726396704751,-0.335289291096404,
2.16143437130467));
#55092=CARTESIAN_POINT('Ctrl Pts',(0.736282876650117,0.0170753189409072,
2.17327293105514));
#55093=CARTESIAN_POINT('Ctrl Pts',(0.639457211206318,0.365413469264011,
2.18511149080562));
#55094=CARTESIAN_POINT('Ctrl Pts',(0.472202410004372,0.538807492514513,
2.1930038639726));
#55095=CARTESIAN_POINT('Ctrl Pts',(0.372948717605748,0.600454974611942,
2.19695005055609));
#55096=CARTESIAN_POINT('Ctrl Pts',(0.345504974425206,0.713245911452249,
0.8));
#55097=CARTESIAN_POINT('Ctrl Pts',(0.36583353368801,0.702081547762358,0.8));
#55098=CARTESIAN_POINT('Ctrl Pts',(0.385637643802227,0.690039175705666,
0.8));
#55099=CARTESIAN_POINT('Ctrl Pts',(0.404853295913343,0.677138077406943,
0.8));
#55100=CARTESIAN_POINT('Ctrl Pts',(0.431589435756686,0.659187837349888,
0.8));
#55101=CARTESIAN_POINT('Ctrl Pts',(0.457187440867682,0.63957581308399,0.8));
#55102=CARTESIAN_POINT('Ctrl Pts',(0.481519180772095,0.618436888473522,
0.8));
#55103=CARTESIAN_POINT('Ctrl Pts',(0.490041012870151,0.611033292718694,
0.8));
#55104=CARTESIAN_POINT('Ctrl Pts',(0.498407317172348,0.603442222277882,
0.8));
#55105=CARTESIAN_POINT('Ctrl Pts',(0.506611886748092,0.595668956909438,
0.8));
#55106=CARTESIAN_POINT('Ctrl Pts',(0.512987438654641,0.589628559983995,
0.8));
#55107=CARTESIAN_POINT('Ctrl Pts',(0.519262318463782,0.583480863158659,
0.8));
#55108=CARTESIAN_POINT('Ctrl Pts',(0.525428333131113,0.577234389533608,
0.8));
#55109=CARTESIAN_POINT('Ctrl Pts',(0.552361828544955,0.549949444912184,
0.8));
#55110=CARTESIAN_POINT('Ctrl Pts',(0.577255825711188,0.520751087178113,
0.8));
#55111=CARTESIAN_POINT('Ctrl Pts',(0.599886914660718,0.48986502862222,0.8));
#55112=CARTESIAN_POINT('Ctrl Pts',(0.609541659734953,0.4766885958677,0.8));
#55113=CARTESIAN_POINT('Ctrl Pts',(0.618783914351497,0.463204566301741,
0.8));
#55114=CARTESIAN_POINT('Ctrl Pts',(0.627593177155457,0.449428880659182,
0.8));
#55115=CARTESIAN_POINT('Ctrl Pts',(0.633449833557471,0.440270400624467,
0.8));
#55116=CARTESIAN_POINT('Ctrl Pts',(0.639117093402895,0.43097907060152,0.8));
#55117=CARTESIAN_POINT('Ctrl Pts',(0.64457466299164,0.421584382346768,0.8));
#55118=CARTESIAN_POINT('Ctrl Pts',(0.650150271728973,0.411986500896801,
0.8));
#55119=CARTESIAN_POINT('Ctrl Pts',(0.655510064988793,0.402276354406898,
0.8));
#55120=CARTESIAN_POINT('Ctrl Pts',(0.660649057912794,0.392459620153433,
0.8));
#55121=CARTESIAN_POINT('Ctrl Pts',(0.677398500727402,0.360464084951061,
0.8));
#55122=CARTESIAN_POINT('Ctrl Pts',(0.691806162809588,0.327337699200768,
0.8));
#55123=CARTESIAN_POINT('Ctrl Pts',(0.703820537250413,0.29335172176486,0.8));
#55124=CARTESIAN_POINT('Ctrl Pts',(0.712004329212203,0.270201605183803,
0.8));
#55125=CARTESIAN_POINT('Ctrl Pts',(0.719076667813015,0.246652090573615,
0.8));
#55126=CARTESIAN_POINT('Ctrl Pts',(0.725007698830821,0.222786213838172,
0.8));
#55127=CARTESIAN_POINT('Ctrl Pts',(0.729682972771009,0.203973378223933,
0.8));
#55128=CARTESIAN_POINT('Ctrl Pts',(0.73364885638524,0.184963897214997,0.8));
#55129=CARTESIAN_POINT('Ctrl Pts',(0.73688566164746,0.165798785722696,0.8));
#55130=CARTESIAN_POINT('Ctrl Pts',(0.738101009586174,0.158602715258016,
0.8));
#55131=CARTESIAN_POINT('Ctrl Pts',(0.739213253909337,0.151385563578606,
0.8));
#55132=CARTESIAN_POINT('Ctrl Pts',(0.740219854302973,0.144162331267803,
0.8));
#55133=CARTESIAN_POINT('Ctrl Pts',(0.745122019678705,0.108985035929166,
0.8));
#55134=CARTESIAN_POINT('Ctrl Pts',(0.747536860054795,0.0735840120457708,
0.8));
#55135=CARTESIAN_POINT('Ctrl Pts',(0.747398095781194,0.038213143437428,
0.8));
#55136=CARTESIAN_POINT('Ctrl Pts',(0.747387383346823,0.0354825550893366,
0.8));
#55137=CARTESIAN_POINT('Ctrl Pts',(0.747361426528289,0.0327521458004539,
0.8));
#55138=CARTESIAN_POINT('Ctrl Pts',(0.747320181801601,0.030022032614301,
0.8));
#55139=CARTESIAN_POINT('Ctrl Pts',(0.746859569917307,-0.000467260926602417,
0.8));
#55140=CARTESIAN_POINT('Ctrl Pts',(0.744494531099263,-0.0309202575391632,
0.8));
#55141=CARTESIAN_POINT('Ctrl Pts',(0.740261770482073,-0.0611646713267921,
0.8));
#55142=CARTESIAN_POINT('Ctrl Pts',(0.737719428203378,-0.0793305112645305,
0.8));
#55143=CARTESIAN_POINT('Ctrl Pts',(0.734502747220283,-0.0974209830990813,
0.8));
#55144=CARTESIAN_POINT('Ctrl Pts',(0.730615146452625,-0.115396704760788,
0.8));
#55145=CARTESIAN_POINT('Ctrl Pts',(0.728559969813086,-0.124899553804686,
0.8));
#55146=CARTESIAN_POINT('Ctrl Pts',(0.72631599569988,-0.134374304191129,
0.8));
#55147=CARTESIAN_POINT('Ctrl Pts',(0.723890962231601,-0.143787847611887,
0.8));
#55148=CARTESIAN_POINT('Ctrl Pts',(0.71517862288476,-0.177607580745754,
0.8));
#55149=CARTESIAN_POINT('Ctrl Pts',(0.704121082802721,-0.210704194639309,
0.8));
#55150=CARTESIAN_POINT('Ctrl Pts',(0.690789930854426,-0.242823645553218,
0.8));
#55151=CARTESIAN_POINT('Ctrl Pts',(0.679792305406727,-0.269320807396919,
0.8));
#55152=CARTESIAN_POINT('Ctrl Pts',(0.667246321255119,-0.295153115200466,
0.8));
#55153=CARTESIAN_POINT('Ctrl Pts',(0.653168640005758,-0.320165218334144,
0.8));
#55154=CARTESIAN_POINT('Ctrl Pts',(0.645345018624938,-0.334065605861727,
0.8));
#55155=CARTESIAN_POINT('Ctrl Pts',(0.637047938644404,-0.347712405880769,
0.8));
#55156=CARTESIAN_POINT('Ctrl Pts',(0.628293128421847,-0.36108455082462,
0.8));
#55157=CARTESIAN_POINT('Ctrl Pts',(0.623632127364847,-0.368203789292754,
0.8));
#55158=CARTESIAN_POINT('Ctrl Pts',(0.618841361406744,-0.375245149184032,
0.8));
#55159=CARTESIAN_POINT('Ctrl Pts',(0.613923051360153,-0.382205232791639,
0.8));
#55160=CARTESIAN_POINT('Ctrl Pts',(0.610216510191735,-0.387450497157415,
0.8));
#55161=CARTESIAN_POINT('Ctrl Pts',(0.606438371485466,-0.392648260874719,
0.8));
#55162=CARTESIAN_POINT('Ctrl Pts',(0.602595484873438,-0.397789698506065,
0.8));
#55163=CARTESIAN_POINT('Ctrl Pts',(0.581986083819865,-0.425363228728034,
0.8));
#55164=CARTESIAN_POINT('Ctrl Pts',(0.559474301213147,-0.451381505199937,
0.8));
#55165=CARTESIAN_POINT('Ctrl Pts',(0.535252367285333,-0.475662926269611,
0.8));
#55166=CARTESIAN_POINT('Ctrl Pts',(0.511393995304302,-0.499579892513297,
0.8));
#55167=CARTESIAN_POINT('Ctrl Pts',(0.485875450752161,-0.521812462744942,
0.8));
#55168=CARTESIAN_POINT('Ctrl Pts',(0.458849939885056,-0.542148155172804,
0.8));
#55169=CARTESIAN_POINT('Ctrl Pts',(0.443140321239726,-0.55396905929933,
0.8));
#55170=CARTESIAN_POINT('Ctrl Pts',(0.426921009928925,-0.565148233479232,
0.8));
#55171=CARTESIAN_POINT('Ctrl Pts',(0.410219162127159,-0.575636310115764,
0.8));
#55172=CARTESIAN_POINT('Ctrl Pts',(0.418139433688274,0.673212941048261,
2.1475));
#55173=CARTESIAN_POINT('Ctrl Pts',(0.529419834375704,0.604095547595317,
2.14355381341651));
#55174=CARTESIAN_POINT('Ctrl Pts',(0.623180483701969,0.506893338197268,
2.13960762683302));
#55175=CARTESIAN_POINT('Ctrl Pts',(0.688153836085317,0.393201105222312,
2.13566144024952));
#55176=CARTESIAN_POINT('Ctrl Pts',(0.753127188468667,0.279508872247353,
2.13171525366603));
#55177=CARTESIAN_POINT('Ctrl Pts',(0.789313243909101,0.149326615695483,
2.12776906708254));
#55178=CARTESIAN_POINT('Ctrl Pts',(0.7923533348071,0.0183919672350275,2.12382288049905));
#55179=CARTESIAN_POINT('Ctrl Pts',(0.795393425705099,-0.112542681225426,
2.11987669391556));
#55180=CARTESIAN_POINT('Ctrl Pts',(0.765287552060666,-0.244229721594463,
2.11593050733207));
#55181=CARTESIAN_POINT('Ctrl Pts',(0.705663152651071,-0.360830948710805,
2.11198432074857));
#55182=CARTESIAN_POINT('Ctrl Pts',(0.646038753241476,-0.477432175827145,
2.10803813416508));
#55183=CARTESIAN_POINT('Ctrl Pts',(0.556895828066718,-0.578947589690789,
2.10409194758159));
#55184=CARTESIAN_POINT('Ctrl Pts',(0.448971554738058,-0.653137157594104,
2.1001457609981));
#55185=CARTESIAN_POINT('Ctrl Pts',(0.341047281409397,-0.72732672549742,
2.09619957441461));
#55186=CARTESIAN_POINT('Ctrl Pts',(0.214341659926831,-0.774190447440409,
2.09225338783112));
#55187=CARTESIAN_POINT('Ctrl Pts',(0.0841173903529904,-0.788089336120012,
2.08830720124762));
#55188=CARTESIAN_POINT('Ctrl Pts',(-0.04610687922085,-0.801988224799615,
2.08436101466413));
#55189=CARTESIAN_POINT('Ctrl Pts',(-0.179849796885967,-0.782922280215831,
2.08041482808064));
#55190=CARTESIAN_POINT('Ctrl Pts',(-0.301001435910588,-0.733185064597701,
2.07646864149715));
#55191=CARTESIAN_POINT('Ctrl Pts',(-0.42215307493521,-0.68344784897957,
2.07252245491366));
#55192=CARTESIAN_POINT('Ctrl Pts',(-0.530713435319334,-0.603039362327094,
2.06857626833016));
#55193=CARTESIAN_POINT('Ctrl Pts',(-0.613605739088308,-0.501646790933058,
2.06463008174667));
#55194=CARTESIAN_POINT('Ctrl Pts',(-0.696498042857281,-0.400254219539023,
2.06068389516318));
#55195=CARTESIAN_POINT('Ctrl Pts',(-0.753722290011102,-0.277877563403429,
2.05673770857969));
#55196=CARTESIAN_POINT('Ctrl Pts',(-0.778385540234301,-0.149256996009377,
2.0527915219962));
#55197=CARTESIAN_POINT('Ctrl Pts',(-0.787807963541229,-0.100118402312424,
2.05128390884297));
#55198=CARTESIAN_POINT('Ctrl Pts',(-0.792477884965536,-0.0500684667399751,
2.04977629568975));
#55199=CARTESIAN_POINT('Ctrl Pts',(-0.792448351156449,-1.30718296499355E-5,
2.04826868253652));
#55200=CARTESIAN_POINT('Origin',(0.,0.,1.095));
#55201=CARTESIAN_POINT('Origin',(0.,0.,2.1475));
#55202=CARTESIAN_POINT('Ctrl Pts',(0.82685,-1.18395083925468E-14,-1.12625));
#55203=CARTESIAN_POINT('Ctrl Pts',(0.826850000000002,0.135161967341259,
-1.12277201246584));
#55204=CARTESIAN_POINT('Ctrl Pts',(0.759329854291363,0.405358483866941,
-1.11581603739752));
#55205=CARTESIAN_POINT('Ctrl Pts',(0.478857035684602,0.715228292912721,
-1.10538207479504));
#55206=CARTESIAN_POINT('Ctrl Pts',(0.0855976892416321,0.856457731826549,
-1.09494811219256));
#55207=CARTESIAN_POINT('Ctrl Pts',(-0.327878991306288,0.795839011623238,
-1.08451414959008));
#55208=CARTESIAN_POINT('Ctrl Pts',(-0.664050737432057,0.547619885496967,
-1.0740801869876));
#55209=CARTESIAN_POINT('Ctrl Pts',(-0.843710039187729,0.170328555651523,
-1.06364622438512));
#55210=CARTESIAN_POINT('Ctrl Pts',(-0.82449358245641,-0.247114352893216,
-1.05321226178264));
#55211=CARTESIAN_POINT('Ctrl Pts',(-0.610938970960348,-0.606308285553778,
-1.04277829918016));
#55212=CARTESIAN_POINT('Ctrl Pts',(-0.253378910006028,-0.822590571742088,
-1.03234433657767));
#55213=CARTESIAN_POINT('Ctrl Pts',(0.163904234062427,-0.844980061330929,
-1.02191037397519));
#55214=CARTESIAN_POINT('Ctrl Pts',(0.542553969616093,-0.668200044521292,
-1.01147641137271));
#55215=CARTESIAN_POINT('Ctrl Pts',(0.793318450980055,-0.333918875136038,
-1.00104244877023));
#55216=CARTESIAN_POINT('Ctrl Pts',(0.857090409214356,0.0790700506594052,
-0.990608486167753));
#55217=CARTESIAN_POINT('Ctrl Pts',(0.718838053513714,0.473421453487905,
-0.980174523565272));
#55218=CARTESIAN_POINT('Ctrl Pts',(0.411148835382887,0.756182953459401,
-0.969740560962792));
#55219=CARTESIAN_POINT('Ctrl Pts',(0.00654795948644188,0.860705030962387,
-0.95930659836031));
#55220=CARTESIAN_POINT('Ctrl Pts',(-0.399596325757388,0.762350837560665,
-0.94887263575783));
#55221=CARTESIAN_POINT('Ctrl Pts',(-0.711552003832334,0.484303387427033,
-0.93843867315535));
#55222=CARTESIAN_POINT('Ctrl Pts',(-0.855788184097906,0.0921010751558536,
-0.928004710552868));
#55223=CARTESIAN_POINT('Ctrl Pts',(-0.798307045430397,-0.321810325775003,
-0.917570747950388));
#55224=CARTESIAN_POINT('Ctrl Pts',(-0.55265743131608,-0.65986800804578,
-0.907136785347908));
#55225=CARTESIAN_POINT('Ctrl Pts',(-0.176741265643775,-0.842388597645019,
-0.896702822745427));
#55226=CARTESIAN_POINT('Ctrl Pts',(0.240834477891071,-0.826350276046739,
-0.886268860142947));
#55227=CARTESIAN_POINT('Ctrl Pts',(0.601643270987137,-0.615533426310559,
-0.875834897540465));
#55228=CARTESIAN_POINT('Ctrl Pts',(0.820639089441999,-0.25962956174058,
-0.865400934937985));
#55229=CARTESIAN_POINT('Ctrl Pts',(0.846202560151337,0.157471431167258,
-0.854966972335505));
#55230=CARTESIAN_POINT('Ctrl Pts',(0.672308132783288,0.537454927447037,
-0.844533009733024));
#55231=CARTESIAN_POINT('Ctrl Pts',(0.33994435853765,0.790755245029512,-0.834099047130543));
#55232=CARTESIAN_POINT('Ctrl Pts',(-0.0725474966321811,0.857667117928168,
-0.823665084528063));
#55233=CARTESIAN_POINT('Ctrl Pts',(-0.467939224870042,0.722418788703158,
-0.813231121925582));
#55234=CARTESIAN_POINT('Ctrl Pts',(-0.753033278981657,0.416889559942566,
-0.802797159323102));
#55235=CARTESIAN_POINT('Ctrl Pts',(-0.860630310410645,0.0130955429679326,
-0.792363196720621));
#55236=CARTESIAN_POINT('Ctrl Pts',(-0.765368687391839,-0.393785216587891,
-0.78192923411814));
#55237=CARTESIAN_POINT('Ctrl Pts',(-0.489702469969954,-0.707847098848631,
-0.771495271515659));
#55238=CARTESIAN_POINT('Ctrl Pts',(-0.0986087769686523,-0.855062765852802,
-0.761061308913179));
#55239=CARTESIAN_POINT('Ctrl Pts',(0.315727931727777,-0.800732100998826,
-0.750627346310698));
#55240=CARTESIAN_POINT('Ctrl Pts',(0.655644598941732,-0.557661352723705,
-0.740193383708218));
#55241=CARTESIAN_POINT('Ctrl Pts',(0.841019670852427,-0.183144581362296,
-0.729759421105738));
#55242=CARTESIAN_POINT('Ctrl Pts',(0.828158500407521,0.234541089461656,
-0.719325458503256));
#55243=CARTESIAN_POINT('Ctrl Pts',(0.620092586381245,0.596943220715433,
-0.708891495900776));
#55244=CARTESIAN_POINT('Ctrl Pts',(0.265865020615963,0.818640223331329,
-0.698457533298295));
#55245=CARTESIAN_POINT('Ctrl Pts',(-0.151029429750584,0.847376029748488,
-0.688023570695815));
#55246=CARTESIAN_POINT('Ctrl Pts',(-0.532324823785285,0.676377340265816,
-0.677589608093333));
#55247=CARTESIAN_POINT('Ctrl Pts',(-0.788146252778425,0.345950153453387,
-0.667155645490855));
#55248=CARTESIAN_POINT('Ctrl Pts',(-0.858194201088189,-0.0660207366037404,
-0.656721682888372));
#55249=CARTESIAN_POINT('Ctrl Pts',(-0.725957708818034,-0.462429918420906,
-0.646287720285893));
#55250=CARTESIAN_POINT('Ctrl Pts',(-0.422606160274217,-0.749840021432158,
-0.635853757683411));
#55251=CARTESIAN_POINT('Ctrl Pts',(-0.0196423670795976,-0.860505782582898,
-0.625419795080932));
#55252=CARTESIAN_POINT('Ctrl Pts',(0.387951316682126,-0.768342241665588,
-0.61498583247845));
#55253=CARTESIAN_POINT('Ctrl Pts',(0.704101228197687,-0.495073211650161,
-0.604551869875971));
#55254=CARTESIAN_POINT('Ctrl Pts',(0.854287861381836,-0.105110771754112,
-0.594117907273489));
#55255=CARTESIAN_POINT('Ctrl Pts',(0.803110814976075,0.309627265129476,
-0.583683944671009));
#55256=CARTESIAN_POINT('Ctrl Pts',(0.562632999903826,0.651383244996612,
-0.573249982068529));
#55257=CARTESIAN_POINT('Ctrl Pts',(0.189537297769378,0.83960207074386,-0.562816019466047));
#55258=CARTESIAN_POINT('Ctrl Pts',(-0.228234127178966,0.829918795807126,
-0.552382056863567));
#55259=CARTESIAN_POINT('Ctrl Pts',(-0.592208622855237,0.624615859115824,
-0.541948094261086));
#55260=CARTESIAN_POINT('Ctrl Pts',(-0.816593979116471,0.272085092781327,
-0.531514131658605));
#55261=CARTESIAN_POINT('Ctrl Pts',(-0.848500458175958,-0.144578687635082,
-0.521080169056126));
#55262=CARTESIAN_POINT('Ctrl Pts',(-0.680407402985169,-0.527163912275939,
-0.510646206453644));
#55263=CARTESIAN_POINT('Ctrl Pts',(-0.351935926797396,-0.785491647232708,
-0.500212243851165));
#55264=CARTESIAN_POINT('Ctrl Pts',(0.0594901556810223,-0.858671616987626,
-0.489778281248683));
#55265=CARTESIAN_POINT('Ctrl Pts',(0.45689384923315,-0.729454614747216,
-0.479344318646203));
#55266=CARTESIAN_POINT('Ctrl Pts',(0.746603367528273,-0.42829830263327,
-0.468910356043722));
#55267=CARTESIAN_POINT('Ctrl Pts',(0.860331453713932,-0.0261880544059605,
-0.458476393441242));
#55268=CARTESIAN_POINT('Ctrl Pts',(0.771271328784714,0.382094964423429,
-0.448042430838761));
#55269=CARTESIAN_POINT('Ctrl Pts',(0.500415301388765,0.700314608286261,
-0.437608468236281));
#55270=CARTESIAN_POINT('Ctrl Pts',(0.111606683342926,0.853463515726458,
-0.427174505633799));
#55271=CARTESIAN_POINT('Ctrl Pts',(-0.303508679116197,0.80544304959721,
-0.41674054303132));
#55272=CARTESIAN_POINT('Ctrl Pts',(-0.647084192799489,0.567572085176711,
-0.406306580428838));
#55273=CARTESIAN_POINT('Ctrl Pts',(-0.838135879378581,0.195919044866881,
-0.395872617826358));
#55274=CARTESIAN_POINT('Ctrl Pts',(-0.831631060361417,-0.221913956041068,
-0.385438655223877));
#55275=CARTESIAN_POINT('Ctrl Pts',(-0.629102982738002,-0.587439751421957,
-0.375004692621397));
#55276=CARTESIAN_POINT('Ctrl Pts',(-0.278289418253274,-0.81450047522273,
-0.364570730018916));
#55277=CARTESIAN_POINT('Ctrl Pts',(0.138119578151266,-0.849575780352192,
-0.354136767416436));
#55278=CARTESIAN_POINT('Ctrl Pts',(0.521972491602115,-0.684398087719615,
-0.343702804813954));
#55279=CARTESIAN_POINT('Ctrl Pts',(0.782791582026743,-0.357901332117912,
-0.333268842211475));
#55280=CARTESIAN_POINT('Ctrl Pts',(0.859099337993372,0.0529561317558256,
-0.322834879608993));
#55281=CARTESIAN_POINT('Ctrl Pts',(0.732909304116489,0.45133133782035,-0.312400917006513));
#55282=CARTESIAN_POINT('Ctrl Pts',(0.433965657579441,0.74332350435601,-0.301966954404032));
#55283=CARTESIAN_POINT('Ctrl Pts',(0.0327322261453245,0.86010733435001,
-0.291532991801552));
#55284=CARTESIAN_POINT('Ctrl Pts',(-0.376216498791165,0.774155778332482,
-0.281099029199071));
#55285=CARTESIAN_POINT('Ctrl Pts',(-0.696487458167504,0.505728431782088,
-0.270665066596591));
#55286=CARTESIAN_POINT('Ctrl Pts',(-0.852589776780192,0.118096132321047,
-0.26023110399411));
#55287=CARTESIAN_POINT('Ctrl Pts',(-0.807728669522175,-0.297372520979868,
-0.249797141391629));
#55288=CARTESIAN_POINT('Ctrl Pts',(-0.572478323412175,-0.64274770454798,
-0.239363178789149));
#55289=CARTESIAN_POINT('Ctrl Pts',(-0.202289451911256,-0.836621155292499,
-0.228929216186668));
#55290=CARTESIAN_POINT('Ctrl Pts',(0.215580939060973,-0.833295246691126,
-0.218495253584188));
#55291=CARTESIAN_POINT('Ctrl Pts',(0.582636887836437,-0.633553595935407,
-0.208061290981707));
#55292=CARTESIAN_POINT('Ctrl Pts',(0.812359822146789,-0.284477837654277,
-0.197627328379227));
#55293=CARTESIAN_POINT('Ctrl Pts',(0.850601954996978,0.131652867513664,
-0.187193365776746));
#55294=CARTESIAN_POINT('Ctrl Pts',(0.688349122337913,0.51675009114103,-0.176759403174265));
#55295=CARTESIAN_POINT('Ctrl Pts',(0.363846105084824,0.780047728610944,
-0.166325440571784));
#55296=CARTESIAN_POINT('Ctrl Pts',(-0.0464192020363373,0.859474361780549,
-0.155891477969304));
#55297=CARTESIAN_POINT('Ctrl Pts',(-0.445742392858137,0.736327430271739,
-0.145457515366823));
#55298=CARTESIAN_POINT('Ctrl Pts',(-0.740001245121636,0.439596369442942,
-0.135023552764343));
#55299=CARTESIAN_POINT('Ctrl Pts',(-0.859832124525603,0.0392974457347477,
-0.124589590161862));
#55300=CARTESIAN_POINT('Ctrl Pts',(-0.776998977184778,-0.370364573784881,
-0.114155627559381));
#55301=CARTESIAN_POINT('Ctrl Pts',(-0.599661254481017,-0.585112006191819,
-0.107199652491061));
#55302=CARTESIAN_POINT('Ctrl Pts',(-0.490897892427236,-0.665357183556695,
-0.103721664956901));
#55303=CARTESIAN_POINT('Ctrl Pts',(0.82685,-1.18395083925468E-14,-1.12910983122651));
#55304=CARTESIAN_POINT('Ctrl Pts',(0.826850000000002,0.13516238059478,-1.12563184369235));
#55305=CARTESIAN_POINT('Ctrl Pts',(0.759329891769109,0.405358236621008,
-1.11867586862402));
#55306=CARTESIAN_POINT('Ctrl Pts',(0.478857042724253,0.715228435638399,
-1.10824190602155));
#55307=CARTESIAN_POINT('Ctrl Pts',(0.0855976953161874,0.85645769610236,
-1.09780794341906));
#55308=CARTESIAN_POINT('Ctrl Pts',(-0.327879002777259,0.795839066043269,
-1.08737398081658));
#55309=CARTESIAN_POINT('Ctrl Pts',(-0.664050756097952,0.547619885902207,
-1.0769400182141));
#55310=CARTESIAN_POINT('Ctrl Pts',(-0.84371006453472,0.170328568685808,
-1.06650605561162));
#55311=CARTESIAN_POINT('Ctrl Pts',(-0.824493606532929,-0.247114364257438,
-1.05607209300914));
#55312=CARTESIAN_POINT('Ctrl Pts',(-0.610938989097409,-0.606308301358728,
-1.04563813040666));
#55313=CARTESIAN_POINT('Ctrl Pts',(-0.253378917416567,-0.8225905970557,
-1.03520416780418));
#55314=CARTESIAN_POINT('Ctrl Pts',(0.163904238864593,-0.844980085711621,
-1.0247702052017));
#55315=CARTESIAN_POINT('Ctrl Pts',(0.542553985631643,-0.668200064499605,
-1.01433624259922));
#55316=CARTESIAN_POINT('Ctrl Pts',(0.793318474366497,-0.333918884843972,
-1.00390227999674));
#55317=CARTESIAN_POINT('Ctrl Pts',(0.857090434493622,0.0790700529203221,
-0.993468317394257));
#55318=CARTESIAN_POINT('Ctrl Pts',(0.718838074709771,0.473421467484893,
-0.983034354791779));
#55319=CARTESIAN_POINT('Ctrl Pts',(0.411148847508517,0.756182975740498,
-0.972600392189296));
#55320=CARTESIAN_POINT('Ctrl Pts',(0.00654795967899482,0.860705056353458,
-0.962166429586817));
#55321=CARTESIAN_POINT('Ctrl Pts',(-0.399596337540997,0.76235086003724,
-0.951732466984335));
#55322=CARTESIAN_POINT('Ctrl Pts',(-0.711552024815767,0.484303401711301,
-0.941298504381855));
#55323=CARTESIAN_POINT('Ctrl Pts',(-0.855788209334577,0.0921010778706362,
-0.930864541779374));
#55324=CARTESIAN_POINT('Ctrl Pts',(-0.798307068972087,-0.321810335264394,
-0.920430579176894));
#55325=CARTESIAN_POINT('Ctrl Pts',(-0.552657447613637,-0.659868027505257,
-0.909996616574414));
#55326=CARTESIAN_POINT('Ctrl Pts',(-0.176741270855791,-0.842388622486454,
-0.899562653971932));
#55327=CARTESIAN_POINT('Ctrl Pts',(0.240834484993158,-0.826350300415455,
-0.889128691369453));
#55328=CARTESIAN_POINT('Ctrl Pts',(0.601643288729277,-0.615533444462273,
-0.878694728766971));
#55329=CARTESIAN_POINT('Ctrl Pts',(0.820639113642215,-0.25962956939694,
-0.868260766164491));
#55330=CARTESIAN_POINT('Ctrl Pts',(0.846202585105403,0.157471435811019,
-0.857826803562011));
#55331=CARTESIAN_POINT('Ctrl Pts',(0.672308152609301,0.537454943296294,
-0.847392840959529));
#55332=CARTESIAN_POINT('Ctrl Pts',(0.33994436856243,0.79075526834847,-0.83695887835705));
#55333=CARTESIAN_POINT('Ctrl Pts',(-0.0725474987715683,0.857667143220317,
-0.826524915754568));
#55334=CARTESIAN_POINT('Ctrl Pts',(-0.467939238669323,0.722418810006908,
-0.816090953152088));
#55335=CARTESIAN_POINT('Ctrl Pts',(-0.753033301188211,0.416889572236419,
-0.805656990549607));
#55336=CARTESIAN_POINT('Ctrl Pts',(-0.86063033579018,0.0130955433541141,
-0.795223027947127));
#55337=CARTESIAN_POINT('Ctrl Pts',(-0.765368709962157,-0.393785228200411,
-0.784789065344645));
#55338=CARTESIAN_POINT('Ctrl Pts',(-0.489702484411022,-0.707847119722667,
-0.774355102742166));
#55339=CARTESIAN_POINT('Ctrl Pts',(-0.0986087798765727,-0.855062791068153,
-0.763921140139684));
#55340=CARTESIAN_POINT('Ctrl Pts',(0.315727941038427,-0.800732124611992,
-0.753487177537205));
#55341=CARTESIAN_POINT('Ctrl Pts',(0.655644618276346,-0.557661369168844,
-0.743053214934723));
#55342=CARTESIAN_POINT('Ctrl Pts',(0.841019695653654,-0.183144586763133,
-0.732619252332244));
#55343=CARTESIAN_POINT('Ctrl Pts',(0.828158524829477,0.23454109637815,-0.722185289729761));
#55344=CARTESIAN_POINT('Ctrl Pts',(0.620092604667449,0.596943238318974,
-0.711751327127283));
#55345=CARTESIAN_POINT('Ctrl Pts',(0.265865028456182,0.818640247472597,
-0.7013173645248));
#55346=CARTESIAN_POINT('Ctrl Pts',(-0.151029434204362,0.84737605473716,
-0.690883401922322));
#55347=CARTESIAN_POINT('Ctrl Pts',(-0.532324839483263,0.676377360211827,
-0.680449439319839));
#55348=CARTESIAN_POINT('Ctrl Pts',(-0.788146276020443,0.345950163655275,
-0.670015476717359));
#55349=CARTESIAN_POINT('Ctrl Pts',(-0.858194226395883,-0.0660207385506573,
-0.659581514114879));
#55350=CARTESIAN_POINT('Ctrl Pts',(-0.725957730226144,-0.46242993205772,
-0.649147551512397));
#55351=CARTESIAN_POINT('Ctrl Pts',(-0.42260617273665,-0.749840043544545,
-0.638713588909918));
#55352=CARTESIAN_POINT('Ctrl Pts',(-0.0196423676588402,-0.860505807958759,
-0.628279626307437));
#55353=CARTESIAN_POINT('Ctrl Pts',(0.387951328122605,-0.768342264323595,
-0.617845663704956));
#55354=CARTESIAN_POINT('Ctrl Pts',(0.704101248961261,-0.495073226249609,
-0.607411701102476));
#55355=CARTESIAN_POINT('Ctrl Pts',(0.854287886574333,-0.105110774853773,
-0.596977738499995));
#55356=CARTESIAN_POINT('Ctrl Pts',(0.803110838659391,0.309627274260221,
-0.586543775897515));
#55357=CARTESIAN_POINT('Ctrl Pts',(0.562633016495577,0.65138326420556,-0.576109813295034));
#55358=CARTESIAN_POINT('Ctrl Pts',(0.189537303358733,0.839602095503282,
-0.565675850692553));
#55359=CARTESIAN_POINT('Ctrl Pts',(-0.228234133909469,0.829918820280995,
-0.555241888090073));
#55360=CARTESIAN_POINT('Ctrl Pts',(-0.592208640319157,0.624615877535415,
-0.544807925487591));
#55361=CARTESIAN_POINT('Ctrl Pts',(-0.816594003197397,0.272085100804974,
-0.534373962885112));
#55362=CARTESIAN_POINT('Ctrl Pts',(-0.848500483197789,-0.144578691898632,
-0.523940000282631));
#55363=CARTESIAN_POINT('Ctrl Pts',(-0.680407423050025,-0.527163927821724,
-0.51350603768015));
#55364=CARTESIAN_POINT('Ctrl Pts',(-0.351935937175801,-0.785491670396442,
-0.50307207507767));
#55365=CARTESIAN_POINT('Ctrl Pts',(0.0594901574353561,-0.858671642309399,
-0.492638112475189));
#55366=CARTESIAN_POINT('Ctrl Pts',(0.456893862706708,-0.729454636258447,
-0.482204149872708));
#55367=CARTESIAN_POINT('Ctrl Pts',(0.746603389545214,-0.428298315263561,
-0.471770187270228));
#55368=CARTESIAN_POINT('Ctrl Pts',(0.860331479084652,-0.0261880551782322,
-0.461336224667747));
#55369=CARTESIAN_POINT('Ctrl Pts',(0.771271351529099,0.382094975691208,
-0.450902262065267));
#55370=CARTESIAN_POINT('Ctrl Pts',(0.500415316145748,0.700314628938169,
-0.440468299462786));
#55371=CARTESIAN_POINT('Ctrl Pts',(0.111606686634148,0.853463540894647,
-0.430034336860305));
#55372=CARTESIAN_POINT('Ctrl Pts',(-0.303508688066508,0.805443073349301,
-0.419600374257825));
#55373=CARTESIAN_POINT('Ctrl Pts',(-0.64708421188166,0.567572101914111,
-0.409166411655344));
#55374=CARTESIAN_POINT('Ctrl Pts',(-0.838135904094767,0.195919050644432,
-0.398732449052864));
#55375=CARTESIAN_POINT('Ctrl Pts',(-0.831631084885775,-0.221913962585196,
-0.388298486450383));
#55376=CARTESIAN_POINT('Ctrl Pts',(-0.629103001289925,-0.587439768745239,
-0.377864523847903));
#55377=CARTESIAN_POINT('Ctrl Pts',(-0.278289426459866,-0.814500499241933,
-0.367430561245421));
#55378=CARTESIAN_POINT('Ctrl Pts',(0.138119582224307,-0.849575805405707,
-0.356996598642941));
#55379=CARTESIAN_POINT('Ctrl Pts',(0.521972506994872,-0.684398107902206,
-0.346562636040461));
#55380=CARTESIAN_POINT('Ctrl Pts',(0.78279160511073,-0.35790134267213,-0.336128673437979));
#55381=CARTESIAN_POINT('Ctrl Pts',(0.859099363328004,0.0529561333172702,
-0.3256947108355));
#55382=CARTESIAN_POINT('Ctrl Pts',(0.732909325729115,0.451331351130274,
-0.315260748233019));
#55383=CARTESIAN_POINT('Ctrl Pts',(0.433965670377806,0.743323526275441,
-0.304826785630538));
#55384=CARTESIAN_POINT('Ctrl Pts',(0.032732227108719,0.86010735971567,-0.294392823028057));
#55385=CARTESIAN_POINT('Ctrl Pts',(-0.376216509881933,0.774155801158885,
-0.283958860425577));
#55386=CARTESIAN_POINT('Ctrl Pts',(-0.696487478713739,0.505728446701731,
-0.273524897823096));
#55387=CARTESIAN_POINT('Ctrl Pts',(-0.85258980190849,0.118096135791892,
-0.263090935220616));
#55388=CARTESIAN_POINT('Ctrl Pts',(-0.807728693369422,-0.297372529726142,
-0.252656972618135));
#55389=CARTESIAN_POINT('Ctrl Pts',(-0.57247834023972,-0.642747723547633,
-0.242223010015654));
#55390=CARTESIAN_POINT('Ctrl Pts',(-0.202289457983834,-0.836621179874879,
-0.231789047413174));
#55391=CARTESIAN_POINT('Ctrl Pts',(0.215580945628928,-0.833295271439718,
-0.221355084810693));
#55392=CARTESIAN_POINT('Ctrl Pts',(0.582636904604284,-0.633553614274387,
-0.210921122208213));
#55393=CARTESIAN_POINT('Ctrl Pts',(0.812359846915988,-0.2844778467197,-0.200487159605732));
#55394=CARTESIAN_POINT('Ctrl Pts',(0.850601978482956,0.131652872725018,
-0.190053197003252));
#55395=CARTESIAN_POINT('Ctrl Pts',(0.688349145776723,0.516750103768243,
-0.179619234400771));
#55396=CARTESIAN_POINT('Ctrl Pts',(0.363846109644695,0.780047756745801,
-0.16918527179829));
#55397=CARTESIAN_POINT('Ctrl Pts',(-0.0464191912805547,0.85947437704138,
-0.15875130919581));
#55398=CARTESIAN_POINT('Ctrl Pts',(-0.445742429839068,0.736327471811283,
-0.148317346593329));
#55399=CARTESIAN_POINT('Ctrl Pts',(-0.740001219981211,0.439596343345489,
-0.137883383990848));
#55400=CARTESIAN_POINT('Ctrl Pts',(-0.859832243554816,0.0392975248057425,
-0.127449421388368));
#55401=CARTESIAN_POINT('Ctrl Pts',(-0.776998800479074,-0.370364750731842,
-0.117015458785887));
#55402=CARTESIAN_POINT('Ctrl Pts',(-0.599661587021621,-0.58511176084468,
-0.110059483717567));
#55403=CARTESIAN_POINT('Ctrl Pts',(-0.490897892427236,-0.665357183556695,
-0.106581496183407));
#55404=CARTESIAN_POINT('Ctrl Pts',(0.825266255435535,-1.18168310543808E-14,
-1.13578682154469));
#55405=CARTESIAN_POINT('Ctrl Pts',(0.825266255435537,0.13490237313339,-1.13230883401053));
#55406=CARTESIAN_POINT('Ctrl Pts',(0.757875373501364,0.404582484316022,
-1.12535285894221));
#55407=CARTESIAN_POINT('Ctrl Pts',(0.477939823171883,0.7138581043365,-1.11491889633972));
#55408=CARTESIAN_POINT('Ctrl Pts',(0.0854337254619297,0.854817337751033,
-1.10448493373724));
#55409=CARTESIAN_POINT('Ctrl Pts',(-0.327250953856651,0.794314572438201,
-1.09405097113476));
#55410=CARTESIAN_POINT('Ctrl Pts',(-0.662778785930788,0.54657097627622,
-1.08361700853228));
#55411=CARTESIAN_POINT('Ctrl Pts',(-0.842093957705063,0.170002286889046,
-1.0731830459298));
#55412=CARTESIAN_POINT('Ctrl Pts',(-0.822914310253027,-0.246641011830828,
-1.06274908332732));
#55413=CARTESIAN_POINT('Ctrl Pts',(-0.609768750387392,-0.605146938555674,
-1.05231512072484));
#55414=CARTESIAN_POINT('Ctrl Pts',(-0.252893576591479,-0.821014942444095,
-1.04188115812236));
#55415=CARTESIAN_POINT('Ctrl Pts',(0.163590284471105,-0.843361548903805,
-1.03144719551988));
#55416=CARTESIAN_POINT('Ctrl Pts',(0.541514736972462,-0.666920143216012,
-1.0210132329174));
#55417=CARTESIAN_POINT('Ctrl Pts',(0.791798892653782,-0.333279271931917,
-1.01057927031492));
#55418=CARTESIAN_POINT('Ctrl Pts',(0.855448699150102,0.0789185963993196,
-1.00014530771244));
#55419=CARTESIAN_POINT('Ctrl Pts',(0.717461158327158,0.472514640384086,
-0.989711345109958));
#55420=CARTESIAN_POINT('Ctrl Pts',(0.410361302151426,0.754734526176116,
-0.979277382507477));
#55421=CARTESIAN_POINT('Ctrl Pts',(0.00653541722715152,0.859056397277897,
-0.968843419904996));
#55422=CARTESIAN_POINT('Ctrl Pts',(-0.398830920732009,0.760890596007683,
-0.958409457302515));
#55423=CARTESIAN_POINT('Ctrl Pts',(-0.710189064673792,0.483375730628087,
-0.947975494700036));
#55424=CARTESIAN_POINT('Ctrl Pts',(-0.854148968382191,0.0919246605583529,
-0.937541532097554));
#55425=CARTESIAN_POINT('Ctrl Pts',(-0.796777931708914,-0.321193915601999,
-0.927107569495075));
#55426=CARTESIAN_POINT('Ctrl Pts',(-0.551598846068358,-0.658604066769501,
-0.916673606892592));
#55427=CARTESIAN_POINT('Ctrl Pts',(-0.176402727363301,-0.840775048108436,
-0.906239644290114));
#55428=CARTESIAN_POINT('Ctrl Pts',(0.240373172548911,-0.824767447042349,
-0.895805681687632));
#55429=CARTESIAN_POINT('Ctrl Pts',(0.600490856028094,-0.61435440551462,
-0.885371719085151));
#55430=CARTESIAN_POINT('Ctrl Pts',(0.819067199905029,-0.259132255437641,
-0.874937756482671));
#55431=CARTESIAN_POINT('Ctrl Pts',(0.844581705176757,0.157169803206534,
-0.86450379388019));
#55432=CARTESIAN_POINT('Ctrl Pts',(0.671020363125302,0.53642546176851,-0.854069831277709));
#55433=CARTESIAN_POINT('Ctrl Pts',(0.339293213610226,0.789240596370972,
-0.84363586867523));
#55434=CARTESIAN_POINT('Ctrl Pts',(-0.0724085358486207,0.856024303216785,
-0.833201906072748));
#55435=CARTESIAN_POINT('Ctrl Pts',(-0.467042912738468,0.721035034809539,
-0.822767943470269));
#55436=CARTESIAN_POINT('Ctrl Pts',(-0.751590884697192,0.416091030667303,
-0.812333980867787));
#55437=CARTESIAN_POINT('Ctrl Pts',(-0.858981819865244,0.013070459167713,
-0.801900018265307));
#55438=CARTESIAN_POINT('Ctrl Pts',(-0.763902665303551,-0.393030942425558,
-0.791466055662826));
#55439=CARTESIAN_POINT('Ctrl Pts',(-0.488764471526209,-0.706491256234298,
-0.781032093060345));
#55440=CARTESIAN_POINT('Ctrl Pts',(-0.0984198972202164,-0.853424939636153,
-0.770598130457865));
#55441=CARTESIAN_POINT('Ctrl Pts',(0.315123172048648,-0.799198342215375,
-0.760164167855384));
#55442=CARTESIAN_POINT('Ctrl Pts',(0.654388747376403,-0.556593182736684,
-0.749730205252904));
#55443=CARTESIAN_POINT('Ctrl Pts',(0.839408743420374,-0.182793777878889,
-0.739296242650423));
#55444=CARTESIAN_POINT('Ctrl Pts',(0.826572207847868,0.234091838762711,
-0.728862280047942));
#55445=CARTESIAN_POINT('Ctrl Pts',(0.618904832762115,0.595799808447021,
-0.718428317445462));
#55446=CARTESIAN_POINT('Ctrl Pts',(0.265355770630764,0.817072162513667,
-0.70799435484298));
#55447=CARTESIAN_POINT('Ctrl Pts',(-0.150740141093178,0.845752927056724,
-0.697560392240501));
#55448=CARTESIAN_POINT('Ctrl Pts',(-0.531305184541259,0.675081776262244,
-0.687126429638019));
#55449=CARTESIAN_POINT('Ctrl Pts',(-0.786636601502631,0.345287504752488,
-0.67669246703554));
#55450=CARTESIAN_POINT('Ctrl Pts',(-0.856550376777681,-0.0658942774739896,
-0.666258504433059));
#55451=CARTESIAN_POINT('Ctrl Pts',(-0.724567176315435,-0.461544159066156,
-0.655824541830578));
#55452=CARTESIAN_POINT('Ctrl Pts',(-0.421796681161974,-0.74840374365883,
-0.645390579228098));
#55453=CARTESIAN_POINT('Ctrl Pts',(-0.0196047431939077,-0.858857530563777,
-0.634956616625617));
#55454=CARTESIAN_POINT('Ctrl Pts',(0.387208217037725,-0.766870523895835,
-0.624522654023137));
#55455=CARTESIAN_POINT('Ctrl Pts',(0.702752560594827,-0.49412492584287,
-0.614088691420656));
#55456=CARTESIAN_POINT('Ctrl Pts',(0.85265151945255,-0.104909437788342,
-0.603654728818175));
#55457=CARTESIAN_POINT('Ctrl Pts',(0.801572499895392,0.309034190945369,
-0.593220766215695));
#55458=CARTESIAN_POINT('Ctrl Pts',(0.561555306997066,0.650135555822967,
-0.582786803613214));
#55459=CARTESIAN_POINT('Ctrl Pts',(0.189174249385427,0.837993858647704,
-0.572352841010733));
#55460=CARTESIAN_POINT('Ctrl Pts',(-0.227796957123204,0.828329131497389,
-0.561918878408252));
#55461=CARTESIAN_POINT('Ctrl Pts',(-0.591074279451486,0.623419441413815,
-0.551484915805773));
#55462=CARTESIAN_POINT('Ctrl Pts',(-0.815029837768297,0.271563928586238,
-0.541050953203291));
#55463=CARTESIAN_POINT('Ctrl Pts',(-0.846875201702706,-0.144301755023309,
-0.530616990600811));
#55464=CARTESIAN_POINT('Ctrl Pts',(-0.679104119615673,-0.52615415847718,
-0.52018302799833));
#55465=CARTESIAN_POINT('Ctrl Pts',(-0.351261812673254,-0.783987080709438,
-0.50974906539585));
#55466=CARTESIAN_POINT('Ctrl Pts',(0.0593762055237972,-0.857026878212933,
-0.499315102793369));
#55467=CARTESIAN_POINT('Ctrl Pts',(0.456018693917792,-0.728057384111524,
-0.488881140190888));
#55468=CARTESIAN_POINT('Ctrl Pts',(0.745173289389441,-0.427477920531964,
-0.478447177588408));
#55469=CARTESIAN_POINT('Ctrl Pts',(0.858683535612276,-0.0261378926122512,
-0.468013214985927));
#55470=CARTESIAN_POINT('Ctrl Pts',(0.769794000507914,0.381363082303222,
-0.457579252383447));
#55471=CARTESIAN_POINT('Ctrl Pts',(0.499456783099164,0.698973193747868,
-0.447145289780966));
#55472=CARTESIAN_POINT('Ctrl Pts',(0.111392906811854,0.851828752786435,
-0.436711327178485));
#55473=CARTESIAN_POINT('Ctrl Pts',(-0.302927324750776,0.803900267247972,
-0.426277364576005));
#55474=CARTESIAN_POINT('Ctrl Pts',(-0.645844738226482,0.566484931720774,
-0.415843401973524));
#55475=CARTESIAN_POINT('Ctrl Pts',(-0.836530475692227,0.195543772593499,
-0.405409439371044));
#55476=CARTESIAN_POINT('Ctrl Pts',(-0.830038116302071,-0.221488891929327,
-0.394975476768563));
#55477=CARTESIAN_POINT('Ctrl Pts',(-0.627897970194759,-0.586314542532045,
-0.384541514166082));
#55478=CARTESIAN_POINT('Ctrl Pts',(-0.277756370010257,-0.812940343867364,
-0.374107551563602));
#55479=CARTESIAN_POINT('Ctrl Pts',(0.137855017612419,-0.84794846415785,
-0.363673588961121));
#55480=CARTESIAN_POINT('Ctrl Pts',(0.52097268168716,-0.683087160410494,
-0.353239626358641));
#55481=CARTESIAN_POINT('Ctrl Pts',(0.781292187331718,-0.357215791584545,
-0.34280566375616));
#55482=CARTESIAN_POINT('Ctrl Pts',(0.85745377994194,0.0528546971663574,
-0.33237170115368));
#55483=CARTESIAN_POINT('Ctrl Pts',(0.731505456212053,0.450466837192345,
-0.321937738551198));
#55484=CARTESIAN_POINT('Ctrl Pts',(0.433134419966394,0.741899708618021,
-0.311503775948719));
#55485=CARTESIAN_POINT('Ctrl Pts',(0.0326695293497987,0.85845984553416,
-0.301069813346238));
#55486=CARTESIAN_POINT('Ctrl Pts',(-0.375495876558362,0.772672925054669,
-0.290635850743757));
#55487=CARTESIAN_POINT('Ctrl Pts',(-0.695153374314712,0.504759736470019,
-0.280201888141276));
#55488=CARTESIAN_POINT('Ctrl Pts',(-0.850956687463709,0.117869925623513,
-0.269767925538796));
#55489=CARTESIAN_POINT('Ctrl Pts',(-0.806181509144908,-0.296802920130996,
-0.259333962936315));
#55490=CARTESIAN_POINT('Ctrl Pts',(-0.571381772416895,-0.641516556204879,
-0.248900000333835));
#55491=CARTESIAN_POINT('Ctrl Pts',(-0.201901977286717,-0.83501865312994,
-0.238466037731354));
#55492=CARTESIAN_POINT('Ctrl Pts',(0.215168005139208,-0.831699114674313,
-0.228032075128874));
#55493=CARTESIAN_POINT('Ctrl Pts',(0.581520879277018,-0.632340059072367,
-0.217598112526393));
#55494=CARTESIAN_POINT('Ctrl Pts',(0.810803789707571,-0.283932934675695,
-0.207164149923912));
#55495=CARTESIAN_POINT('Ctrl Pts',(0.84897267594911,0.131400691338038,-0.196730187321431));
#55496=CARTESIAN_POINT('Ctrl Pts',(0.687030621675953,0.515760288909202,
-0.186296224718951));
#55497=CARTESIAN_POINT('Ctrl Pts',(0.363149188196698,0.778553580855524,
-0.175862262116471));
#55498=CARTESIAN_POINT('Ctrl Pts',(-0.0463303092822942,0.857828102611029,
-0.16542829951399));
#55499=CARTESIAN_POINT('Ctrl Pts',(-0.444888556851283,0.734917001280111,
-0.154994336911509));
#55500=CARTESIAN_POINT('Ctrl Pts',(-0.738583893176423,0.438754413204503,
-0.144560374309029));
#55501=CARTESIAN_POINT('Ctrl Pts',(-0.858185002917794,0.0392220405825323,
-0.134126411706548));
#55502=CARTESIAN_POINT('Ctrl Pts',(-0.77551101875214,-0.369654877107249,
-0.123692449104067));
#55503=CARTESIAN_POINT('Ctrl Pts',(-0.598512098358559,-0.583991704355505,
-0.116736474035747));
#55504=CARTESIAN_POINT('Ctrl Pts',(-0.489957628934657,-0.664082761566146,
-0.113258486501587));
#55505=CARTESIAN_POINT('Ctrl Pts',(0.82035433218061,-1.17464981565151E-14,
-1.14076763757253));
#55506=CARTESIAN_POINT('Ctrl Pts',(0.820354332180612,0.134101768298544,
-1.13728965003837));
#55507=CARTESIAN_POINT('Ctrl Pts',(0.753364766519594,0.402173049067142,
-1.13033367497005));
#55508=CARTESIAN_POINT('Ctrl Pts',(0.475095200548904,0.709610076749487,
-1.11989971236757));
#55509=CARTESIAN_POINT('Ctrl Pts',(0.0849252644561764,0.849729327752102,
-1.10946574976509));
#55510=CARTESIAN_POINT('Ctrl Pts',(-0.325303245075429,0.789587177339037,
-1.09903178716261));
#55511=CARTESIAN_POINT('Ctrl Pts',(-0.658834080958521,0.543317828833928,
-1.08859782456013));
#55512=CARTESIAN_POINT('Ctrl Pts',(-0.837082019765518,0.168990519247415,
-1.07816386195765));
#55513=CARTESIAN_POINT('Ctrl Pts',(-0.818016521001053,-0.245173086817304,
-1.06772989935517));
#55514=CARTESIAN_POINT('Ctrl Pts',(-0.606139554222435,-0.601545237955094,
-1.05729593675269));
#55515=CARTESIAN_POINT('Ctrl Pts',(-0.251388414543869,-0.816128465044896,
-1.04686197415021));
#55516=CARTESIAN_POINT('Ctrl Pts',(0.162616634294616,-0.838342060921673,
-1.03642801154773));
#55517=CARTESIAN_POINT('Ctrl Pts',(0.538291771678315,-0.662950796574508,
-1.02599404894525));
#55518=CARTESIAN_POINT('Ctrl Pts',(0.787086296167862,-0.331295673135843,
-1.01556008634276));
#55519=CARTESIAN_POINT('Ctrl Pts',(0.850357274403785,0.0784488915092764,
-1.00512612374029));
#55520=CARTESIAN_POINT('Ctrl Pts',(0.713191002178242,0.469702347171158,
-0.994692161137803));
#55521=CARTESIAN_POINT('Ctrl Pts',(0.407918930452038,0.750242527821308,
-0.984258198535323));
#55522=CARTESIAN_POINT('Ctrl Pts',(0.00649651999369233,0.853943500409919,
-0.973824235932843));
#55523=CARTESIAN_POINT('Ctrl Pts',(-0.396457175080158,0.756361958283298,
-0.963390273330362));
#55524=CARTESIAN_POINT('Ctrl Pts',(-0.705962190288657,0.480498794630974,
-0.952956310727882));
#55525=CARTESIAN_POINT('Ctrl Pts',(-0.849065279296998,0.0913775470960521,
-0.9425223481254));
#55526=CARTESIAN_POINT('Ctrl Pts',(-0.792035701226651,-0.319282246717183,
-0.932088385522921));
#55527=CARTESIAN_POINT('Ctrl Pts',(-0.548315862494261,-0.654684213877508,
-0.92165442292044));
#55528=CARTESIAN_POINT('Ctrl Pts',(-0.175352820786375,-0.835770957377393,
-0.911220460317959));
#55529=CARTESIAN_POINT('Ctrl Pts',(0.238942529278504,-0.819858629701546,
-0.900786497715479));
#55530=CARTESIAN_POINT('Ctrl Pts',(0.596916878978049,-0.610697915954462,
-0.890352535112997));
#55531=CARTESIAN_POINT('Ctrl Pts',(0.814192309062805,-0.257589962620876,
-0.879918572510518));
#55532=CARTESIAN_POINT('Ctrl Pts',(0.83955495813993,0.156234366365253,-0.869484609908036));
#55533=CARTESIAN_POINT('Ctrl Pts',(0.667026611423942,0.533232786525937,
-0.859050647305557));
#55534=CARTESIAN_POINT('Ctrl Pts',(0.33727382206329,0.784543226294379,-0.848616684703075));
#55535=CARTESIAN_POINT('Ctrl Pts',(-0.0719775776704039,0.850929452590404,
-0.838182722100595));
#55536=CARTESIAN_POINT('Ctrl Pts',(-0.464263185728888,0.716743607819756,
-0.827748759498115));
#55537=CARTESIAN_POINT('Ctrl Pts',(-0.747117596643002,0.413614556996802,
-0.817314796895633));
#55538=CARTESIAN_POINT('Ctrl Pts',(-0.853869366811588,0.012992666940522,
-0.806880834293153));
#55539=CARTESIAN_POINT('Ctrl Pts',(-0.759356100494369,-0.390691716850214,
-0.796446871690672));
#55540=CARTESIAN_POINT('Ctrl Pts',(-0.485855463026629,-0.70228639031422,
-0.786012909088192));
#55541=CARTESIAN_POINT('Ctrl Pts',(-0.0978341256794837,-0.848345559796202,
-0.775578946485711));
#55542=CARTESIAN_POINT('Ctrl Pts',(0.313247634771886,-0.794441706032112,
-0.765144983883231));
#55543=CARTESIAN_POINT('Ctrl Pts',(0.650493983049112,-0.553280474072871,
-0.754711021280749));
#55544=CARTESIAN_POINT('Ctrl Pts',(0.834412784606905,-0.181705833307428,
-0.74427705867827));
#55545=CARTESIAN_POINT('Ctrl Pts',(0.821652649004654,0.232698580479193,
-0.733843096075788));
#55546=CARTESIAN_POINT('Ctrl Pts',(0.615221260154405,0.592253751383159,
-0.723409133473309));
#55547=CARTESIAN_POINT('Ctrl Pts',(0.263776436949314,0.812209145653827,
-0.712975170870827));
#55548=CARTESIAN_POINT('Ctrl Pts',(-0.149842972053255,0.84071920918916,
-0.702541208268347));
#55549=CARTESIAN_POINT('Ctrl Pts',(-0.528142983956435,0.671063852007384,
-0.692107245665866));
#55550=CARTESIAN_POINT('Ctrl Pts',(-0.781954729776754,0.34323243662737,
-0.681673283063386));
#55551=CARTESIAN_POINT('Ctrl Pts',(-0.851452395088088,-0.0655020905937791,
-0.671239320460906));
#55552=CARTESIAN_POINT('Ctrl Pts',(-0.720254726869515,-0.458797159315003,
-0.660805357858424));
#55553=CARTESIAN_POINT('Ctrl Pts',(-0.419286248832957,-0.743949424701024,
-0.650371395255944));
#55554=CARTESIAN_POINT('Ctrl Pts',(-0.0194880604808514,-0.85374581725013,
-0.639937432653463));
#55555=CARTESIAN_POINT('Ctrl Pts',(0.384903646922486,-0.76230629510661,
-0.629503470050983));
#55556=CARTESIAN_POINT('Ctrl Pts',(0.698569946491375,-0.491184013209342,
-0.619069507448502));
#55557=CARTESIAN_POINT('Ctrl Pts',(0.847576742823385,-0.104285042064039,
-0.608635544846021));
#55558=CARTESIAN_POINT('Ctrl Pts',(0.796801733297026,0.307194893818649,
-0.598201582243541));
#55559=CARTESIAN_POINT('Ctrl Pts',(0.55821306496393,0.646266105468152,-0.58776761964106));
#55560=CARTESIAN_POINT('Ctrl Pts',(0.188048329783199,0.833006320887871,
-0.577333657038579));
#55561=CARTESIAN_POINT('Ctrl Pts',(-0.226441164460163,0.823399115867464,
-0.566899694436099));
#55562=CARTESIAN_POINT('Ctrl Pts',(-0.587556347598874,0.619708998941978,
-0.556465731833618));
#55563=CARTESIAN_POINT('Ctrl Pts',(-0.810178976333799,0.269947645442805,
-0.546031769231138));
#55564=CARTESIAN_POINT('Ctrl Pts',(-0.841834804326554,-0.143442905707695,
-0.535597806628657));
#55565=CARTESIAN_POINT('Ctrl Pts',(-0.675062255341266,-0.52302261555975,
-0.525163844026177));
#55566=CARTESIAN_POINT('Ctrl Pts',(-0.349171186905277,-0.779320978293641,
-0.514729881423696));
#55567=CARTESIAN_POINT('Ctrl Pts',(0.0590228126390766,-0.851926060501479,
-0.504295918821215));
#55568=CARTESIAN_POINT('Ctrl Pts',(0.453304580405343,-0.723724161788819,
-0.493861956218735));
#55569=CARTESIAN_POINT('Ctrl Pts',(0.740738197317948,-0.424933674833566,
-0.483427993616254));
#55570=CARTESIAN_POINT('Ctrl Pts',(0.853572857874703,-0.0259823261662435,
-0.472994031013774));
#55571=CARTESIAN_POINT('Ctrl Pts',(0.765212371889512,0.379093301023127,
-0.462560068411293));
#55572=CARTESIAN_POINT('Ctrl Pts',(0.496484136534507,0.694813073526278,
-0.452126105808813));
#55573=CARTESIAN_POINT('Ctrl Pts',(0.110729923040354,0.846758873066444,
-0.441692143206331));
#55574=CARTESIAN_POINT('Ctrl Pts',(-0.30112437422186,0.799115646338569,
-0.431258180603851));
#55575=CARTESIAN_POINT('Ctrl Pts',(-0.642000825785288,0.56311334974773,
-0.420824218001371));
#55576=CARTESIAN_POINT('Ctrl Pts',(-0.831551647635553,0.194379943122152,
-0.41039025539889));
#55577=CARTESIAN_POINT('Ctrl Pts',(-0.825097929205881,-0.220170643352128,
-0.39995629279641));
#55578=CARTESIAN_POINT('Ctrl Pts',(-0.624160872597549,-0.582824939487973,
-0.389522330193928));
#55579=CARTESIAN_POINT('Ctrl Pts',(-0.276103230945762,-0.808101918597746,
-0.379088367591449));
#55580=CARTESIAN_POINT('Ctrl Pts',(0.137034537726103,-0.842901678981725,
-0.368654404988967));
#55581=CARTESIAN_POINT('Ctrl Pts',(0.517871977672874,-0.679021590036204,
-0.358220442386487));
#55582=CARTESIAN_POINT('Ctrl Pts',(0.776642124272,-0.355089729166497,-0.347786479784006));
#55583=CARTESIAN_POINT('Ctrl Pts',(0.852350421415522,0.0525401187286473,
-0.337352517181526));
#55584=CARTESIAN_POINT('Ctrl Pts',(0.72715171179137,0.447785766997171,-0.326918554579045));
#55585=CARTESIAN_POINT('Ctrl Pts',(0.430556508150087,0.737484100106967,
-0.316484591976564));
#55586=CARTESIAN_POINT('Ctrl Pts',(0.0324750881634825,0.853350499154804,
-0.306050629374084));
#55587=CARTESIAN_POINT('Ctrl Pts',(-0.373261015454179,0.768074161753147,
-0.295616666771603));
#55588=CARTESIAN_POINT('Ctrl Pts',(-0.691015988779464,0.501755528036826,
-0.285182704169123));
#55589=CARTESIAN_POINT('Ctrl Pts',(-0.8458919979872,0.117168392128854,-0.274748741566642));
#55590=CARTESIAN_POINT('Ctrl Pts',(-0.801383310988863,-0.295036420454541,
-0.264314778964161));
#55591=CARTESIAN_POINT('Ctrl Pts',(-0.567981045319887,-0.637698404316488,
-0.253880816361681));
#55592=CARTESIAN_POINT('Ctrl Pts',(-0.200700305913994,-0.830048822576,-0.2434468537592));
#55593=CARTESIAN_POINT('Ctrl Pts',(0.213887378143152,-0.826749042700625,
-0.23301289115672));
#55594=CARTESIAN_POINT('Ctrl Pts',(0.578059804635804,-0.628576521295636,
-0.222578928554239));
#55595=CARTESIAN_POINT('Ctrl Pts',(0.805978085266888,-0.282243037988429,
-0.212144965951759));
#55596=CARTESIAN_POINT('Ctrl Pts',(0.843919785925286,0.130618633522338,
-0.201711003349278));
#55597=CARTESIAN_POINT('Ctrl Pts',(0.68294159842625,0.512690593115567,-0.191277040746797));
#55598=CARTESIAN_POINT('Ctrl Pts',(0.36098777693341,0.773919846182344,-0.180843078144317));
#55599=CARTESIAN_POINT('Ctrl Pts',(-0.0460544942459941,0.852722459491375,
-0.170409115541836));
#55600=CARTESIAN_POINT('Ctrl Pts',(-0.442240821285006,0.730543063661545,
-0.159975152939355));
#55601=CARTESIAN_POINT('Ctrl Pts',(-0.734187755498606,0.436142832866609,
-0.149541190336875));
#55602=CARTESIAN_POINT('Ctrl Pts',(-0.853077819122259,0.0389890385957994,
-0.139107227734394));
#55603=CARTESIAN_POINT('Ctrl Pts',(-0.770894241208358,-0.367455713931453,
-0.128673265131913));
#55604=CARTESIAN_POINT('Ctrl Pts',(-0.594951669076752,-0.580514449476566,
-0.121717290063593));
#55605=CARTESIAN_POINT('Ctrl Pts',(-0.487041437638041,-0.660130190455614,
-0.118239302529433));
#55606=CARTESIAN_POINT('Ctrl Pts',(0.816972063808647,-1.16980680969206E-14,
-1.1425283350431));
#55607=CARTESIAN_POINT('Ctrl Pts',(0.816972063808649,0.133547259366542,
-1.13905034750894));
#55608=CARTESIAN_POINT('Ctrl Pts',(0.750258545288667,0.400515882139589,
-1.13209437244062));
#55609=CARTESIAN_POINT('Ctrl Pts',(0.473136385937643,0.706683841755145,
-1.12166040983814));
#55610=CARTESIAN_POINT('Ctrl Pts',(0.0845750992767583,0.84622608784569,
-1.11122644723566));
#55611=CARTESIAN_POINT('Ctrl Pts',(-0.323961995775528,0.786331547179381,
-1.10079248463318));
#55612=CARTESIAN_POINT('Ctrl Pts',(-0.656117677249225,0.541077762637857,
-1.0903585220307));
#55613=CARTESIAN_POINT('Ctrl Pts',(-0.833630685095572,0.168293731192079,
-1.07992455942822));
#55614=CARTESIAN_POINT('Ctrl Pts',(-0.814643797129344,-0.244162209445375,
-1.06949059682573));
#55615=CARTESIAN_POINT('Ctrl Pts',(-0.603640408739925,-0.599065043663486,
-1.05905663422325));
#55616=CARTESIAN_POINT('Ctrl Pts',(-0.250351927233731,-0.812763520669612,
-1.04862267162077));
#55617=CARTESIAN_POINT('Ctrl Pts',(0.161946157548475,-0.834885534961222,
-1.03818870901829));
#55618=CARTESIAN_POINT('Ctrl Pts',(0.536072366553588,-0.660217414778485,
-1.02775474641581));
#55619=CARTESIAN_POINT('Ctrl Pts',(0.783841098330598,-0.32992972433277,
-1.01732078381333));
#55620=CARTESIAN_POINT('Ctrl Pts',(0.846851206973998,0.0781254429130661,
-1.00688682121085));
#55621=CARTESIAN_POINT('Ctrl Pts',(0.710250478470448,0.467765739743972,
-0.996452858608371));
#55622=CARTESIAN_POINT('Ctrl Pts',(0.406237059412565,0.747149238803466,
-0.98601889600589));
#55623=CARTESIAN_POINT('Ctrl Pts',(0.00646973450489691,0.850422646762807,
-0.97558493340341));
#55624=CARTESIAN_POINT('Ctrl Pts',(-0.394822561461409,0.753243438481209,
-0.965150970800928));
#55625=CARTESIAN_POINT('Ctrl Pts',(-0.703051471340727,0.478517673019027,
-0.954717008198449));
#55626=CARTESIAN_POINT('Ctrl Pts',(-0.845564538846854,0.0910007927061417,
-0.944283045595967));
#55627=CARTESIAN_POINT('Ctrl Pts',(-0.78877009670225,-0.317965829356397,
-0.933849082993488));
#55628=CARTESIAN_POINT('Ctrl Pts',(-0.546055127582371,-0.65198491670129,
-0.923415120391006));
#55629=CARTESIAN_POINT('Ctrl Pts',(-0.174629831956398,-0.83232503011057,
-0.912981157788526));
#55630=CARTESIAN_POINT('Ctrl Pts',(0.237957356762347,-0.816478309791074,
-0.902547195186046));
#55631=CARTESIAN_POINT('Ctrl Pts',(0.59445575953915,-0.608179976581176,
-0.892113232583564));
#55632=CARTESIAN_POINT('Ctrl Pts',(0.810835351688311,-0.256527905763967,
-0.881679269981085));
#55633=CARTESIAN_POINT('Ctrl Pts',(0.836093429239884,0.15559020392044,-0.871245307378603));
#55634=CARTESIAN_POINT('Ctrl Pts',(0.664276425899862,0.531034239923243,
-0.860811344776123));
#55635=CARTESIAN_POINT('Ctrl Pts',(0.335883224496113,0.781308513635209,
-0.850377382173642));
#55636=CARTESIAN_POINT('Ctrl Pts',(-0.0716808103619085,0.847421026056226,
-0.839943419571162));
#55637=CARTESIAN_POINT('Ctrl Pts',(-0.462349004389063,0.713788436525322,
-0.829509456968682));
#55638=CARTESIAN_POINT('Ctrl Pts',(-0.74403719180775,0.411909202596066,
-0.8190754943662));
#55639=CARTESIAN_POINT('Ctrl Pts',(-0.850348818857666,0.0129390974967731,
-0.808641531763721));
#55640=CARTESIAN_POINT('Ctrl Pts',(-0.756225235669137,-0.389080874515505,
-0.798207569161238));
#55641=CARTESIAN_POINT('Ctrl Pts',(-0.483852255600829,-0.699390826881937,
-0.787773606558759));
#55642=CARTESIAN_POINT('Ctrl Pts',(-0.0974307504743618,-0.844847786786835,
-0.777339643956278));
#55643=CARTESIAN_POINT('Ctrl Pts',(0.311956098428587,-0.791166181424496,
-0.766905681353798));
#55644=CARTESIAN_POINT('Ctrl Pts',(0.647811962414489,-0.550999269808317,
-0.756471718751317));
#55645=CARTESIAN_POINT('Ctrl Pts',(0.83097245715665,-0.180956650675365,
-0.746037756148837));
#55646=CARTESIAN_POINT('Ctrl Pts',(0.818264932259306,0.23173915208976,-0.735603793546355));
#55647=CARTESIAN_POINT('Ctrl Pts',(0.612684670796792,0.589811858262646,
-0.725169830943875));
#55648=CARTESIAN_POINT('Ctrl Pts',(0.262688872936025,0.808860364965553,
-0.714735868341394));
#55649=CARTESIAN_POINT('Ctrl Pts',(-0.149225161660734,0.837252880021285,
-0.704301905738914));
#55650=CARTESIAN_POINT('Ctrl Pts',(-0.525965422875295,0.668297020729719,
-0.693867943136433));
#55651=CARTESIAN_POINT('Ctrl Pts',(-0.778730689623804,0.341817271381426,
-0.683433980533953));
#55652=CARTESIAN_POINT('Ctrl Pts',(-0.847941812434699,-0.0652320220563885,
-0.673000017931472));
#55653=CARTESIAN_POINT('Ctrl Pts',(-0.717285079048033,-0.456905514687298,
-0.662566055328991));
#55654=CARTESIAN_POINT('Ctrl Pts',(-0.417557509750832,-0.740882082404003,
-0.652132092726512));
#55655=CARTESIAN_POINT('Ctrl Pts',(-0.0194077101906099,-0.850225778697497,
-0.64169813012403));
#55656=CARTESIAN_POINT('Ctrl Pts',(0.383316669102108,-0.759163266475053,
-0.63126416752155));
#55657=CARTESIAN_POINT('Ctrl Pts',(0.695689706150895,-0.489158835893097,
-0.620830204919069));
#55658=CARTESIAN_POINT('Ctrl Pts',(0.844082139686514,-0.103855069394057,
-0.610396242316588));
#55659=CARTESIAN_POINT('Ctrl Pts',(0.793516478173852,0.305928313242129,
-0.599962279714108));
#55660=CARTESIAN_POINT('Ctrl Pts',(0.555911523369752,0.643601516593405,
-0.589528317111627));
#55661=CARTESIAN_POINT('Ctrl Pts',(0.187272996707218,0.829571792360917,
-0.579094354509147));
#55662=CARTESIAN_POINT('Ctrl Pts',(-0.225507535723487,0.820004198348112,
-0.568660391906665));
#55663=CARTESIAN_POINT('Ctrl Pts',(-0.585133822119271,0.617153906403175,
-0.558226429304186));
#55664=CARTESIAN_POINT('Ctrl Pts',(-0.806838566139565,0.268834637214886,
-0.547792466701704));
#55665=CARTESIAN_POINT('Ctrl Pts',(-0.838363875501718,-0.142851483122669,
-0.537358504099225));
#55666=CARTESIAN_POINT('Ctrl Pts',(-0.67227893843802,-0.520866166024689,
-0.526924541496743));
#55667=CARTESIAN_POINT('Ctrl Pts',(-0.347731535882055,-0.776107797235483,
-0.516490578894264));
#55668=CARTESIAN_POINT('Ctrl Pts',(0.0587794585027789,-0.848413524900877,
-0.506056616291782));
#55669=CARTESIAN_POINT('Ctrl Pts',(0.451435581967084,-0.72074020930613,
-0.495622653689302));
#55670=CARTESIAN_POINT('Ctrl Pts',(0.737684095078986,-0.423181651119361,
-0.485188691086821));
#55671=CARTESIAN_POINT('Ctrl Pts',(0.850053532442601,-0.0258751996797124,
-0.474754728484341));
#55672=CARTESIAN_POINT('Ctrl Pts',(0.762057361351739,0.377530279562073,
-0.46432076588186));
#55673=CARTESIAN_POINT('Ctrl Pts',(0.494437106533235,0.691948322969065,
-0.453886803279379));
#55674=CARTESIAN_POINT('Ctrl Pts',(0.110273377789815,0.843267642049257,
-0.443452840676898));
#55675=CARTESIAN_POINT('Ctrl Pts',(-0.299882822714393,0.795820850831183,
-0.433018878074419));
#55676=CARTESIAN_POINT('Ctrl Pts',(-0.639353822881238,0.560791604023697,
-0.422584915471937));
#55677=CARTESIAN_POINT('Ctrl Pts',(-0.828123116802315,0.193578504473986,
-0.412150952869457));
#55678=CARTESIAN_POINT('Ctrl Pts',(-0.821696007390508,-0.219262868301158,
-0.401716990266976));
#55679=CARTESIAN_POINT('Ctrl Pts',(-0.621587424751335,-0.580421921850922,
-0.391283027664496));
#55680=CARTESIAN_POINT('Ctrl Pts',(-0.274964842917683,-0.804770072220884,
-0.380849065062015));
#55681=CARTESIAN_POINT('Ctrl Pts',(0.136469537176779,-0.839426351377121,
-0.370415102459535));
#55682=CARTESIAN_POINT('Ctrl Pts',(0.51573676448633,-0.676221948589207,
-0.359981139857054));
#55683=CARTESIAN_POINT('Ctrl Pts',(0.773439988269244,-0.353625675685112,
-0.349547177254573));
#55684=CARTESIAN_POINT('Ctrl Pts',(0.848836136151767,0.0523234930784053,
-0.339113214652093));
#55685=CARTESIAN_POINT('Ctrl Pts',(0.724153627343059,0.445939522912994,
-0.328679252049612));
#55686=CARTESIAN_POINT('Ctrl Pts',(0.428781301197015,0.734443414683686,
-0.318245289447131));
#55687=CARTESIAN_POINT('Ctrl Pts',(0.0323411916877275,0.849832090513251,
-0.307811326844651));
#55688=CARTESIAN_POINT('Ctrl Pts',(-0.371722040825158,0.764907351918338,
-0.29737736424217));
#55689=CARTESIAN_POINT('Ctrl Pts',(-0.688166893772684,0.499686763789953,
-0.28694340163969));
#55690=CARTESIAN_POINT('Ctrl Pts',(-0.84240434119643,0.116685300780245,
-0.276509439037209));
#55691=CARTESIAN_POINT('Ctrl Pts',(-0.798079165673271,-0.293819969988393,
-0.266075476434728));
#55692=CARTESIAN_POINT('Ctrl Pts',(-0.565639230046271,-0.635069140343272,
-0.255641513832248));
#55693=CARTESIAN_POINT('Ctrl Pts',(-0.199872807661195,-0.826626488317455,
-0.245207551229767));
#55694=CARTESIAN_POINT('Ctrl Pts',(0.213005508499063,-0.823340312573242,
-0.234773588627287));
#55695=CARTESIAN_POINT('Ctrl Pts',(0.575676435516455,-0.625984868845304,
-0.224339626024806));
#55696=CARTESIAN_POINT('Ctrl Pts',(0.802654992386151,-0.281079332570885,
-0.213905663422325));
#55697=CARTESIAN_POINT('Ctrl Pts',(0.840440266860436,0.130080080884035,
-0.203471700819845));
#55698=CARTESIAN_POINT('Ctrl Pts',(0.680125782303049,0.510576753259713,
-0.193037738217364));
#55699=CARTESIAN_POINT('Ctrl Pts',(0.359499429618295,0.770728914207573,
-0.182603775614884));
#55700=CARTESIAN_POINT('Ctrl Pts',(-0.0458646565737162,0.849206679729665,
-0.172169813012403));
#55701=CARTESIAN_POINT('Ctrl Pts',(-0.440417346097015,0.72753091896719,
-0.161735850409923));
#55702=CARTESIAN_POINT('Ctrl Pts',(-0.731160844709429,0.434344745947377,
-0.151301887807442));
#55703=CARTESIAN_POINT('Ctrl Pts',(-0.849560168473915,0.0388279800983555,
-0.140867925204961));
#55704=CARTESIAN_POINT('Ctrl Pts',(-0.767716584589533,-0.365940025647511,
-0.13043396260248));
#55705=CARTESIAN_POINT('Ctrl Pts',(-0.5924974211277,-0.578121984952227,
-0.12347798753416));
#55706=CARTESIAN_POINT('Ctrl Pts',(-0.485033396983243,-0.657408515958423,
-0.12));
#55707=CARTESIAN_POINT('',(-0.814921455736579,-0.139942643537184,-0.12));
#55708=CARTESIAN_POINT('',(-0.485033396983246,-0.657408515958421,-0.12));
#55709=CARTESIAN_POINT('Ctrl Pts',(-0.814921455736576,-0.139942643537195,
-0.12));
#55710=CARTESIAN_POINT('Ctrl Pts',(-0.797805299826955,-0.239614354303296,
-0.12));
#55711=CARTESIAN_POINT('Ctrl Pts',(-0.76198915728887,-0.33528609840046,
-0.12));
#55712=CARTESIAN_POINT('Ctrl Pts',(-0.676216606680933,-0.475719941382479,
-0.12));
#55713=CARTESIAN_POINT('Ctrl Pts',(-0.636663795100031,-0.52585283471045,
-0.12));
#55714=CARTESIAN_POINT('Ctrl Pts',(-0.553238444854244,-0.608184477072079,
-0.12));
#55715=CARTESIAN_POINT('Ctrl Pts',(-0.51637010940319,-0.636623334743938,
-0.12));
#55716=CARTESIAN_POINT('Ctrl Pts',(-0.485033396983242,-0.657408515958424,
-0.12));
#55717=CARTESIAN_POINT('',(0.826819918308061,8.40320865522751E-9,-1.12624999033503));
#55718=CARTESIAN_POINT('Ctrl Pts',(0.82685,-1.18395083925468E-14,-1.12625));
#55719=CARTESIAN_POINT('Ctrl Pts',(0.826850000000002,0.135161967341259,
-1.12277201246584));
#55720=CARTESIAN_POINT('Ctrl Pts',(0.793089927145682,0.2702602256041,-1.11929402493168));
#55721=CARTESIAN_POINT('Ctrl Pts',(0.729464420950729,0.389454322909817,
-1.11581603739752));
#55722=CARTESIAN_POINT('Ctrl Pts',(0.665838914755776,0.508648420215534,
-1.11233804986336));
#55723=CARTESIAN_POINT('Ctrl Pts',(0.572347975220189,0.611938356564128,
-1.1088600623292));
#55724=CARTESIAN_POINT('Ctrl Pts',(0.460059281045234,0.687121564557396,
-1.10538207479504));
#55725=CARTESIAN_POINT('Ctrl Pts',(0.347770586870279,0.762304772550664,
-1.10190408726088));
#55726=CARTESIAN_POINT('Ctrl Pts',(0.216684138055956,0.809381252188606,
-1.09842609972672));
#55727=CARTESIAN_POINT('Ctrl Pts',(0.082228133557474,0.822816371973693,
-1.09494811219256));
#55728=CARTESIAN_POINT('Ctrl Pts',(-0.0522278709410078,0.836251491758779,
-1.0914701246584));
#55729=CARTESIAN_POINT('Ctrl Pts',(-0.190053431123648,0.816045251691008,
-1.08799213712424));
#55730=CARTESIAN_POINT('Ctrl Pts',(-0.314994835569263,0.764572277302744,
-1.08451414959008));
#55731=CARTESIAN_POINT('Ctrl Pts',(-0.439936240014878,0.713099302914481,
-1.08103616205592));
#55732=CARTESIAN_POINT('Ctrl Pts',(-0.551993488723467,0.630359594205724,
-1.07755817452176));
#55733=CARTESIAN_POINT('Ctrl Pts',(-0.63796533003704,0.526107851543772,
-1.0740801869876));
#55734=CARTESIAN_POINT('Ctrl Pts',(-0.723937171350614,0.421856108881819,
-1.07060219945344));
#55735=CARTESIAN_POINT('Ctrl Pts',(-0.783823605269172,0.296092332266671,
-1.06712421191928));
#55736=CARTESIAN_POINT('Ctrl Pts',(-0.810564079439897,0.163636625868307,
-1.06364622438512));
#55737=CARTESIAN_POINT('Ctrl Pts',(-0.837304553610622,0.0311809194699431,
-1.06016823685096));
#55738=CARTESIAN_POINT('Ctrl Pts',(-0.830899068033516,-0.107966716711637,
-1.0566902493168));
#55739=CARTESIAN_POINT('Ctrl Pts',(-0.792103889995619,-0.237406190245854,
-1.05321226178264));
#55740=CARTESIAN_POINT('Ctrl Pts',(-0.753308711957722,-0.36684566378007,
-1.04973427424848));
#55741=CARTESIAN_POINT('Ctrl Pts',(-0.682123841459035,-0.486576974666924,
-1.04625628671432));
#55742=CARTESIAN_POINT('Ctrl Pts',(-0.586938062717305,-0.582489677808403,
-1.04277829918016));
#55743=CARTESIAN_POINT('Ctrl Pts',(-0.491752283975575,-0.678402380949881,
-1.039300311646));
#55744=CARTESIAN_POINT('Ctrl Pts',(-0.372565596990802,-0.750496476345984,
-1.03582232411183));
#55745=CARTESIAN_POINT('Ctrl Pts',(-0.243425062820339,-0.790275105642176,
-1.03234433657767));
#55746=CARTESIAN_POINT('Ctrl Pts',(-0.114284528649877,-0.830053734938369,
-1.02886634904351));
#55747=CARTESIAN_POINT('Ctrl Pts',(0.0248098527062749,-0.837516898134649,
-1.02538836150935));
#55748=CARTESIAN_POINT('Ctrl Pts',(0.157465332643295,-0.81178514359785,
-1.02191037397519));
#55749=CARTESIAN_POINT('Ctrl Pts',(0.290120812580316,-0.78605338906105,
-1.01843238644103));
#55750=CARTESIAN_POINT('Ctrl Pts',(0.416337391098204,-0.727126716791171,
-1.01495439890687));
#55751=CARTESIAN_POINT('Ctrl Pts',(0.521239760584476,-0.641949852425356,
-1.01147641137271));
#55752=CARTESIAN_POINT('Ctrl Pts',(0.626142130070747,-0.55677298805954,
-1.00799842383855));
#55753=CARTESIAN_POINT('Ctrl Pts',(0.709730290525401,-0.445345931597789,
-1.00452043630439));
#55754=CARTESIAN_POINT('Ctrl Pts',(0.762153030458445,-0.320800915734339,
-1.00104244877023));
#55755=CARTESIAN_POINT('Ctrl Pts',(0.814575770391489,-0.19625589987089,
-0.997564461236073));
#55756=CARTESIAN_POINT('Ctrl Pts',(0.835833089802922,-0.0585929246057423,
-0.994086473701913));
#55757=CARTESIAN_POINT('Ctrl Pts',(0.823419690225199,0.0759637968315813,
-0.990608486167753));
#55758=CARTESIAN_POINT('Ctrl Pts',(0.811006290647475,0.210520518268905,
-0.987130498633592));
#55759=CARTESIAN_POINT('Ctrl Pts',(0.764922172080595,0.341970985878405,
-0.983652511099432));
#55760=CARTESIAN_POINT('Ctrl Pts',(0.690598576442017,0.45482313634507,-0.980174523565272));
#55761=CARTESIAN_POINT('Ctrl Pts',(0.616274980803439,0.567675286811736,
-0.976696536031112));
#55762=CARTESIAN_POINT('Ctrl Pts',(0.513711908093162,0.661929120135569,
-0.973218548496952));
#55763=CARTESIAN_POINT('Ctrl Pts',(0.394996892421951,0.726476383047983,
-0.969740560962791));
#55764=CARTESIAN_POINT('Ctrl Pts',(0.276281876750738,0.791023645960397,
-0.966262573428631));
#55765=CARTESIAN_POINT('Ctrl Pts',(0.14141491811859,0.825864338461392,-0.962784585894471));
#55766=CARTESIAN_POINT('Ctrl Pts',(0.00629072459521057,0.826892319144936,
-0.95930659836031));
#55767=CARTESIAN_POINT('Ctrl Pts',(-0.128833468928168,0.82792029982848,
-0.95582861082615));
#55768=CARTESIAN_POINT('Ctrl Pts',(-0.264214897342778,0.795135568694573,
-0.95235062329199));
#55769=CARTESIAN_POINT('Ctrl Pts',(-0.383898224562574,0.73240196143868,
-0.94887263575783));
#55770=CARTESIAN_POINT('Ctrl Pts',(-0.50358155178237,0.669668354182788,
-0.94539464822367));
#55771=CARTESIAN_POINT('Ctrl Pts',(-0.607566777807351,0.576985870804911,
-0.94191666068951));
#55772=CARTESIAN_POINT('Ctrl Pts',(-0.683598754197438,0.465277577070776,
-0.93843867315535));
#55773=CARTESIAN_POINT('Ctrl Pts',(-0.759630730587524,0.353569283336641,
-0.934960685621189));
#55774=CARTESIAN_POINT('Ctrl Pts',(-0.807709457342714,0.222835179246249,
-0.931482698087029));
#55775=CARTESIAN_POINT('Ctrl Pts',(-0.822168630942392,0.088482893712577,
-0.928004710552869));
#55776=CARTESIAN_POINT('Ctrl Pts',(-0.83662780454207,-0.0458693918210959,
-0.924526723018708));
#55777=CARTESIAN_POINT('Ctrl Pts',(-0.817467424986234,-0.183839858798048,
-0.921048735484548));
#55778=CARTESIAN_POINT('Ctrl Pts',(-0.76694563285593,-0.309168039331654,
-0.917570747950388));
#55779=CARTESIAN_POINT('Ctrl Pts',(-0.716423840725626,-0.43449621986526,
-0.914092760416228));
#55780=CARTESIAN_POINT('Ctrl Pts',(-0.634540636020853,-0.54718211395552,
-0.910614772882068));
#55781=CARTESIAN_POINT('Ctrl Pts',(-0.530946339389749,-0.63394515926719,
-0.907136785347908));
#55782=CARTESIAN_POINT('Ctrl Pts',(-0.427352042758645,-0.720708204578859,
-0.903658797813747));
#55783=CARTESIAN_POINT('Ctrl Pts',(-0.30204665420121,-0.781548401111939,
-0.900180810279587));
#55784=CARTESIAN_POINT('Ctrl Pts',(-0.169798002666685,-0.809295445778766,
-0.896702822745427));
#55785=CARTESIAN_POINT('Ctrl Pts',(-0.0375493511321594,-0.837042490445593,
-0.893224835211267));
#55786=CARTESIAN_POINT('Ctrl Pts',(0.101642563379456,-0.831696383246166,
-0.889746847677107));
#55787=CARTESIAN_POINT('Ctrl Pts',(0.231373319484608,-0.793887188023756,
-0.886268860142946));
#55788=CARTESIAN_POINT('Ctrl Pts',(0.36110407558976,-0.756077992801346,
-0.882790872608786));
#55789=CARTESIAN_POINT('Ctrl Pts',(0.481373673288448,-0.685805709555952,
-0.879312885074626));
#55790=CARTESIAN_POINT('Ctrl Pts',(0.578007775213603,-0.591352257171592,
-0.875834897540466));
#55791=CARTESIAN_POINT('Ctrl Pts',(0.674641877138758,-0.496898804787232,
-0.872356910006305));
#55792=CARTESIAN_POINT('Ctrl Pts',(0.747640483290378,-0.378264183263906,
-0.868878922472145));
#55793=CARTESIAN_POINT('Ctrl Pts',(0.788400364817745,-0.249430040350937,
-0.865400934937985));
#55794=CARTESIAN_POINT('Ctrl Pts',(0.829160246345111,-0.120595897437968,
-0.861922947403825));
#55795=CARTESIAN_POINT('Ctrl Pts',(0.837681403248224,0.0184377668646435,
-0.858444959869665));
#55796=CARTESIAN_POINT('Ctrl Pts',(0.81295957713844,0.151285181729246,-0.854966972335505));
#55797=CARTESIAN_POINT('Ctrl Pts',(0.788237751028655,0.284132596593849,
-0.851488984801344));
#55798=CARTESIAN_POINT('Ctrl Pts',(0.730272941905971,0.410793762020445,
-0.848010997267184));
#55799=CARTESIAN_POINT('Ctrl Pts',(0.645896574970356,0.51634106433082,-0.844533009733024));
#55800=CARTESIAN_POINT('Ctrl Pts',(0.561520208034741,0.621888366641196,
-0.841055022198864));
#55801=CARTESIAN_POINT('Ctrl Pts',(0.450732283286197,0.706321805835353,
-0.837577034664704));
#55802=CARTESIAN_POINT('Ctrl Pts',(0.326589678383619,0.759690504248875,
-0.834099047130543));
#55803=CARTESIAN_POINT('Ctrl Pts',(0.202447073481041,0.813059202662397,
-0.830621059596383));
#55804=CARTESIAN_POINT('Ctrl Pts',(0.0649497884244317,0.835363160295282,
-0.827143072062223));
#55805=CARTESIAN_POINT('Ctrl Pts',(-0.0696974754768497,0.823973750907557,
-0.823665084528063));
#55806=CARTESIAN_POINT('Ctrl Pts',(-0.204344739378132,0.812584341519832,
-0.820187096993903));
#55807=CARTESIAN_POINT('Ctrl Pts',(-0.336141982124086,0.767501565111495,
-0.816709109459743));
#55808=CARTESIAN_POINT('Ctrl Pts',(-0.449556279182332,0.694038638780562,
-0.813231121925582));
#55809=CARTESIAN_POINT('Ctrl Pts',(-0.562970576240578,0.620575712449629,
-0.809753134391422));
#55810=CARTESIAN_POINT('Ctrl Pts',(-0.658001927611118,0.518732636196097,
-0.806275146857262));
#55811=CARTESIAN_POINT('Ctrl Pts',(-0.723450441867886,0.400512095240227,
-0.802797159323102));
#55812=CARTESIAN_POINT('Ctrl Pts',(-0.788898956124654,0.282291554284355,
-0.799319171788942));
#55813=CARTESIAN_POINT('Ctrl Pts',(-0.824764633267649,0.147693548626145,
-0.795841184254781));
#55814=CARTESIAN_POINT('Ctrl Pts',(-0.826820534669346,0.0125810858710678,
-0.792363196720621));
#55815=CARTESIAN_POINT('Ctrl Pts',(-0.828876436071043,-0.122531376884008,
-0.788885209186461));
#55816=CARTESIAN_POINT('Ctrl Pts',(-0.79712256173144,-0.258158296735951,
-0.7854072216523));
#55817=CARTESIAN_POINT('Ctrl Pts',(-0.735301254991326,-0.378315403705377,
-0.78192923411814));
#55818=CARTESIAN_POINT('Ctrl Pts',(-0.67347994825121,-0.498472510674805,
-0.77845124658398));
#55819=CARTESIAN_POINT('Ctrl Pts',(-0.581591209110583,-0.603159804761717,
-0.77497325904982));
#55820=CARTESIAN_POINT('Ctrl Pts',(-0.470464557373384,-0.68003939630587,
-0.77149527151566));
#55821=CARTESIAN_POINT('Ctrl Pts',(-0.359337905636187,-0.756918987850021,
-0.768017283981499));
#55822=CARTESIAN_POINT('Ctrl Pts',(-0.228973341302421,-0.805990876851411,
-0.76453929644734));
#55823=CARTESIAN_POINT('Ctrl Pts',(-0.0947349410194663,-0.82147171054311,
-0.761061308913179));
#55824=CARTESIAN_POINT('Ctrl Pts',(0.0395034592634891,-0.83695254423481,
-0.757583321379019));
#55825=CARTESIAN_POINT('Ctrl Pts',(0.177615695495633,-0.818842322616818,
-0.754105333844859));
#55826=CARTESIAN_POINT('Ctrl Pts',(0.303324591480697,-0.769275420428635,
-0.750627346310698));
#55827=CARTESIAN_POINT('Ctrl Pts',(0.42903348746576,-0.719708518240453,
-0.747149358776538));
#55828=CARTESIAN_POINT('Ctrl Pts',(0.542339043203747,-0.638684935482078,
-0.743671371242378));
#55829=CARTESIAN_POINT('Ctrl Pts',(0.629887666391188,-0.535753682209324,
-0.740193383708218));
#55830=CARTESIAN_POINT('Ctrl Pts',(0.71743628957863,-0.432822428936568,
-0.736715396174058));
#55831=CARTESIAN_POINT('Ctrl Pts',(0.779227980215528,-0.307983505149434,
-0.733237408639898));
#55832=CARTESIAN_POINT('Ctrl Pts',(0.807980297126493,-0.175949764785207,
-0.729759421105738));
#55833=CARTESIAN_POINT('Ctrl Pts',(0.836732614037458,-0.0439160244209799,
-0.726281433571577));
#55834=CARTESIAN_POINT('Ctrl Pts',(0.83244555722249,0.0953125325203378,
-0.722803446037417));
#55835=CARTESIAN_POINT('Ctrl Pts',(0.795624376477293,0.22532716619996,-0.719325458503256));
#55836=CARTESIAN_POINT('Ctrl Pts',(0.758803195732096,0.355341799879582,
-0.715847470969096));
#55837=CARTESIAN_POINT('Ctrl Pts',(0.689447891056671,0.476142510297508,
-0.712369483434936));
#55838=CARTESIAN_POINT('Ctrl Pts',(0.595732311091411,0.573492365942453,
-0.708891495900776));
#55839=CARTESIAN_POINT('Ctrl Pts',(0.502016731126152,0.670842221587398,
-0.705413508366616));
#55840=CARTESIAN_POINT('Ctrl Pts',(0.383940875871059,0.744741222459363,
-0.701935520832456));
#55841=CARTESIAN_POINT('Ctrl Pts',(0.255420539849088,0.786480023964872,
-0.698457533298296));
#55842=CARTESIAN_POINT('Ctrl Pts',(0.126900203827117,0.828218825470381,
-0.694979545764135));
#55843=CARTESIAN_POINT('Ctrl Pts',(-0.0120646129617348,0.837797427609435,
-0.691501558229975));
#55844=CARTESIAN_POINT('Ctrl Pts',(-0.145096253695276,0.814086947098516,
-0.688023570695815));
#55845=CARTESIAN_POINT('Ctrl Pts',(-0.278127894428818,0.790376466587597,
-0.684545583161654));
#55846=CARTESIAN_POINT('Ctrl Pts',(-0.405226359107049,0.733376903426708,
-0.681067595627494));
#55847=CARTESIAN_POINT('Ctrl Pts',(-0.511412496278356,0.649805924044191,
-0.677589608093334));
#55848=CARTESIAN_POINT('Ctrl Pts',(-0.617598633449664,0.566234944661674,
-0.674111620559174));
#55849=CARTESIAN_POINT('Ctrl Pts',(-0.702872443114044,0.456092549057531,
-0.670633633025015));
#55850=CARTESIAN_POINT('Ctrl Pts',(-0.757184005997862,0.332359536245938,
-0.667155645490854));
#55851=CARTESIAN_POINT('Ctrl Pts',(-0.811495568881679,0.208626523434346,
-0.663677657956694));
#55852=CARTESIAN_POINT('Ctrl Pts',(-0.834844884984934,0.0713028934153015,
-0.660199670422533));
#55853=CARTESIAN_POINT('Ctrl Pts',(-0.824480127658203,-0.0634271185637466,
-0.656721682888373));
#55854=CARTESIAN_POINT('Ctrl Pts',(-0.814115370331471,-0.198157130542796,
-0.653243695354212));
#55855=CARTESIAN_POINT('Ctrl Pts',(-0.770036539574752,-0.330293524481851,
-0.649765707820053));
#55856=CARTESIAN_POINT('Ctrl Pts',(-0.697438532772424,-0.444263405286587,
-0.646287720285893));
#55857=CARTESIAN_POINT('Ctrl Pts',(-0.624840525970095,-0.558233286091323,
-0.642809732751732));
#55858=CARTESIAN_POINT('Ctrl Pts',(-0.523723343122159,-0.654036653761738,
-0.639331745217572));
#55859=CARTESIAN_POINT('Ctrl Pts',(-0.406004119499086,-0.720382631122071,
-0.635853757683411));
#55860=CARTESIAN_POINT('Ctrl Pts',(-0.288284895876013,-0.786728608482404,
-0.632375770149251));
#55861=CARTESIAN_POINT('Ctrl Pts',(-0.153963631477803,-0.823617195532651,
-0.628897782615092));
#55862=CARTESIAN_POINT('Ctrl Pts',(-0.018870718651746,-0.82670089890489,
-0.625419795080931));
#55863=CARTESIAN_POINT('Ctrl Pts',(0.116222194174311,-0.829784602277128,
-0.621941807546771));
#55864=CARTESIAN_POINT('Ctrl Pts',(0.252086755428218,-0.799063421971358,
-0.618463820012611));
#55865=CARTESIAN_POINT('Ctrl Pts',(0.372710687974431,-0.738157993482569,
-0.614985832478451));
#55866=CARTESIAN_POINT('Ctrl Pts',(0.493334620520646,-0.677252564993779,
-0.61150784494429));
#55867=CARTESIAN_POINT('Ctrl Pts',(0.598717924359164,-0.586162888321972,
-0.608029857410131));
#55868=CARTESIAN_POINT('Ctrl Pts',(0.676440681809117,-0.475624310003393,
-0.604551869875971));
#55869=CARTESIAN_POINT('Ctrl Pts',(0.754163439259069,-0.365085731684814,
-0.60107388234181));
#55870=CARTESIAN_POINT('Ctrl Pts',(0.804225650320453,-0.235098251719462,
-0.59759589480765));
#55871=CARTESIAN_POINT('Ctrl Pts',(0.820727248116851,-0.100981505589522,
-0.594117907273489));
#55872=CARTESIAN_POINT('Ctrl Pts',(0.837228845913249,0.0331352405404182,
-0.590639919739329));
#55873=CARTESIAN_POINT('Ctrl Pts',(0.820169830444662,0.171381252834949,
-0.587161932205169));
#55874=CARTESIAN_POINT('Ctrl Pts',(0.771560686864993,0.29746358896007,-0.583683944671009));
#55875=CARTESIAN_POINT('Ctrl Pts',(0.722951543285324,0.42354592508519,-0.580205957136849));
#55876=CARTESIAN_POINT('Ctrl Pts',(0.642792271594575,0.537464585040901,
-0.576727969602689));
#55877=CARTESIAN_POINT('Ctrl Pts',(0.540530018726793,0.625793719309964,
-0.573249982068529));
#55878=CARTESIAN_POINT('Ctrl Pts',(0.43826776585901,0.714122853579028,-0.569771994534368));
#55879=CARTESIAN_POINT('Ctrl Pts',(0.313902531814194,0.776862462161444,
-0.566294007000208));
#55880=CARTESIAN_POINT('Ctrl Pts',(0.182091343967062,0.80661838729653,-0.562816019466048));
#55881=CARTESIAN_POINT('Ctrl Pts',(0.0502801561199283,0.836374312431616,
-0.559338031931887));
#55882=CARTESIAN_POINT('Ctrl Pts',(-0.0889769855295217,0.833146554119371,
-0.555860044397727));
#55883=CARTESIAN_POINT('Ctrl Pts',(-0.219267972300293,0.79731551884803,
-0.552382056863567));
#55884=CARTESIAN_POINT('Ctrl Pts',(-0.34955895907106,0.76148448357669,-0.548904069329407));
#55885=CARTESIAN_POINT('Ctrl Pts',(-0.470883790963148,0.693050171346257,
-0.545426081795247));
#55886=CARTESIAN_POINT('Ctrl Pts',(-0.568943766286064,0.600077887508625,
-0.541948094261086));
#55887=CARTESIAN_POINT('Ctrl Pts',(-0.667003741608982,0.507105603670991,
-0.538470106726926));
#55888=CARTESIAN_POINT('Ctrl Pts',(-0.741798860362727,0.389595348226158,
-0.534992119192766));
#55889=CARTESIAN_POINT('Ctrl Pts',(-0.784514166249514,0.261396257101007,
-0.531514131658606));
#55890=CARTESIAN_POINT('Ctrl Pts',(-0.827229472136301,0.133197165975855,
-0.528036144124446));
#55891=CARTESIAN_POINT('Ctrl Pts',(-0.83786496515613,-0.00569076082960968,
-0.524558156590286));
#55892=CARTESIAN_POINT('Ctrl Pts',(-0.815167202467579,-0.138898928339155,
-0.521080169056126));
#55893=CARTESIAN_POINT('Ctrl Pts',(-0.79246943977903,-0.272107095848698,
-0.517602181521965));
#55894=CARTESIAN_POINT('Ctrl Pts',(-0.736438421382098,-0.399635504062321,
-0.514124193987804));
#55895=CARTESIAN_POINT('Ctrl Pts',(-0.653677666152339,-0.506454330661924,
-0.510646206453644));
#55896=CARTESIAN_POINT('Ctrl Pts',(-0.570916910922578,-0.613273157261528,
-0.507168218919484));
#55897=CARTESIAN_POINT('Ctrl Pts',(-0.461426418859987,-0.699382402247118,
-0.503690231385324));
#55898=CARTESIAN_POINT('Ctrl Pts',(-0.338110159082288,-0.754633686365733,
-0.500212243851164));
#55899=CARTESIAN_POINT('Ctrl Pts',(-0.214793899304592,-0.809884970484346,
-0.496734256317004));
#55900=CARTESIAN_POINT('Ctrl Pts',(-0.0776518718117877,-0.834278293735986,
-0.493256268782844));
#55901=CARTESIAN_POINT('Ctrl Pts',(0.0571530908599681,-0.824938788321739,
-0.489778281248683));
#55902=CARTESIAN_POINT('Ctrl Pts',(0.191958053531728,-0.815599282907491,
-0.486300293714523));
#55903=CARTESIAN_POINT('Ctrl Pts',(0.324425951382439,-0.772526948827354,
-0.482822306180363));
#55904=CARTESIAN_POINT('Ctrl Pts',(0.438944820023649,-0.700798063101627,
-0.479344318646203));
#55905=CARTESIAN_POINT('Ctrl Pts',(0.553463688664858,-0.6290691773759,-0.475866331112043));
#55906=CARTESIAN_POINT('Ctrl Pts',(0.650033528096565,-0.528683740004585,
-0.472388343577882));
#55907=CARTESIAN_POINT('Ctrl Pts',(0.717273128843362,-0.411472646614376,
-0.468910356043722));
#55908=CARTESIAN_POINT('Ctrl Pts',(0.784512729590159,-0.294261553224167,
-0.465432368509562));
#55909=CARTESIAN_POINT('Ctrl Pts',(0.822422091652046,-0.160224803815064,
-0.461954380975402));
#55910=CARTESIAN_POINT('Ctrl Pts',(0.826533418528119,-0.0251592593056137,
-0.458476393441242));
#55911=CARTESIAN_POINT('Ctrl Pts',(0.830644745404193,0.109906285203834,
-0.454998405907081));
#55912=CARTESIAN_POINT('Ctrl Pts',(0.800958037094454,0.246000624813629,
-0.451520418372921));
#55913=CARTESIAN_POINT('Ctrl Pts',(0.740972011706928,0.367084401928998,
-0.448042430838761));
#55914=CARTESIAN_POINT('Ctrl Pts',(0.680985986319401,0.488168179044368,
-0.444564443304601));
#55915=CARTESIAN_POINT('Ctrl Pts',(0.590700643854085,0.594241393665313,
-0.441086455770441));
#55916=CARTESIAN_POINT('Ctrl Pts',(0.480756536280455,0.672802818882485,
-0.437608468236281));
#55917=CARTESIAN_POINT('Ctrl Pts',(0.370812428706822,0.751364244099658,
-0.43413048070212));
#55918=CARTESIAN_POINT('Ctrl Pts',(0.241209556024874,0.802413879913059,
-0.43065249316796));
#55919=CARTESIAN_POINT('Ctrl Pts',(0.107222225940712,0.819935286798217,
-0.427174505633799));
#55920=CARTESIAN_POINT('Ctrl Pts',(-0.0267651041434491,0.837456693683375,
-0.423696518099639));
#55921=CARTESIAN_POINT('Ctrl Pts',(-0.165136891629824,0.821449871640292,
-0.420218530565479));
#55922=CARTESIAN_POINT('Ctrl Pts',(-0.291585370986894,0.773801299882001,
-0.416740543031319));
#55923=CARTESIAN_POINT('Ctrl Pts',(-0.418033850343963,0.726152728123709,
-0.413262555497159));
#55924=CARTESIAN_POINT('Ctrl Pts',(-0.532559021571728,0.646862406650209,
-0.409784567962999));
#55925=CARTESIAN_POINT('Ctrl Pts',(-0.621663554948791,0.545275072528486,
-0.406306580428838));
#55926=CARTESIAN_POINT('Ctrl Pts',(-0.710768088325855,0.443687738406764,
-0.402828592894678));
#55927=CARTESIAN_POINT('Ctrl Pts',(-0.774451983852219,0.319803391636819,
-0.399350605360518));
#55928=CARTESIAN_POINT('Ctrl Pts',(-0.805209795112539,0.188222384767189,
-0.395872617826358));
#55929=CARTESIAN_POINT('Ctrl Pts',(-0.835967606372859,0.0566413778975608,
-0.392394630292198));
#55930=CARTESIAN_POINT('Ctrl Pts',(-0.833799333367138,-0.0826362890717533,
-0.388916642758038));
#55931=CARTESIAN_POINT('Ctrl Pts',(-0.798960517260375,-0.213196088453224,
-0.385438655223877));
#55932=CARTESIAN_POINT('Ctrl Pts',(-0.764121701153612,-0.343755887834697,
-0.381960667689717));
#55933=CARTESIAN_POINT('Ctrl Pts',(-0.696612341945807,-0.465597819628327,
-0.378482680155557));
#55934=CARTESIAN_POINT('Ctrl Pts',(-0.604388734927783,-0.564362239491937,
-0.375004692621397));
#55935=CARTESIAN_POINT('Ctrl Pts',(-0.512165127909759,-0.663126659355548,
-0.371526705087236));
#55936=CARTESIAN_POINT('Ctrl Pts',(-0.395227273081517,-0.738813567289139,
-0.368048717553076));
#55937=CARTESIAN_POINT('Ctrl Pts',(-0.267356846266639,-0.782502905444178,
-0.364570730018916));
#55938=CARTESIAN_POINT('Ctrl Pts',(-0.139486419451759,-0.826192243599218,
-0.361092742484756));
#55939=CARTESIAN_POINT('Ctrl Pts',(-0.000683420650243682,-0.837884011975705,
-0.357614754950596));
#55940=CARTESIAN_POINT('Ctrl Pts',(0.132693564325656,-0.816200280725184,
-0.354136767416435));
#55941=CARTESIAN_POINT('Ctrl Pts',(0.266070549301554,-0.794516549474664,
-0.350658779882275));
#55942=CARTESIAN_POINT('Ctrl Pts',(0.394021520451837,-0.739457318597138,
-0.347180792348115));
#55943=CARTESIAN_POINT('Ctrl Pts',(0.501466854431083,-0.657511577224757,
-0.343702804813955));
#55944=CARTESIAN_POINT('Ctrl Pts',(0.608912188410329,-0.575565835852376,
-0.340224817279794));
#55945=CARTESIAN_POINT('Ctrl Pts',(0.695851885218537,-0.466733583985141,
-0.336746829745634));
#55946=CARTESIAN_POINT('Ctrl Pts',(0.752039692950413,-0.343841214072567,
-0.333268842211474));
#55947=CARTESIAN_POINT('Ctrl Pts',(0.808227500682287,-0.220948844159995,
-0.329790854677314));
#55948=CARTESIAN_POINT('Ctrl Pts',(0.83366341933783,-0.0839963562020835,
-0.326312867143154));
#55949=CARTESIAN_POINT('Ctrl Pts',(0.825349706352787,0.050875755454292,
-0.322834879608994));
#55950=CARTESIAN_POINT('Ctrl Pts',(0.817035993367744,0.185747867110668,
-0.319356892074833));
#55951=CARTESIAN_POINT('Ctrl Pts',(0.774972648742117,0.318539602465508,
-0.315878904540673));
#55952=CARTESIAN_POINT('Ctrl Pts',(0.704117035339796,0.433600831232204,
-0.312400917006513));
#55953=CARTESIAN_POINT('Ctrl Pts',(0.633261421937474,0.548662059998902,
-0.308922929472353));
#55954=CARTESIAN_POINT('Ctrl Pts',(0.533613539758457,0.645992782177456,
-0.305444941938193));
#55955=CARTESIAN_POINT('Ctrl Pts',(0.416917360096596,0.7141221149324,-0.301966954404032));
#55956=CARTESIAN_POINT('Ctrl Pts',(0.300221180434735,0.782251447687343,
-0.298488966869872));
#55957=CARTESIAN_POINT('Ctrl Pts',(0.16647670329003,0.821179391018677,-0.295010979335712));
#55958=CARTESIAN_POINT('Ctrl Pts',(0.031446343894929,0.826318103348089,
-0.291532991801552));
#55959=CARTESIAN_POINT('Ctrl Pts',(-0.103584015500172,0.8314568156775,-0.288055004267392));
#55960=CARTESIAN_POINT('Ctrl Pts',(-0.239900257145668,0.802806297004991,
-0.284577016733231));
#55961=CARTESIAN_POINT('Ctrl Pts',(-0.361436871197806,0.743743146577004,
-0.281099029199071));
#55962=CARTESIAN_POINT('Ctrl Pts',(-0.482973485249944,0.684679996149017,
-0.277621041664911));
#55963=CARTESIAN_POINT('Ctrl Pts',(-0.589730471708724,0.595204213965552,
-0.274143054130751));
#55964=CARTESIAN_POINT('Ctrl Pts',(-0.669126018040229,0.485860939630313,
-0.270665066596591));
#55965=CARTESIAN_POINT('Ctrl Pts',(-0.748521564371732,0.376517665295076,
-0.267187079062431));
#55966=CARTESIAN_POINT('Ctrl Pts',(-0.800555670575961,0.247306898808065,
-0.26370909152827));
#55967=CARTESIAN_POINT('Ctrl Pts',(-0.819095872468407,0.113456740014407,
-0.26023110399411));
#55968=CARTESIAN_POINT('Ctrl Pts',(-0.837636074360853,-0.0203934187792517,
-0.25675311645995));
#55969=CARTESIAN_POINT('Ctrl Pts',(-0.822682371941515,-0.158882969879557,
-0.25327512892579));
#55970=CARTESIAN_POINT('Ctrl Pts',(-0.775997129713513,-0.285690276024395,
-0.24979714139163));
#55971=CARTESIAN_POINT('Ctrl Pts',(-0.729311887485511,-0.412497582169235,
-0.246319153857469));
#55972=CARTESIAN_POINT('Ctrl Pts',(-0.650895105448843,-0.527622643358608,
-0.242841166323309));
#55973=CARTESIAN_POINT('Ctrl Pts',(-0.549988569180355,-0.617497415744048,
-0.239363178789149));
#55974=CARTESIAN_POINT('Ctrl Pts',(-0.449082032911868,-0.707372188129487,
-0.235885191254989));
#55975=CARTESIAN_POINT('Ctrl Pts',(-0.325685742411561,-0.771996671710993,
-0.232407203720828));
#55976=CARTESIAN_POINT('Ctrl Pts',(-0.194342531999369,-0.803754595401518,
-0.228929216186668));
#55977=CARTESIAN_POINT('Ctrl Pts',(-0.0629993215871771,-0.835512519092042,
-0.225451228652508));
#55978=CARTESIAN_POINT('Ctrl Pts',(0.0762908087369,-0.834403882891584,-0.221973241118348));
#55979=CARTESIAN_POINT('Ctrl Pts',(0.207111865361516,-0.800559289665401,
-0.218495253584188));
#55980=CARTESIAN_POINT('Ctrl Pts',(0.337932921986132,-0.766714696439218,
-0.215017266050027));
#55981=CARTESIAN_POINT('Ctrl Pts',(0.460284904911287,-0.70013414618731,
-0.211539278515867));
#55982=CARTESIAN_POINT('Ctrl Pts',(0.559748052092256,-0.608664578014501,
-0.208061290981707));
#55983=CARTESIAN_POINT('Ctrl Pts',(0.659211199273223,-0.517195009841694,
-0.204583303447547));
#55984=CARTESIAN_POINT('Ctrl Pts',(0.735785510710006,-0.400836423747985,
-0.201105315913387));
#55985=CARTESIAN_POINT('Ctrl Pts',(0.780446355236762,-0.273302013173142,
-0.197627328379227));
#55986=CARTESIAN_POINT('Ctrl Pts',(0.825107199763519,-0.145767602598297,
-0.194149340845066));
#55987=CARTESIAN_POINT('Ctrl Pts',(0.837854577380249,-0.00705736754231678,
-0.190671353310906));
#55988=CARTESIAN_POINT('Ctrl Pts',(0.817186127412103,0.126480620590234,
-0.187193365776746));
#55989=CARTESIAN_POINT('Ctrl Pts',(0.796517677443957,0.260018608722786,
-0.183715378242586));
#55990=CARTESIAN_POINT('Ctrl Pts',(0.742433399890935,0.388384349931908,
-0.180237390708426));
#55991=CARTESIAN_POINT('Ctrl Pts',(0.661307424905576,0.496450160114788,
-0.176759403174265));
#55992=CARTESIAN_POINT('Ctrl Pts',(0.580181449920217,0.604515970297668,
-0.173281415640105));
#55993=CARTESIAN_POINT('Ctrl Pts',(0.472013777502521,0.692281849454306,
-0.169803428105945));
#55994=CARTESIAN_POINT('Ctrl Pts',(0.349552390106812,0.749402561227559,
-0.166325440571785));
#55995=CARTESIAN_POINT('Ctrl Pts',(0.227091002711104,0.806523273000812,
-0.162847453037624));
#55996=CARTESIAN_POINT('Ctrl Pts',(0.0903359003373833,0.83299881739068,
-0.159369465503464));
#55997=CARTESIAN_POINT('Ctrl Pts',(-0.0445955159864435,0.825712101000813,
-0.155891477969304));
#55998=CARTESIAN_POINT('Ctrl Pts',(-0.17952693231027,0.818425384610945,
-0.152413490435144));
#55999=CARTESIAN_POINT('Ctrl Pts',(-0.312634662584204,0.777376407441342,
-0.148935502900984));
#56000=CARTESIAN_POINT('Ctrl Pts',(-0.428231669765087,0.707396742051741,
-0.145457515366823));
#56001=CARTESIAN_POINT('Ctrl Pts',(-0.543828676945968,0.637417076662141,
-0.141979527832663));
#56002=CARTESIAN_POINT('Ctrl Pts',(-0.6419149610338,0.538506723052544,-0.138501540298503));
#56003=CARTESIAN_POINT('Ctrl Pts',(-0.710929916311711,0.422335058963047,
-0.135023552764343));
#56004=CARTESIAN_POINT('Ctrl Pts',(-0.779944871589624,0.306163394873548,
-0.131545565230183));
#56005=CARTESIAN_POINT('Ctrl Pts',(-0.819888498057614,0.172730420304148,
-0.128067577696022));
#56006=CARTESIAN_POINT('Ctrl Pts',(-0.826054786734804,0.0377369297661749,
-0.124589590161862));
#56007=CARTESIAN_POINT('Ctrl Pts',(-0.828767153927045,-0.0216426961432744,
-0.123059726774575));
#56008=CARTESIAN_POINT('Ctrl Pts',(-0.824944083444903,-0.0813242598465086,
-0.121529863387287));
#56009=CARTESIAN_POINT('Ctrl Pts',(-0.814862045042683,-0.139933199781809,
-0.12));
#56010=CARTESIAN_POINT('',(0.589301091561381,0.565833523687246,-1.12625));
#56011=CARTESIAN_POINT('Ctrl Pts',(0.589301091561381,0.565833523687246,
-1.12625));
#56012=CARTESIAN_POINT('Ctrl Pts',(0.616667481029585,0.540044898914149,
-1.12625));
#56013=CARTESIAN_POINT('Ctrl Pts',(0.648190221269366,0.505777024736586,
-1.12625));
#56014=CARTESIAN_POINT('Ctrl Pts',(0.716478059012945,0.410513493212772,
-1.12625));
#56015=CARTESIAN_POINT('Ctrl Pts',(0.746976021141481,0.354408470381541,
-1.12625));
#56016=CARTESIAN_POINT('Ctrl Pts',(0.807743006623444,0.201482947924183,
-1.12625));
#56017=CARTESIAN_POINT('Ctrl Pts',(0.826850000000001,0.10113013137271,-1.12625));
#56018=CARTESIAN_POINT('Ctrl Pts',(0.82685,-1.11022302462516E-14,-1.12625));
#56019=CARTESIAN_POINT('Ctrl Pts',(0.589258732516958,0.56579182741905,-1.12625));
#56020=CARTESIAN_POINT('Ctrl Pts',(0.548574338866333,0.608188043340012,
-1.12472013661271));
#56021=CARTESIAN_POINT('Ctrl Pts',(0.400588145741338,0.732737761006612,
-1.11971228569126));
#56022=CARTESIAN_POINT('Ctrl Pts',(0.0845750992767583,0.84622608784569,
-1.11122644723566));
#56023=CARTESIAN_POINT('Ctrl Pts',(-0.323961995775528,0.786331547179381,
-1.10079248463318));
#56024=CARTESIAN_POINT('Ctrl Pts',(-0.656117677249225,0.541077762637857,
-1.0903585220307));
#56025=CARTESIAN_POINT('Ctrl Pts',(-0.833630685095572,0.168293731192079,
-1.07992455942822));
#56026=CARTESIAN_POINT('Ctrl Pts',(-0.814643797129344,-0.244162209445375,
-1.06949059682573));
#56027=CARTESIAN_POINT('Ctrl Pts',(-0.603640408739925,-0.599065043663486,
-1.05905663422325));
#56028=CARTESIAN_POINT('Ctrl Pts',(-0.250351927233731,-0.812763520669612,
-1.04862267162077));
#56029=CARTESIAN_POINT('Ctrl Pts',(0.161946157548475,-0.834885534961222,
-1.03818870901829));
#56030=CARTESIAN_POINT('Ctrl Pts',(0.536072366553588,-0.660217414778485,
-1.02775474641581));
#56031=CARTESIAN_POINT('Ctrl Pts',(0.783841098330598,-0.32992972433277,
-1.01732078381333));
#56032=CARTESIAN_POINT('Ctrl Pts',(0.846851206973998,0.0781254429130661,
-1.00688682121085));
#56033=CARTESIAN_POINT('Ctrl Pts',(0.710250478470448,0.467765739743972,
-0.996452858608371));
#56034=CARTESIAN_POINT('Ctrl Pts',(0.406237059412565,0.747149238803466,
-0.98601889600589));
#56035=CARTESIAN_POINT('Ctrl Pts',(0.00646973450489691,0.850422646762807,
-0.97558493340341));
#56036=CARTESIAN_POINT('Ctrl Pts',(-0.394822561461409,0.753243438481209,
-0.965150970800928));
#56037=CARTESIAN_POINT('Ctrl Pts',(-0.703051471340727,0.478517673019027,
-0.954717008198449));
#56038=CARTESIAN_POINT('Ctrl Pts',(-0.845564538846854,0.0910007927061417,
-0.944283045595967));
#56039=CARTESIAN_POINT('Ctrl Pts',(-0.78877009670225,-0.317965829356397,
-0.933849082993488));
#56040=CARTESIAN_POINT('Ctrl Pts',(-0.546055127582371,-0.65198491670129,
-0.923415120391006));
#56041=CARTESIAN_POINT('Ctrl Pts',(-0.174629831956398,-0.83232503011057,
-0.912981157788526));
#56042=CARTESIAN_POINT('Ctrl Pts',(0.237957356762347,-0.816478309791074,
-0.902547195186046));
#56043=CARTESIAN_POINT('Ctrl Pts',(0.59445575953915,-0.608179976581176,
-0.892113232583564));
#56044=CARTESIAN_POINT('Ctrl Pts',(0.810835351688311,-0.256527905763967,
-0.881679269981085));
#56045=CARTESIAN_POINT('Ctrl Pts',(0.836093429239884,0.15559020392044,-0.871245307378603));
#56046=CARTESIAN_POINT('Ctrl Pts',(0.664276425899862,0.531034239923243,
-0.860811344776123));
#56047=CARTESIAN_POINT('Ctrl Pts',(0.335883224496113,0.781308513635209,
-0.850377382173642));
#56048=CARTESIAN_POINT('Ctrl Pts',(-0.0716808103619085,0.847421026056226,
-0.839943419571162));
#56049=CARTESIAN_POINT('Ctrl Pts',(-0.462349004389063,0.713788436525322,
-0.829509456968682));
#56050=CARTESIAN_POINT('Ctrl Pts',(-0.74403719180775,0.411909202596066,
-0.8190754943662));
#56051=CARTESIAN_POINT('Ctrl Pts',(-0.850348818857666,0.0129390974967731,
-0.808641531763721));
#56052=CARTESIAN_POINT('Ctrl Pts',(-0.756225235669137,-0.389080874515505,
-0.798207569161238));
#56053=CARTESIAN_POINT('Ctrl Pts',(-0.483852255600829,-0.699390826881937,
-0.787773606558759));
#56054=CARTESIAN_POINT('Ctrl Pts',(-0.0974307504743618,-0.844847786786835,
-0.777339643956278));
#56055=CARTESIAN_POINT('Ctrl Pts',(0.311956098428587,-0.791166181424496,
-0.766905681353798));
#56056=CARTESIAN_POINT('Ctrl Pts',(0.647811962414489,-0.550999269808317,
-0.756471718751317));
#56057=CARTESIAN_POINT('Ctrl Pts',(0.83097245715665,-0.180956650675365,
-0.746037756148837));
#56058=CARTESIAN_POINT('Ctrl Pts',(0.818264932259306,0.23173915208976,-0.735603793546355));
#56059=CARTESIAN_POINT('Ctrl Pts',(0.612684670796792,0.589811858262646,
-0.725169830943875));
#56060=CARTESIAN_POINT('Ctrl Pts',(0.262688872936025,0.808860364965553,
-0.714735868341394));
#56061=CARTESIAN_POINT('Ctrl Pts',(-0.149225161660734,0.837252880021285,
-0.704301905738914));
#56062=CARTESIAN_POINT('Ctrl Pts',(-0.525965422875295,0.668297020729719,
-0.693867943136433));
#56063=CARTESIAN_POINT('Ctrl Pts',(-0.778730689623804,0.341817271381426,
-0.683433980533953));
#56064=CARTESIAN_POINT('Ctrl Pts',(-0.847941812434699,-0.0652320220563885,
-0.673000017931472));
#56065=CARTESIAN_POINT('Ctrl Pts',(-0.717285079048033,-0.456905514687298,
-0.662566055328991));
#56066=CARTESIAN_POINT('Ctrl Pts',(-0.417557509750832,-0.740882082404003,
-0.652132092726512));
#56067=CARTESIAN_POINT('Ctrl Pts',(-0.0194077101906099,-0.850225778697497,
-0.64169813012403));
#56068=CARTESIAN_POINT('Ctrl Pts',(0.383316669102108,-0.759163266475053,
-0.63126416752155));
#56069=CARTESIAN_POINT('Ctrl Pts',(0.695689706150895,-0.489158835893097,
-0.620830204919069));
#56070=CARTESIAN_POINT('Ctrl Pts',(0.844082139686514,-0.103855069394057,
-0.610396242316588));
#56071=CARTESIAN_POINT('Ctrl Pts',(0.793516478173852,0.305928313242129,
-0.599962279714108));
#56072=CARTESIAN_POINT('Ctrl Pts',(0.555911523369752,0.643601516593405,
-0.589528317111627));
#56073=CARTESIAN_POINT('Ctrl Pts',(0.187272996707218,0.829571792360917,
-0.579094354509147));
#56074=CARTESIAN_POINT('Ctrl Pts',(-0.225507535723487,0.820004198348112,
-0.568660391906665));
#56075=CARTESIAN_POINT('Ctrl Pts',(-0.585133822119271,0.617153906403175,
-0.558226429304186));
#56076=CARTESIAN_POINT('Ctrl Pts',(-0.806838566139565,0.268834637214886,
-0.547792466701704));
#56077=CARTESIAN_POINT('Ctrl Pts',(-0.838363875501718,-0.142851483122669,
-0.537358504099225));
#56078=CARTESIAN_POINT('Ctrl Pts',(-0.67227893843802,-0.520866166024689,
-0.526924541496743));
#56079=CARTESIAN_POINT('Ctrl Pts',(-0.347731535882055,-0.776107797235483,
-0.516490578894264));
#56080=CARTESIAN_POINT('Ctrl Pts',(0.0587794585027789,-0.848413524900877,
-0.506056616291782));
#56081=CARTESIAN_POINT('Ctrl Pts',(0.451435581967084,-0.72074020930613,
-0.495622653689302));
#56082=CARTESIAN_POINT('Ctrl Pts',(0.737684095078986,-0.423181651119361,
-0.485188691086821));
#56083=CARTESIAN_POINT('Ctrl Pts',(0.850053532442601,-0.0258751996797124,
-0.474754728484341));
#56084=CARTESIAN_POINT('Ctrl Pts',(0.762057361351739,0.377530279562073,
-0.46432076588186));
#56085=CARTESIAN_POINT('Ctrl Pts',(0.494437106533235,0.691948322969065,
-0.453886803279379));
#56086=CARTESIAN_POINT('Ctrl Pts',(0.110273377789815,0.843267642049257,
-0.443452840676898));
#56087=CARTESIAN_POINT('Ctrl Pts',(-0.299882822714393,0.795820850831183,
-0.433018878074419));
#56088=CARTESIAN_POINT('Ctrl Pts',(-0.639353822881238,0.560791604023697,
-0.422584915471937));
#56089=CARTESIAN_POINT('Ctrl Pts',(-0.828123116802315,0.193578504473986,
-0.412150952869457));
#56090=CARTESIAN_POINT('Ctrl Pts',(-0.821696007390508,-0.219262868301158,
-0.401716990266976));
#56091=CARTESIAN_POINT('Ctrl Pts',(-0.621587424751335,-0.580421921850922,
-0.391283027664496));
#56092=CARTESIAN_POINT('Ctrl Pts',(-0.274964842917683,-0.804770072220884,
-0.380849065062015));
#56093=CARTESIAN_POINT('Ctrl Pts',(0.136469537176779,-0.839426351377121,
-0.370415102459535));
#56094=CARTESIAN_POINT('Ctrl Pts',(0.51573676448633,-0.676221948589207,
-0.359981139857054));
#56095=CARTESIAN_POINT('Ctrl Pts',(0.773439988269244,-0.353625675685112,
-0.349547177254573));
#56096=CARTESIAN_POINT('Ctrl Pts',(0.848836136151767,0.0523234930784053,
-0.339113214652093));
#56097=CARTESIAN_POINT('Ctrl Pts',(0.724153627343059,0.445939522912994,
-0.328679252049612));
#56098=CARTESIAN_POINT('Ctrl Pts',(0.428781301197015,0.734443414683686,
-0.318245289447131));
#56099=CARTESIAN_POINT('Ctrl Pts',(0.0323411916877275,0.849832090513251,
-0.307811326844651));
#56100=CARTESIAN_POINT('Ctrl Pts',(-0.371722040825158,0.764907351918338,
-0.29737736424217));
#56101=CARTESIAN_POINT('Ctrl Pts',(-0.688166893772684,0.499686763789953,
-0.28694340163969));
#56102=CARTESIAN_POINT('Ctrl Pts',(-0.84240434119643,0.116685300780245,
-0.276509439037209));
#56103=CARTESIAN_POINT('Ctrl Pts',(-0.798079165673271,-0.293819969988393,
-0.266075476434728));
#56104=CARTESIAN_POINT('Ctrl Pts',(-0.565639230046271,-0.635069140343272,
-0.255641513832248));
#56105=CARTESIAN_POINT('Ctrl Pts',(-0.199872807661195,-0.826626488317455,
-0.245207551229767));
#56106=CARTESIAN_POINT('Ctrl Pts',(0.213005508499063,-0.823340312573242,
-0.234773588627287));
#56107=CARTESIAN_POINT('Ctrl Pts',(0.575676435516455,-0.625984868845304,
-0.224339626024806));
#56108=CARTESIAN_POINT('Ctrl Pts',(0.802654992386151,-0.281079332570885,
-0.213905663422325));
#56109=CARTESIAN_POINT('Ctrl Pts',(0.840440266860436,0.130080080884035,
-0.203471700819845));
#56110=CARTESIAN_POINT('Ctrl Pts',(0.680125782303049,0.510576753259713,
-0.193037738217364));
#56111=CARTESIAN_POINT('Ctrl Pts',(0.359499429618295,0.770728914207573,
-0.182603775614884));
#56112=CARTESIAN_POINT('Ctrl Pts',(-0.0458646565737162,0.849206679729665,
-0.172169813012403));
#56113=CARTESIAN_POINT('Ctrl Pts',(-0.440417346097015,0.72753091896719,
-0.161735850409923));
#56114=CARTESIAN_POINT('Ctrl Pts',(-0.731160844709429,0.434344745947377,
-0.151301887807442));
#56115=CARTESIAN_POINT('Ctrl Pts',(-0.849560168473915,0.0388279800983555,
-0.140867925204961));
#56116=CARTESIAN_POINT('Ctrl Pts',(-0.767716584589533,-0.365940025647511,
-0.13043396260248));
#56117=CARTESIAN_POINT('Ctrl Pts',(-0.5924974211277,-0.578121984952227,
-0.12347798753416));
#56118=CARTESIAN_POINT('Ctrl Pts',(-0.485033396983243,-0.657408515958423,
-0.12));
#56119=CARTESIAN_POINT('Ctrl Pts',(0.546314451000137,0.52455872774923,-1.15727273924394));
#56120=CARTESIAN_POINT('Ctrl Pts',(0.459330425190867,0.615150357993711,
-1.15374460067508));
#56121=CARTESIAN_POINT('Ctrl Pts',(0.239517155169437,0.752140157504834,
-1.14668832353737));
#56122=CARTESIAN_POINT('Ctrl Pts',(-0.148496413265629,0.775239352992087,
-1.1361039078308));
#56123=CARTESIAN_POINT('Ctrl Pts',(-0.500415877733314,0.610427930590285,
-1.12551949212423));
#56124=CARTESIAN_POINT('Ctrl Pts',(-0.731074678445063,0.297631408040504,
-1.11493507641766));
#56125=CARTESIAN_POINT('Ctrl Pts',(-0.78448657507111,-0.0873109114175063,
-1.10435066071109));
#56126=CARTESIAN_POINT('Ctrl Pts',(-0.647739858405566,-0.451090008407739,
-1.09376624500452));
#56127=CARTESIAN_POINT('Ctrl Pts',(-0.35396552579895,-0.705517309450156,
-1.08318182929794));
#56128=CARTESIAN_POINT('Ctrl Pts',(0.0256119661671881,-0.788917676587972,
-1.07259741359137));
#56129=CARTESIAN_POINT('Ctrl Pts',(0.398982356900771,-0.681072808505694,
-1.0620129978848));
#56130=CARTESIAN_POINT('Ctrl Pts',(0.675632891112322,-0.40812628276753,
-1.05142858217823));
#56131=CARTESIAN_POINT('Ctrl Pts',(0.788500750688369,-0.0362440247522399,
-1.04084416647166));
#56132=CARTESIAN_POINT('Ctrl Pts',(0.710224521156417,0.344424265850664,
-1.03025975076509));
#56133=CARTESIAN_POINT('Ctrl Pts',(0.459779801870057,0.641599200064961,
-1.01967533505852));
#56134=CARTESIAN_POINT('Ctrl Pts',(0.097877817393331,0.783241287520996,
-1.00909091935195));
#56135=CARTESIAN_POINT('Ctrl Pts',(-0.287751124101878,0.735014472176637,
-0.998506503645378));
#56136=CARTESIAN_POINT('Ctrl Pts',(-0.603625085401645,0.508609617298406,
-0.987922087938805));
#56137=CARTESIAN_POINT('Ctrl Pts',(-0.773171671953705,0.158910506780707,
-0.977337672232237));
#56138=CARTESIAN_POINT('Ctrl Pts',(-0.755290373416537,-0.229310787602246,
-0.966753256525664));
#56139=CARTESIAN_POINT('Ctrl Pts',(-0.554315867123395,-0.561943861908008,
-0.956168840819094));
#56140=CARTESIAN_POINT('Ctrl Pts',(-0.218967255152568,-0.758353694545465,
-0.945584425112524));
#56141=CARTESIAN_POINT('Ctrl Pts',(0.169462156609868,-0.770927728297873,
-0.935000009405952));
#56142=CARTESIAN_POINT('Ctrl Pts',(0.516811513855876,-0.596617837396196,
-0.924415593699383));
#56143=CARTESIAN_POINT('Ctrl Pts',(0.738878357065632,-0.277679236275888,
-0.91383117799281));
#56144=CARTESIAN_POINT('Ctrl Pts',(0.781830502198587,0.108572789396219,
-0.903246762286241));
#56145=CARTESIAN_POINT('Ctrl Pts',(0.635255734092279,0.468505215644772,
-0.892662346579669));
#56146=CARTESIAN_POINT('Ctrl Pts',(0.334685876135465,0.714865266390365,
-0.882077930873099));
#56147=CARTESIAN_POINT('Ctrl Pts',(-0.0470166324849972,0.787931736286691,
-0.871493515166528));
#56148=CARTESIAN_POINT('Ctrl Pts',(-0.417321635893157,0.669992266368472,
-0.860909099459957));
#56149=CARTESIAN_POINT('Ctrl Pts',(-0.686461896723767,0.389637073600391,
-0.850324683753386));
#56150=CARTESIAN_POINT('Ctrl Pts',(-0.78919396038351,0.0148282727314064,
-0.839740268046816));
#56151=CARTESIAN_POINT('Ctrl Pts',(-0.700614103026785,-0.363575113859107,
-0.829155852340244));
#56152=CARTESIAN_POINT('Ctrl Pts',(-0.442195350963465,-0.65384268472174,
-0.818571436633674));
#56153=CARTESIAN_POINT('Ctrl Pts',(-0.0765821114814538,-0.785609422664232,
-0.807987020927103));
#56154=CARTESIAN_POINT('Ctrl Pts',(0.307595728844424,-0.726933182881658,
-0.797402605220531));
#56155=CARTESIAN_POINT('Ctrl Pts',(0.617207958261566,-0.492037926420706,
-0.786818189513963));
#56156=CARTESIAN_POINT('Ctrl Pts',(0.77720013723641,-0.137865628267142,
-0.776233773807389));
#56157=CARTESIAN_POINT('Ctrl Pts',(0.748787869734938,0.249727273071264,
-0.765649358100821));
#56158=CARTESIAN_POINT('Ctrl Pts',(0.538858696398575,0.576782706132406,
-0.755064942394248));
#56159=CARTESIAN_POINT('Ctrl Pts',(0.198302456030381,0.764017748949666,
-0.744480526687679));
#56160=CARTESIAN_POINT('Ctrl Pts',(-0.19032514031589,0.766043945045929,
-0.733896110981107));
#56161=CARTESIAN_POINT('Ctrl Pts',(-0.532815196286458,0.582370115462682,
-0.723311695274537));
#56162=CARTESIAN_POINT('Ctrl Pts',(-0.746143216224097,0.257521427575559,
-0.712727279567965));
#56163=CARTESIAN_POINT('Ctrl Pts',(-0.778595432221923,-0.129754143290109,
-0.702142863861395));
#56164=CARTESIAN_POINT('Ctrl Pts',(-0.622304962251659,-0.485575451124495,
-0.691558448154824));
#56165=CARTESIAN_POINT('Ctrl Pts',(-0.315158855058528,-0.723686313851513,
-0.680974032448254));
#56166=CARTESIAN_POINT('Ctrl Pts',(0.0683862731776896,-0.786365247463709,
-0.670389616741681));
#56167=CARTESIAN_POINT('Ctrl Pts',(0.435353589178266,-0.658417980592417,
-0.659805201035112));
#56168=CARTESIAN_POINT('Ctrl Pts',(0.696784958823668,-0.370860763541915,
-0.64922078532854));
#56169=CARTESIAN_POINT('Ctrl Pts',(0.789305673168617,0.00659841508485966,
-0.63863636962197));
#56170=CARTESIAN_POINT('Ctrl Pts',(0.690487385718296,0.382458043374312,
-0.6280519539154));
#56171=CARTESIAN_POINT('Ctrl Pts',(0.424285064899528,0.665604363327792,
-0.617467538208828));
#56172=CARTESIAN_POINT('Ctrl Pts',(0.0552299665647739,0.787398650983763,
-0.606883122502257));
#56173=CARTESIAN_POINT('Ctrl Pts',(-0.327213666821637,0.718316226339718,
-0.596298706795687));
#56174=CARTESIAN_POINT('Ctrl Pts',(-0.630336020111223,0.475103658718956,
-0.585714291089115));
#56175=CARTESIAN_POINT('Ctrl Pts',(-0.780655892709758,0.116719158475909,
-0.575129875382546));
#56176=CARTESIAN_POINT('Ctrl Pts',(-0.741733594202337,-0.269959737756351,
-0.564545459675974));
#56177=CARTESIAN_POINT('Ctrl Pts',(-0.52300444729998,-0.591196526446356,
-0.553961043969404));
#56178=CARTESIAN_POINT('Ctrl Pts',(-0.177491530455701,-0.76911880837377,
-0.543376628262832));
#56179=CARTESIAN_POINT('Ctrl Pts',(0.211047875895708,-0.760595673704304,
-0.532792212556262));
#56180=CARTESIAN_POINT('Ctrl Pts',(0.548426253918526,-0.567693252373749,
-0.522207796849691));
#56181=CARTESIAN_POINT('Ctrl Pts',(0.752858251913653,-0.237173854594711,
-0.511623381143121));
#56182=CARTESIAN_POINT('Ctrl Pts',(0.7747866251265,0.150839882998094,-0.501038965436549));
#56183=CARTESIAN_POINT('Ctrl Pts',(0.608895621771465,0.502287872206109,
-0.490454549729979));
#56184=CARTESIAN_POINT('Ctrl Pts',(0.295399597411609,0.731974086035053,
-0.479870134023407));
#56185=CARTESIAN_POINT('Ctrl Pts',(-0.0897055208909376,0.784219296051475,
-0.469285718316837));
#56186=CARTESIAN_POINT('Ctrl Pts',(-0.453064735918984,0.646358514947002,
-0.458701302610266));
#56187=CARTESIAN_POINT('Ctrl Pts',(-0.706594568913726,0.351811170884772,
-0.448116886903695));
#56188=CARTESIAN_POINT('Ctrl Pts',(-0.788835756602106,-0.028020240612635,
-0.437532471197125));
#56189=CARTESIAN_POINT('Ctrl Pts',(-0.679851857001812,-0.401059144402238,
-0.426948055490553));
#56190=CARTESIAN_POINT('Ctrl Pts',(-0.40606212854653,-0.676875566510097,
-0.416363639783983));
#56191=CARTESIAN_POINT('Ctrl Pts',(-0.033837123384323,-0.788607655212059,
-0.405779224077412));
#56192=CARTESIAN_POINT('Ctrl Pts',(0.346590485190783,-0.709169951669662,
-0.395194808370841));
#56193=CARTESIAN_POINT('Ctrl Pts',(0.642999595336517,-0.457819293150201,
-0.38461039266427));
#56194=CARTESIAN_POINT('Ctrl Pts',(0.78353639273709,-0.0954866798140887,
-0.3740259769577));
#56195=CARTESIAN_POINT('Ctrl Pts',(0.734132744595481,0.28999327252796,-0.363441561251129));
#56196=CARTESIAN_POINT('Ctrl Pts',(0.506764802819437,0.605174701533939,
-0.352857145544558));
#56197=CARTESIAN_POINT('Ctrl Pts',(0.156549813679528,0.773653113881338,
-0.342272729837987));
#56198=CARTESIAN_POINT('Ctrl Pts',(-0.231615093084919,0.754586929064552,
-0.331688314131416));
#56199=CARTESIAN_POINT('Ctrl Pts',(-0.563633182964234,0.552598063281491,
-0.321103898424845));
#56200=CARTESIAN_POINT('Ctrl Pts',(-0.759018516340423,0.216651511277527,
-0.310519482718275));
#56201=CARTESIAN_POINT('Ctrl Pts',(-0.770406886705707,-0.171814470849831,
-0.299935067011704));
#56202=CARTESIAN_POINT('Ctrl Pts',(-0.595037595541395,-0.518630163437193,
-0.289350651305133));
#56203=CARTESIAN_POINT('Ctrl Pts',(-0.275422660164443,-0.739722476337535,
-0.278766235598562));
#56204=CARTESIAN_POINT('Ctrl Pts',(0.11095865910622,-0.78149546229302,-0.268181819891991));
#56205=CARTESIAN_POINT('Ctrl Pts',(0.470442038027593,-0.63382275802318,
-0.257597404185421));
#56206=CARTESIAN_POINT('Ctrl Pts',(0.715883472822082,-0.332502328862262,
-0.24701298847885));
#56207=CARTESIAN_POINT('Ctrl Pts',(0.787784607225333,0.0494214101901834,
-0.236428572772279));
#56208=CARTESIAN_POINT('Ctrl Pts',(0.668715255345623,0.419364726111387,
-0.225844157065708));
#56209=CARTESIAN_POINT('Ctrl Pts',(0.387540164029785,0.687647957073743,
-0.215259741359137));
#56210=CARTESIAN_POINT('Ctrl Pts',(0.0124189653016963,0.789235606485636,
-0.204675325652567));
#56211=CARTESIAN_POINT('Ctrl Pts',(-0.365711157649466,0.699500976810326,
-0.194090909945995));
#56212=CARTESIAN_POINT('Ctrl Pts',(-0.655190820886885,0.440197805626207,
-0.183506494239425));
#56213=CARTESIAN_POINT('Ctrl Pts',(-0.785836630350135,0.0741833682121523,
-0.172922078532854));
#56214=CARTESIAN_POINT('Ctrl Pts',(-0.72599658874823,-0.309812190918401,
-0.162337662826283));
#56215=CARTESIAN_POINT('Ctrl Pts',(-0.490140575868292,-0.618708756217204,
-0.151753247119713));
#56216=CARTESIAN_POINT('Ctrl Pts',(-0.135514917188131,-0.777613622822956,
-0.141168831413141));
#56217=CARTESIAN_POINT('Ctrl Pts',(0.252058240770739,-0.748030699511335,
-0.130584415706571));
#56218=CARTESIAN_POINT('Ctrl Pts',(0.469550542503088,-0.607385125337185,
-0.123528138568857));
#56219=CARTESIAN_POINT('Ctrl Pts',(0.555007866453742,-0.515351924808608,
-0.12));
#56220=CARTESIAN_POINT('Ctrl Pts',(0.560643331187219,0.538316993061902,
-1.14693182616263));
#56221=CARTESIAN_POINT('Ctrl Pts',(0.471377865299383,0.631284684590043,
-1.14340368759377));
#56222=CARTESIAN_POINT('Ctrl Pts',(0.245799274584164,0.771867488863265,
-1.13634741045606));
#56223=CARTESIAN_POINT('Ctrl Pts',(-0.152391216542384,0.795572536170746,
-1.12576299474949));
#56224=CARTESIAN_POINT('Ctrl Pts',(-0.513540917978225,0.626438396109299,
-1.11517857904291));
#56225=CARTESIAN_POINT('Ctrl Pts',(-0.750249498836636,0.305437763479057,
-1.10459416333635));
#56226=CARTESIAN_POINT('Ctrl Pts',(-0.805062296840851,-0.089600925138424,
-1.09400974762977));
#56227=CARTESIAN_POINT('Ctrl Pts',(-0.664728951054495,-0.462921316681264,
-1.0834253319232));
#56228=CARTESIAN_POINT('Ctrl Pts',(-0.363249427405883,-0.724021804395359,
-1.07284091621663));
#56229=CARTESIAN_POINT('Ctrl Pts',(0.02628372360266,-0.809609618462481,
-1.06225650051006));
#56230=CARTESIAN_POINT('Ctrl Pts',(0.409446971882717,-0.698936166602649,
-1.05167208480349));
#56231=CARTESIAN_POINT('Ctrl Pts',(0.693353569614376,-0.418830727060134,
-1.04108766909692));
#56232=CARTESIAN_POINT('Ctrl Pts',(0.809181757319903,-0.0371946426376386,
-1.03050325339035));
#56233=CARTESIAN_POINT('Ctrl Pts',(0.728852478097603,0.353457916763361,
-1.01991883768378));
#56234=CARTESIAN_POINT('Ctrl Pts',(0.471839028349194,0.658427233899738,
-1.00933442197721));
#56235=CARTESIAN_POINT('Ctrl Pts',(0.100444982724277,0.803784347558887,
-0.998750006270635));
#56236=CARTESIAN_POINT('Ctrl Pts',(-0.295298336835141,0.754292626522196,
-0.988165590564065));
#56237=CARTESIAN_POINT('Ctrl Pts',(-0.619457124094383,0.521949565115867,
-0.977581174857493));
#56238=CARTESIAN_POINT('Ctrl Pts',(-0.793450623446181,0.163078453661776,
-0.966996759150924));
#56239=CARTESIAN_POINT('Ctrl Pts',(-0.775100329472666,-0.235325211703864,
-0.956412343444351));
#56240=CARTESIAN_POINT('Ctrl Pts',(-0.568854610572829,-0.576682674425973,
-0.945827927737782));
#56241=CARTESIAN_POINT('Ctrl Pts',(-0.224710386344195,-0.778243996199904,
-0.935243512031209));
#56242=CARTESIAN_POINT('Ctrl Pts',(0.173906854958707,-0.791147825041528,
-0.92465909632464));
#56243=CARTESIAN_POINT('Ctrl Pts',(0.530366583189641,-0.612266088131419,
-0.914074680618068));
#56244=CARTESIAN_POINT('Ctrl Pts',(0.75825785440794,-0.284962280866332,
-0.903490264911497));
#56245=CARTESIAN_POINT('Ctrl Pts',(0.802336559785202,0.111420465286886,
-0.892905849204928));
#56246=CARTESIAN_POINT('Ctrl Pts',(0.651917389820589,0.480793294588512,
-0.882321433498355));
#56247=CARTESIAN_POINT('Ctrl Pts',(0.343464105982166,0.733614942027284,
-0.871737017791786));
#56248=CARTESIAN_POINT('Ctrl Pts',(-0.0482497971806113,0.808597818657716,
-0.861152602085215));
#56249=CARTESIAN_POINT('Ctrl Pts',(-0.428267258344188,0.687565001070053,
-0.850568186378643));
#56250=CARTESIAN_POINT('Ctrl Pts',(-0.704466601254544,0.399856578015558,
-0.839983770672074));
#56251=CARTESIAN_POINT('Ctrl Pts',(-0.809893148702622,0.0152171925979065,
-0.829399354965502));
#56252=CARTESIAN_POINT('Ctrl Pts',(-0.718989995374629,-0.373111058288097,
-0.818814939258931));
#56253=CARTESIAN_POINT('Ctrl Pts',(-0.453793367804573,-0.670991843916459,
-0.80823052355236));
#56254=CARTESIAN_POINT('Ctrl Pts',(-0.0785907273946572,-0.806214594778186,
-0.79764610784579));
#56255=CARTESIAN_POINT('Ctrl Pts',(0.315663431129437,-0.745999379030152,
-0.787061692139218));
#56256=CARTESIAN_POINT('Ctrl Pts',(0.633396252142961,-0.504943227538543,
-0.776477276432649));
#56257=CARTESIAN_POINT('Ctrl Pts',(0.797584748383812,-0.141481604497939,
-0.765892860726076));
#56258=CARTESIAN_POINT('Ctrl Pts',(0.768427276401429,0.256277186163868,
-0.755308445019508));
#56259=CARTESIAN_POINT('Ctrl Pts',(0.552992025078288,0.591910715788788,
-0.744724029312934));
#56260=CARTESIAN_POINT('Ctrl Pts',(0.203503585394728,0.78405660892392,-0.734139613606365));
#56261=CARTESIAN_POINT('Ctrl Pts',(-0.19531703852979,0.786135948628312,
-0.723555197899793));
#56262=CARTESIAN_POINT('Ctrl Pts',(-0.546790014443781,0.59764467317157,
-0.712970782193224));
#56263=CARTESIAN_POINT('Ctrl Pts',(-0.765713258217505,0.264275767817853,
-0.702386366486652));
#56264=CARTESIAN_POINT('Ctrl Pts',(-0.79901663953594,-0.133157369343488,
-0.691801950780082));
#56265=CARTESIAN_POINT('Ctrl Pts',(-0.638626941704345,-0.498311252727788,
-0.68121753507351));
#56266=CARTESIAN_POINT('Ctrl Pts',(-0.323424925022017,-0.742667350258706,
-0.67063311936694));
#56267=CARTESIAN_POINT('Ctrl Pts',(0.0701799264720704,-0.806990243550786,
-0.660048703660369));
#56268=CARTESIAN_POINT('Ctrl Pts',(0.446772158478292,-0.675687141859628,
-0.649464287953798));
#56269=CARTESIAN_POINT('Ctrl Pts',(0.71506041936268,-0.380587797921389,
-0.638879872247228));
#56270=CARTESIAN_POINT('Ctrl Pts',(0.810007791520257,0.00677148006419926,
-0.628295456540657));
#56271=CARTESIAN_POINT('Ctrl Pts',(0.708597671841125,0.392489254282357,
-0.617711040834086));
#56272=CARTESIAN_POINT('Ctrl Pts',(0.435413326011757,0.683062010945685,
-0.607126625127516));
#56273=CARTESIAN_POINT('Ctrl Pts',(0.0566785527630608,0.808050751452203,
-0.596542209420943));
#56274=CARTESIAN_POINT('Ctrl Pts',(-0.335795913582415,0.737156414668648,
-0.585957793714374));
#56275=CARTESIAN_POINT('Ctrl Pts',(-0.646868640277576,0.48756480337615,
-0.575373378007802));
#56276=CARTESIAN_POINT('Ctrl Pts',(-0.801131142327445,0.11978049949348,
-0.564788962301232));
#56277=CARTESIAN_POINT('Ctrl Pts',(-0.761187979460866,-0.277040313294056,
-0.554204546594661));
#56278=CARTESIAN_POINT('Ctrl Pts',(-0.536721946533164,-0.606702585601409,
-0.54362013088809));
#56279=CARTESIAN_POINT('Ctrl Pts',(-0.18214682534945,-0.789291460286313,
-0.533035715181519));
#56280=CARTESIAN_POINT('Ctrl Pts',(0.216583295509653,-0.780544778582218,
-0.522451299474949));
#56281=CARTESIAN_POINT('Ctrl Pts',(0.56281052303215,-0.582582861428363,
-0.511866883768378));
#56282=CARTESIAN_POINT('Ctrl Pts',(0.772604417642525,-0.24339451330102,
-0.501282468061807));
#56283=CARTESIAN_POINT('Ctrl Pts',(0.795107934038734,0.154796151419981,
-0.490698052355236));
#56284=CARTESIAN_POINT('Ctrl Pts',(0.624865897488736,0.515462011618108,
-0.480113636648666));
#56285=CARTESIAN_POINT('Ctrl Pts',(0.303147416329586,0.751172496327227,
-0.469529220942094));
#56286=CARTESIAN_POINT('Ctrl Pts',(-0.0920583410636652,0.804788007556264,
-0.458944805235524));
#56287=CARTESIAN_POINT('Ctrl Pts',(-0.464947837868951,0.663311377353662,
-0.448360389528953));
#56288=CARTESIAN_POINT('Ctrl Pts',(-0.725127318505599,0.361038567500139,
-0.437775973822382));
#56289=CARTESIAN_POINT('Ctrl Pts',(-0.809525549857519,-0.0287551629084234,
-0.427191558115811));
#56290=CARTESIAN_POINT('Ctrl Pts',(-0.697683191659187,-0.411578229917095,
-0.416607142409241));
#56291=CARTESIAN_POINT('Ctrl Pts',(-0.416712433655251,-0.694628838231777,
-0.40602272670267));
#56292=CARTESIAN_POINT('Ctrl Pts',(-0.034724612422847,-0.80929146576377,
-0.395438310996099));
#56293=CARTESIAN_POINT('Ctrl Pts',(0.355680952278354,-0.727770249082901,
-0.384853895289528));
#56294=CARTESIAN_POINT('Ctrl Pts',(0.659864359109563,-0.469827098887125,
-0.374269479582957));
#56295=CARTESIAN_POINT('Ctrl Pts',(0.804087192872789,-0.0979911297549861,
-0.363685063876387));
#56296=CARTESIAN_POINT('Ctrl Pts',(0.753387772756394,0.297599292924283,
-0.353100648169815));
#56297=CARTESIAN_POINT('Ctrl Pts',(0.520056364353892,0.621047383969223,
-0.342516232463245));
#56298=CARTESIAN_POINT('Ctrl Pts',(0.160655843676387,0.793944692760268,
-0.331931816756674));
#56299=CARTESIAN_POINT('Ctrl Pts',(-0.237689955121348,0.774378434995814,
-0.321347401050103));
#56300=CARTESIAN_POINT('Ctrl Pts',(-0.578416303442509,0.567091751716565,
-0.310762985343532));
#56301=CARTESIAN_POINT('Ctrl Pts',(-0.778926255117071,0.222333904525157,
-0.300178569636961));
#56302=CARTESIAN_POINT('Ctrl Pts',(-0.790613322678065,-0.176320866319888,
-0.289594153930391));
#56303=CARTESIAN_POINT('Ctrl Pts',(-0.610644399274507,-0.532232932794095,
-0.27900973822382));
#56304=CARTESIAN_POINT('Ctrl Pts',(-0.282646518678672,-0.759124113463787,
-0.268425322517249));
#56305=CARTESIAN_POINT('Ctrl Pts',(0.113868912219864,-0.801992732364211,
-0.257840906810678));
#56306=CARTESIAN_POINT('Ctrl Pts',(0.482780916462025,-0.65044682927543,
-0.247256491104107));
#56307=CARTESIAN_POINT('Ctrl Pts',(0.734659854247102,-0.34122328805247,
-0.236672075397537));
#56308=CARTESIAN_POINT('Ctrl Pts',(0.808446830656353,0.0507176480326844,
-0.226087659690966));
#56309=CARTESIAN_POINT('Ctrl Pts',(0.686254496263704,0.430363935274053,
-0.215503243984395));
#56310=CARTESIAN_POINT('Ctrl Pts',(0.39770467014508,0.705683769909671,-0.204918828277824));
#56311=CARTESIAN_POINT('Ctrl Pts',(0.0127446932144949,0.809935887109748,
-0.194334412571253));
#56312=CARTESIAN_POINT('Ctrl Pts',(-0.375303126801014,0.717847673788803,
-0.183749996864682));
#56313=CARTESIAN_POINT('Ctrl Pts',(-0.672375339354181,0.451743430318885,
-0.173165581158112));
#56314=CARTESIAN_POINT('Ctrl Pts',(-0.806447761727482,0.0761290692512524,
-0.162581165451541));
#56315=CARTESIAN_POINT('Ctrl Pts',(-0.745038219657606,-0.317938027158024,
-0.15199674974497));
#56316=CARTESIAN_POINT('Ctrl Pts',(-0.502996112773066,-0.634936413425072,
-0.141412334038399));
#56317=CARTESIAN_POINT('Ctrl Pts',(-0.139069238345838,-0.798009078979888,
-0.130827918331828));
#56318=CARTESIAN_POINT('Ctrl Pts',(0.258669291101841,-0.76765024691656,
-0.120243502625258));
#56319=CARTESIAN_POINT('Ctrl Pts',(0.481866038556668,-0.623315783353716,
-0.113187225487544));
#56320=CARTESIAN_POINT('Ctrl Pts',(0.569564759844983,-0.52886871165407,
-0.109659086918687));
#56321=CARTESIAN_POINT('Ctrl Pts',(0.574972211374301,0.552075258374573,
-1.13659091308131));
#56322=CARTESIAN_POINT('Ctrl Pts',(0.4834253054079,0.647419011186374,-1.13306277451246));
#56323=CARTESIAN_POINT('Ctrl Pts',(0.25208139399889,0.791594820221696,-1.12600649737474));
#56324=CARTESIAN_POINT('Ctrl Pts',(-0.15628601981914,0.815905719349405,
-1.11542208166817));
#56325=CARTESIAN_POINT('Ctrl Pts',(-0.526665958223137,0.642448861628311,
-1.1048376659616));
#56326=CARTESIAN_POINT('Ctrl Pts',(-0.769424319228209,0.31324411891761,
-1.09425325025503));
#56327=CARTESIAN_POINT('Ctrl Pts',(-0.825638018610592,-0.0918909388593417,
-1.08366883454846));
#56328=CARTESIAN_POINT('Ctrl Pts',(-0.681718043703425,-0.474752624954789,
-1.07308441884189));
#56329=CARTESIAN_POINT('Ctrl Pts',(-0.372533329012816,-0.742526299340561,
-1.06250000313532));
#56330=CARTESIAN_POINT('Ctrl Pts',(0.0269554810381316,-0.830301560336992,
-1.05191558742875));
#56331=CARTESIAN_POINT('Ctrl Pts',(0.419911586864664,-0.716799524699605,
-1.04133117172218));
#56332=CARTESIAN_POINT('Ctrl Pts',(0.711074248116431,-0.429535171352737,
-1.0307467560156));
#56333=CARTESIAN_POINT('Ctrl Pts',(0.829862763951438,-0.0381452605230374,
-1.02016234030904));
#56334=CARTESIAN_POINT('Ctrl Pts',(0.747480435038788,0.362491567676058,
-1.00957792460246));
#56335=CARTESIAN_POINT('Ctrl Pts',(0.483898254828331,0.675255267734517,
-0.998993508895893));
#56336=CARTESIAN_POINT('Ctrl Pts',(0.103012148055223,0.824327407596778,
-0.988409093189322));
#56337=CARTESIAN_POINT('Ctrl Pts',(-0.302845549568404,0.773570780867756,
-0.977824677482752));
#56338=CARTESIAN_POINT('Ctrl Pts',(-0.635289162787122,0.535289512933327,
-0.96724026177618));
#56339=CARTESIAN_POINT('Ctrl Pts',(-0.813729574938656,0.167246400542847,
-0.95665584606961));
#56340=CARTESIAN_POINT('Ctrl Pts',(-0.794910285528796,-0.241339635805483,
-0.946071430363038));
#56341=CARTESIAN_POINT('Ctrl Pts',(-0.583393354022263,-0.591421486943936,
-0.935487014656468));
#56342=CARTESIAN_POINT('Ctrl Pts',(-0.230453517535823,-0.798134297854346,
-0.924902598949897));
#56343=CARTESIAN_POINT('Ctrl Pts',(0.178351553307546,-0.811367921785181,
-0.914318183243326));
#56344=CARTESIAN_POINT('Ctrl Pts',(0.543921652523406,-0.627914338866642,
-0.903733767536756));
#56345=CARTESIAN_POINT('Ctrl Pts',(0.777637351750247,-0.292245325456775,
-0.893149351830184));
#56346=CARTESIAN_POINT('Ctrl Pts',(0.822842617371817,0.114268141177551,
-0.882564936123615));
#56347=CARTESIAN_POINT('Ctrl Pts',(0.6685790455489,0.493081373532255,-0.871980520417042));
#56348=CARTESIAN_POINT('Ctrl Pts',(0.352242335828867,0.7523646176642,-0.861396104710473));
#56349=CARTESIAN_POINT('Ctrl Pts',(-0.0494829618762249,0.829263901028745,
-0.850811689003901));
#56350=CARTESIAN_POINT('Ctrl Pts',(-0.439212880795219,0.705137735771633,
-0.840227273297331));
#56351=CARTESIAN_POINT('Ctrl Pts',(-0.72247130578532,0.410076082430725,
-0.829642857590759));
#56352=CARTESIAN_POINT('Ctrl Pts',(-0.830592337021733,0.0156061124644064,
-0.81905844188419));
#56353=CARTESIAN_POINT('Ctrl Pts',(-0.737365887722473,-0.382647002717086,
-0.808474026177617));
#56354=CARTESIAN_POINT('Ctrl Pts',(-0.465391384645681,-0.688141003111179,
-0.797889610471048));
#56355=CARTESIAN_POINT('Ctrl Pts',(-0.0805993433078604,-0.826819766892139,
-0.787305194764476));
#56356=CARTESIAN_POINT('Ctrl Pts',(0.32373113341445,-0.765065575178645,
-0.776720779057906));
#56357=CARTESIAN_POINT('Ctrl Pts',(0.649584546024354,-0.51784852865638,
-0.766136363351335));
#56358=CARTESIAN_POINT('Ctrl Pts',(0.817969359531213,-0.145097580728735,
-0.755551947644763));
#56359=CARTESIAN_POINT('Ctrl Pts',(0.788066683067918,0.262827099256472,
-0.744967531938194));
#56360=CARTESIAN_POINT('Ctrl Pts',(0.567125353758002,0.607038725445171,
-0.734383116231622));
#56361=CARTESIAN_POINT('Ctrl Pts',(0.208704714759074,0.804095468898175,
-0.723798700525051));
#56362=CARTESIAN_POINT('Ctrl Pts',(-0.20030893674369,0.806227952210694,
-0.713214284818481));
#56363=CARTESIAN_POINT('Ctrl Pts',(-0.560764832601105,0.612919230880461,
-0.702629869111909));
#56364=CARTESIAN_POINT('Ctrl Pts',(-0.785283300210914,0.271030108060145,
-0.69204545340534));
#56365=CARTESIAN_POINT('Ctrl Pts',(-0.819437846849956,-0.136560595396867,
-0.681461037698767));
#56366=CARTESIAN_POINT('Ctrl Pts',(-0.654948921157034,-0.511047054331084,
-0.670876621992198));
#56367=CARTESIAN_POINT('Ctrl Pts',(-0.331690994985504,-0.761648386665898,
-0.660292206285627));
#56368=CARTESIAN_POINT('Ctrl Pts',(0.0719735797664497,-0.827615239637865,
-0.649707790579055));
#56369=CARTESIAN_POINT('Ctrl Pts',(0.458190727778319,-0.692956303126838,
-0.639123374872485));
#56370=CARTESIAN_POINT('Ctrl Pts',(0.733335879901691,-0.390314832300863,
-0.628538959165914));
#56371=CARTESIAN_POINT('Ctrl Pts',(0.830709909871899,0.00694454504353916,
-0.617954543459344));
#56372=CARTESIAN_POINT('Ctrl Pts',(0.726707957963954,0.402520465190403,
-0.607370127752772));
#56373=CARTESIAN_POINT('Ctrl Pts',(0.446541587123986,0.700519658563577,
-0.596785712046202));
#56374=CARTESIAN_POINT('Ctrl Pts',(0.0581271389613474,0.828702851920643,
-0.586201296339631));
#56375=CARTESIAN_POINT('Ctrl Pts',(-0.344378160343194,0.755996602997577,
-0.575616880633061));
#56376=CARTESIAN_POINT('Ctrl Pts',(-0.66340126044393,0.500025948033344,
-0.565032464926489));
#56377=CARTESIAN_POINT('Ctrl Pts',(-0.821606391945131,0.122841840511051,
-0.554448049219919));
#56378=CARTESIAN_POINT('Ctrl Pts',(-0.780642364719396,-0.284120888831762,
-0.543863633513348));
#56379=CARTESIAN_POINT('Ctrl Pts',(-0.55043944576635,-0.622208644756461,
-0.533279217806777));
#56380=CARTESIAN_POINT('Ctrl Pts',(-0.186802120243198,-0.809464112198859,
-0.522694802100206));
#56381=CARTESIAN_POINT('Ctrl Pts',(0.222118715123597,-0.800493883460131,
-0.512110386393635));
#56382=CARTESIAN_POINT('Ctrl Pts',(0.577194792145775,-0.597472470482978,
-0.501525970687065));
#56383=CARTESIAN_POINT('Ctrl Pts',(0.792350583371397,-0.249615172007328,
-0.490941554980493));
#56384=CARTESIAN_POINT('Ctrl Pts',(0.815429242950966,0.158752419841869,
-0.480357139273923));
#56385=CARTESIAN_POINT('Ctrl Pts',(0.640836173206008,0.528636151030106,
-0.469772723567352));
#56386=CARTESIAN_POINT('Ctrl Pts',(0.310895235247563,0.770370906619402,
-0.459188307860781));
#56387=CARTESIAN_POINT('Ctrl Pts',(-0.0944111612363924,0.825356719061053,
-0.44860389215421));
#56388=CARTESIAN_POINT('Ctrl Pts',(-0.476830939818917,0.680264239760323,
-0.43801947644764));
#56389=CARTESIAN_POINT('Ctrl Pts',(-0.743660068097472,0.370265964115506,
-0.427435060741068));
#56390=CARTESIAN_POINT('Ctrl Pts',(-0.830215343112932,-0.0294900852042113,
-0.416850645034498));
#56391=CARTESIAN_POINT('Ctrl Pts',(-0.715514526316563,-0.422097315431953,
-0.406266229327927));
#56392=CARTESIAN_POINT('Ctrl Pts',(-0.427362738763972,-0.712382109953456,
-0.395681813621356));
#56393=CARTESIAN_POINT('Ctrl Pts',(-0.0356121014613704,-0.829975276315482,
-0.385097397914786));
#56394=CARTESIAN_POINT('Ctrl Pts',(0.364771419365924,-0.746370546496139,
-0.374512982208215));
#56395=CARTESIAN_POINT('Ctrl Pts',(0.676729122882608,-0.481834904624049,
-0.363928566501644));
#56396=CARTESIAN_POINT('Ctrl Pts',(0.824637993008488,-0.100495579695883,
-0.353344150795073));
#56397=CARTESIAN_POINT('Ctrl Pts',(0.772642800917309,0.305205313320604,
-0.342759735088502));
#56398=CARTESIAN_POINT('Ctrl Pts',(0.533347925888346,0.63692006640451,-0.332175319381932));
#56399=CARTESIAN_POINT('Ctrl Pts',(0.164761873673246,0.814236271639195,
-0.321590903675361));
#56400=CARTESIAN_POINT('Ctrl Pts',(-0.243764817157777,0.794169940927079,
-0.311006487968789));
#56401=CARTESIAN_POINT('Ctrl Pts',(-0.593199423920784,0.581585440151637,
-0.300422072262219));
#56402=CARTESIAN_POINT('Ctrl Pts',(-0.798833993893717,0.228016297772788,
-0.289837656555648));
#56403=CARTESIAN_POINT('Ctrl Pts',(-0.810819758650425,-0.180827261789946,
-0.279253240849078));
#56404=CARTESIAN_POINT('Ctrl Pts',(-0.626251203007618,-0.545835702150998,
-0.268668825142506));
#56405=CARTESIAN_POINT('Ctrl Pts',(-0.289870377192901,-0.778525750590038,
-0.258084409435936));
#56406=CARTESIAN_POINT('Ctrl Pts',(0.116779165333508,-0.822490002435403,
-0.247499993729365));
#56407=CARTESIAN_POINT('Ctrl Pts',(0.495119794896455,-0.667070900527678,
-0.236915578022794));
#56408=CARTESIAN_POINT('Ctrl Pts',(0.753436235672123,-0.349944247242678,
-0.226331162316223));
#56409=CARTESIAN_POINT('Ctrl Pts',(0.829109054087371,0.0520138858751856,
-0.215746746609652));
#56410=CARTESIAN_POINT('Ctrl Pts',(0.703793737181786,0.44136314443672,-0.205162330903082));
#56411=CARTESIAN_POINT('Ctrl Pts',(0.407869176260375,0.723719582745598,
-0.194577915196511));
#56412=CARTESIAN_POINT('Ctrl Pts',(0.0130704211272931,0.830636167733862,
-0.18399349948994));
#56413=CARTESIAN_POINT('Ctrl Pts',(-0.384895095952561,0.736194370767277,
-0.173409083783369));
#56414=CARTESIAN_POINT('Ctrl Pts',(-0.689559857821479,0.463289055011564,
-0.162824668076798));
#56415=CARTESIAN_POINT('Ctrl Pts',(-0.827058893104828,0.0780747702903524,
-0.152240252370228));
#56416=CARTESIAN_POINT('Ctrl Pts',(-0.764079850566983,-0.326063863397647,
-0.141655836663657));
#56417=CARTESIAN_POINT('Ctrl Pts',(-0.515851649677841,-0.651164070632938,
-0.131071420957086));
#56418=CARTESIAN_POINT('Ctrl Pts',(-0.142623559503546,-0.818404535136822,
-0.120487005250515));
#56419=CARTESIAN_POINT('Ctrl Pts',(0.265280341432943,-0.787269794321785,
-0.109902589543944));
#56420=CARTESIAN_POINT('Ctrl Pts',(0.494181534610247,-0.639246441370247,
-0.10284631240623));
#56421=CARTESIAN_POINT('Ctrl Pts',(0.584121653236224,-0.542385498499533,
-0.0993181738373734));
#56422=CARTESIAN_POINT('Ctrl Pts',(0.589301091561382,0.565833523687245,
-1.12625));
#56423=CARTESIAN_POINT('Ctrl Pts',(0.495472745516417,0.663553337782706,
-1.12272186143114));
#56424=CARTESIAN_POINT('Ctrl Pts',(0.258363513413617,0.811322151580129,
-1.11566558429343));
#56425=CARTESIAN_POINT('Ctrl Pts',(-0.160180823095895,0.836238902528063,
-1.10508116858686));
#56426=CARTESIAN_POINT('Ctrl Pts',(-0.539790998468049,0.658459327147326,
-1.09449675288029));
#56427=CARTESIAN_POINT('Ctrl Pts',(-0.788599139619781,0.321050474356163,
-1.08391233717372));
#56428=CARTESIAN_POINT('Ctrl Pts',(-0.846213740380333,-0.0941809525802601,
-1.07332792146715));
#56429=CARTESIAN_POINT('Ctrl Pts',(-0.698707136352355,-0.486583933228312,
-1.06274350576058));
#56430=CARTESIAN_POINT('Ctrl Pts',(-0.381817230619748,-0.761030794285765,
-1.052159090054));
#56431=CARTESIAN_POINT('Ctrl Pts',(0.0276272384736035,-0.8509935022115,
-1.04157467434743));
#56432=CARTESIAN_POINT('Ctrl Pts',(0.430376201846611,-0.734662882796562,
-1.03099025864086));
#56433=CARTESIAN_POINT('Ctrl Pts',(0.728794926618486,-0.44023961564534,
-1.02040584293429));
#56434=CARTESIAN_POINT('Ctrl Pts',(0.850543770582973,-0.0390958784084376,
-1.00982142722772));
#56435=CARTESIAN_POINT('Ctrl Pts',(0.766108391979974,0.371525218588757,
-0.99923701152115));
#56436=CARTESIAN_POINT('Ctrl Pts',(0.495957481307468,0.692083301569292,
-0.988652595814579));
#56437=CARTESIAN_POINT('Ctrl Pts',(0.10557931338617,0.844870467634672,-0.978068180108009));
#56438=CARTESIAN_POINT('Ctrl Pts',(-0.310392762301666,0.792848935213314,
-0.967483764401438));
#56439=CARTESIAN_POINT('Ctrl Pts',(-0.651121201479862,0.548629460750789,
-0.956899348694867));
#56440=CARTESIAN_POINT('Ctrl Pts',(-0.834008526431131,0.171414347423916,
-0.946314932988296));
#56441=CARTESIAN_POINT('Ctrl Pts',(-0.814720241584927,-0.247354059907101,
-0.935730517281725));
#56442=CARTESIAN_POINT('Ctrl Pts',(-0.597932097471697,-0.6061602994619,
-0.925146101575155));
#56443=CARTESIAN_POINT('Ctrl Pts',(-0.23619664872745,-0.818024599508785,
-0.914561685868583));
#56444=CARTESIAN_POINT('Ctrl Pts',(0.182796251656384,-0.831588018528836,
-0.903977270162014));
#56445=CARTESIAN_POINT('Ctrl Pts',(0.557476721857172,-0.643562589601865,
-0.893392854455442));
#56446=CARTESIAN_POINT('Ctrl Pts',(0.797016849092552,-0.299528370047219,
-0.882808438748871));
#56447=CARTESIAN_POINT('Ctrl Pts',(0.843348674958435,0.117115817068216,
-0.872224023042301));
#56448=CARTESIAN_POINT('Ctrl Pts',(0.685240701277209,0.505369452475996,
-0.86163960733573));
#56449=CARTESIAN_POINT('Ctrl Pts',(0.361020565675569,0.771114293301118,
-0.851055191629159));
#56450=CARTESIAN_POINT('Ctrl Pts',(-0.0507161265718399,0.849929983399771,
-0.840470775922588));
#56451=CARTESIAN_POINT('Ctrl Pts',(-0.450158503246249,0.722710470473214,
-0.829886360216016));
#56452=CARTESIAN_POINT('Ctrl Pts',(-0.740476010316099,0.420295586845891,
-0.819301944509447));
#56453=CARTESIAN_POINT('Ctrl Pts',(-0.851291525340843,0.0159950323309065,
-0.808717528802875));
#56454=CARTESIAN_POINT('Ctrl Pts',(-0.755741780070319,-0.392182947146076,
-0.798133113096306));
#56455=CARTESIAN_POINT('Ctrl Pts',(-0.476989401486788,-0.705290162305898,
-0.787548697389734));
#56456=CARTESIAN_POINT('Ctrl Pts',(-0.0826079592210633,-0.847424939006094,
-0.776964281683164));
#56457=CARTESIAN_POINT('Ctrl Pts',(0.331798835699463,-0.784131771327138,
-0.766379865976592));
#56458=CARTESIAN_POINT('Ctrl Pts',(0.66577283990575,-0.530753829774217,
-0.755795450270022));
#56459=CARTESIAN_POINT('Ctrl Pts',(0.838353970678613,-0.148713556959531,
-0.74521103456345));
#56460=CARTESIAN_POINT('Ctrl Pts',(0.807706089734409,0.269377012349076,
-0.73462661885688));
#56461=CARTESIAN_POINT('Ctrl Pts',(0.581258682437715,0.622166735101554,
-0.72404220315031));
#56462=CARTESIAN_POINT('Ctrl Pts',(0.213905844123421,0.824134328872429,
-0.713457787443737));
#56463=CARTESIAN_POINT('Ctrl Pts',(-0.205300834957591,0.826319955793078,
-0.702873371737168));
#56464=CARTESIAN_POINT('Ctrl Pts',(-0.574739650758427,0.628193788589349,
-0.692288956030596));
#56465=CARTESIAN_POINT('Ctrl Pts',(-0.804853342204323,0.277784448302439,
-0.681704540324026));
#56466=CARTESIAN_POINT('Ctrl Pts',(-0.839859054163972,-0.139963821450246,
-0.671120124617455));
#56467=CARTESIAN_POINT('Ctrl Pts',(-0.67127090060972,-0.523782855934378,
-0.660535708910885));
#56468=CARTESIAN_POINT('Ctrl Pts',(-0.339957064948993,-0.780629423073091,
-0.649951293204313));
#56469=CARTESIAN_POINT('Ctrl Pts',(0.0737672330608303,-0.848240235724942,
-0.639366877497742));
#56470=CARTESIAN_POINT('Ctrl Pts',(0.469609297078345,-0.71022546439405,
-0.628782461791172));
#56471=CARTESIAN_POINT('Ctrl Pts',(0.751611340440703,-0.400041866680337,
-0.6181980460846));
#56472=CARTESIAN_POINT('Ctrl Pts',(0.85141202822354,0.00711761002287854,
-0.60761363037803));
#56473=CARTESIAN_POINT('Ctrl Pts',(0.744818244086783,0.41255167609845,-0.597029214671459));
#56474=CARTESIAN_POINT('Ctrl Pts',(0.457669848236215,0.717977306181469,
-0.586444798964888));
#56475=CARTESIAN_POINT('Ctrl Pts',(0.0595757251596351,0.849354952389083,
-0.575860383258318));
#56476=CARTESIAN_POINT('Ctrl Pts',(-0.352960407103974,0.774836791326507,
-0.565275967551747));
#56477=CARTESIAN_POINT('Ctrl Pts',(-0.679933880610282,0.512487092690538,
-0.554691551845177));
#56478=CARTESIAN_POINT('Ctrl Pts',(-0.842081641562818,0.125903181528622,
-0.544107136138605));
#56479=CARTESIAN_POINT('Ctrl Pts',(-0.800096749977925,-0.291201464369467,
-0.533522720432035));
#56480=CARTESIAN_POINT('Ctrl Pts',(-0.564156944999535,-0.637714703911514,
-0.522938304725464));
#56481=CARTESIAN_POINT('Ctrl Pts',(-0.191457415136946,-0.829636764111403,
-0.512353889018893));
#56482=CARTESIAN_POINT('Ctrl Pts',(0.227654134737541,-0.820442988338044,
-0.501769473312322));
#56483=CARTESIAN_POINT('Ctrl Pts',(0.591579061259401,-0.612362079537592,
-0.491185057605751));
#56484=CARTESIAN_POINT('Ctrl Pts',(0.812096749100268,-0.255835830713636,
-0.48060064189918));
#56485=CARTESIAN_POINT('Ctrl Pts',(0.8357505518632,0.162708688263756,-0.47001622619261));
#56486=CARTESIAN_POINT('Ctrl Pts',(0.656806448923279,0.541810290442105,
-0.459431810486038));
#56487=CARTESIAN_POINT('Ctrl Pts',(0.318643054165541,0.789569316911576,
-0.448847394779468));
#56488=CARTESIAN_POINT('Ctrl Pts',(-0.0967639814091197,0.845925430565842,
-0.438262979072897));
#56489=CARTESIAN_POINT('Ctrl Pts',(-0.488714041768884,0.697217102166983,
-0.427678563366326));
#56490=CARTESIAN_POINT('Ctrl Pts',(-0.762192817689344,0.379493360730874,
-0.417094147659756));
#56491=CARTESIAN_POINT('Ctrl Pts',(-0.850905136368346,-0.0302250075,-0.406509731953184));
#56492=CARTESIAN_POINT('Ctrl Pts',(-0.733345860973939,-0.43261640094681,
-0.395925316246614));
#56493=CARTESIAN_POINT('Ctrl Pts',(-0.438013043872693,-0.730135381675136,
-0.385340900540043));
#56494=CARTESIAN_POINT('Ctrl Pts',(-0.0364995904998943,-0.850659086867193,
-0.374756484833472));
#56495=CARTESIAN_POINT('Ctrl Pts',(0.373861886453494,-0.764970843909378,
-0.364172069126902));
#56496=CARTESIAN_POINT('Ctrl Pts',(0.693593886655655,-0.493842710360973,
-0.35358765342033));
#56497=CARTESIAN_POINT('Ctrl Pts',(0.845188793144186,-0.10300002963678,
-0.34300323771376));
#56498=CARTESIAN_POINT('Ctrl Pts',(0.791897829078223,0.312811333716926,
-0.332418822007189));
#56499=CARTESIAN_POINT('Ctrl Pts',(0.5466394874228,0.652792748839794,-0.321834406300618));
#56500=CARTESIAN_POINT('Ctrl Pts',(0.168867903670105,0.834527850518125,
-0.311249990594047));
#56501=CARTESIAN_POINT('Ctrl Pts',(-0.249839679194206,0.813961446858341,
-0.300665574887477));
#56502=CARTESIAN_POINT('Ctrl Pts',(-0.607982544399059,0.59607912858671,
-0.290081159180906));
#56503=CARTESIAN_POINT('Ctrl Pts',(-0.818741732670364,0.233698691020418,
-0.279496743474335));
#56504=CARTESIAN_POINT('Ctrl Pts',(-0.831026194622783,-0.185333657260002,
-0.268912327767764));
#56505=CARTESIAN_POINT('Ctrl Pts',(-0.64185800674073,-0.559438471507901,
-0.258327912061193));
#56506=CARTESIAN_POINT('Ctrl Pts',(-0.29709423570713,-0.797927387716288,
-0.247743496354622));
#56507=CARTESIAN_POINT('Ctrl Pts',(0.119689418447152,-0.842987272506594,
-0.237159080648052));
#56508=CARTESIAN_POINT('Ctrl Pts',(0.507458673330886,-0.683694971779928,
-0.226574664941481));
#56509=CARTESIAN_POINT('Ctrl Pts',(0.772212617097144,-0.358665206432886,
-0.21599024923491));
#56510=CARTESIAN_POINT('Ctrl Pts',(0.849771277518388,0.0533101237176862,
-0.205405833528339));
#56511=CARTESIAN_POINT('Ctrl Pts',(0.721332978099869,0.452362353599387,
-0.194821417821768));
#56512=CARTESIAN_POINT('Ctrl Pts',(0.41803368237567,0.741755395581526,-0.184237002115198));
#56513=CARTESIAN_POINT('Ctrl Pts',(0.0133961490400916,0.851336448357975,
-0.173652586408627));
#56514=CARTESIAN_POINT('Ctrl Pts',(-0.394487065104108,0.754541067745753,
-0.163068170702056));
#56515=CARTESIAN_POINT('Ctrl Pts',(-0.706744376288777,0.474834679704242,
-0.152483754995485));
#56516=CARTESIAN_POINT('Ctrl Pts',(-0.847670024482175,0.0800204713294527,
-0.141899339288914));
#56517=CARTESIAN_POINT('Ctrl Pts',(-0.783121481476359,-0.334189699637271,
-0.131314923582344));
#56518=CARTESIAN_POINT('Ctrl Pts',(-0.528707186582616,-0.667391727840805,
-0.120730507875773));
#56519=CARTESIAN_POINT('Ctrl Pts',(-0.146177880661253,-0.838799991293755,
-0.110146092169202));
#56520=CARTESIAN_POINT('Ctrl Pts',(0.271891391764045,-0.80688934172701,
-0.0995616764626311));
#56521=CARTESIAN_POINT('Ctrl Pts',(0.506497030663827,-0.655177099386778,
-0.0925053993249171));
#56522=CARTESIAN_POINT('Ctrl Pts',(0.598678546627464,-0.555902285344995,
-0.0889772607560602));
#56523=CARTESIAN_POINT('',(0.555007866453742,-0.515351924808608,-0.12));
#56524=CARTESIAN_POINT('Ctrl Pts',(-0.485074560134029,-0.65745190369334,
-0.12));
#56525=CARTESIAN_POINT('Ctrl Pts',(-0.453585509292985,-0.678311536271589,
-0.12));
#56526=CARTESIAN_POINT('Ctrl Pts',(-0.420738538427663,-0.696888835579881,
-0.12));
#56527=CARTESIAN_POINT('Ctrl Pts',(-0.386803943986794,-0.71311112212273,
-0.12));
#56528=CARTESIAN_POINT('Ctrl Pts',(-0.352869989072943,-0.729333102942445,
-0.12));
#56529=CARTESIAN_POINT('Ctrl Pts',(-0.317847265091438,-0.743200535649333,
-0.12));
#56530=CARTESIAN_POINT('Ctrl Pts',(-0.281986661942266,-0.754592743143696,
-0.12));
#56531=CARTESIAN_POINT('Ctrl Pts',(-0.255949172785094,-0.762864340748367,
-0.12));
#56532=CARTESIAN_POINT('Ctrl Pts',(-0.229469505293985,-0.7698300648233,
-0.12));
#56533=CARTESIAN_POINT('Ctrl Pts',(-0.202642618159761,-0.775426102639775,
-0.12));
#56534=CARTESIAN_POINT('Ctrl Pts',(-0.195274171519276,-0.776963146645012,
-0.12));
#56535=CARTESIAN_POINT('Ctrl Pts',(-0.187880255141526,-0.778396492216609,
-0.12));
#56536=CARTESIAN_POINT('Ctrl Pts',(-0.18047576779481,-0.779722738931636,
-0.12));
#56537=CARTESIAN_POINT('Ctrl Pts',(-0.166033419362242,-0.782309564496876,
-0.12));
#56538=CARTESIAN_POINT('Ctrl Pts',(-0.151538081932198,-0.784491790553693,
-0.12));
#56539=CARTESIAN_POINT('Ctrl Pts',(-0.137004865545485,-0.786263720842401,
-0.12));
#56540=CARTESIAN_POINT('Ctrl Pts',(-0.100095238310147,-0.790763845570678,
-0.12));
#56541=CARTESIAN_POINT('Ctrl Pts',(-0.0629412165342028,-0.792621345331591,
-0.12));
#56542=CARTESIAN_POINT('Ctrl Pts',(-0.0258198641282066,-0.791883010674466,
-0.12));
#56543=CARTESIAN_POINT('Ctrl Pts',(0.00402572525169566,-0.791289389171658,
-0.12));
#56544=CARTESIAN_POINT('Ctrl Pts',(0.0338506107991278,-0.789016694488355,
-0.12));
#56545=CARTESIAN_POINT('Ctrl Pts',(0.0635063571289652,-0.78506522308076,
-0.12));
#56546=CARTESIAN_POINT('Ctrl Pts',(0.0773427424639829,-0.78322159788827,
-0.12));
#56547=CARTESIAN_POINT('Ctrl Pts',(0.0911422070269432,-0.781012233182779,
-0.12));
#56548=CARTESIAN_POINT('Ctrl Pts',(0.104888951407889,-0.778435636705529,
-0.12));
#56549=CARTESIAN_POINT('Ctrl Pts',(0.112442728465956,-0.777019807995953,
-0.12));
#56550=CARTESIAN_POINT('Ctrl Pts',(0.119978617797336,-0.775493331514514,
-0.12));
#56551=CARTESIAN_POINT('Ctrl Pts',(0.127482778712085,-0.773858786233986,
-0.12));
#56552=CARTESIAN_POINT('Ctrl Pts',(0.163232326165741,-0.766071872449056,
-0.12));
#56553=CARTESIAN_POINT('Ctrl Pts',(0.198335071471806,-0.755823166547615,
-0.12));
#56554=CARTESIAN_POINT('Ctrl Pts',(0.232522340410342,-0.743135834971473,
-0.12));
#56555=CARTESIAN_POINT('Ctrl Pts',(0.237813230372167,-0.741172318219104,
-0.12));
#56556=CARTESIAN_POINT('Ctrl Pts',(0.243082158223076,-0.739150297995532,
-0.12));
#56557=CARTESIAN_POINT('Ctrl Pts',(0.248328083260998,-0.73706975670363,
-0.12));
#56558=CARTESIAN_POINT('Ctrl Pts',(0.277906408593185,-0.725338951029883,
-0.12));
#56559=CARTESIAN_POINT('Ctrl Pts',(0.306754972760517,-0.711749564176307,
-0.12));
#56560=CARTESIAN_POINT('Ctrl Pts',(0.334717544680486,-0.696396977944506,
-0.12));
#56561=CARTESIAN_POINT('Ctrl Pts',(0.341939489339631,-0.692431837382394,
-0.12));
#56562=CARTESIAN_POINT('Ctrl Pts',(0.349102230975186,-0.688348968720245,
-0.12));
#56563=CARTESIAN_POINT('Ctrl Pts',(0.356202844476414,-0.684149788320379,
-0.12));
#56564=CARTESIAN_POINT('Ctrl Pts',(0.363162967541051,-0.680033691542456,
-0.12));
#56565=CARTESIAN_POINT('Ctrl Pts',(0.370055970531007,-0.675810190952825,
-0.12));
#56566=CARTESIAN_POINT('Ctrl Pts',(0.376876658708298,-0.671483106796323,
-0.12));
#56567=CARTESIAN_POINT('Ctrl Pts',(0.40745623441888,-0.652083246528505,
-0.12));
#56568=CARTESIAN_POINT('Ctrl Pts',(0.436604118212131,-0.630593159071821,
-0.12));
#56569=CARTESIAN_POINT('Ctrl Pts',(0.46410233189715,-0.60717227783143,-0.12));
#56570=CARTESIAN_POINT('Ctrl Pts',(0.491112633055654,-0.58416696327003,
-0.12));
#56571=CARTESIAN_POINT('Ctrl Pts',(0.516532076721098,-0.559297921856729,
-0.12));
#56572=CARTESIAN_POINT('Ctrl Pts',(0.540116340216444,-0.532683959290642,
-0.12));
#56573=CARTESIAN_POINT('Ctrl Pts',(0.545165350086534,-0.52698633978665,
-0.12));
#56574=CARTESIAN_POINT('Ctrl Pts',(0.550130085791934,-0.521208653511241,
-0.12));
#56575=CARTESIAN_POINT('Ctrl Pts',(0.555007866453742,-0.515351924808608,
-0.12));
#56576=CARTESIAN_POINT('',(-0.459778808448974,0.601851132366397,-1.12625));
#56577=CARTESIAN_POINT('Ctrl Pts',(-0.459817636075317,0.601890711574512,
-1.12625));
#56578=CARTESIAN_POINT('Ctrl Pts',(-0.432503985120066,0.625165263761577,
-1.12625));
#56579=CARTESIAN_POINT('Ctrl Pts',(-0.403593713495987,0.646405611026664,
-1.12625));
#56580=CARTESIAN_POINT('Ctrl Pts',(-0.373360039769222,0.665530294930177,
-1.12625));
#56581=CARTESIAN_POINT('Ctrl Pts',(-0.342830078355013,0.684842399271513,
-1.12625));
#56582=CARTESIAN_POINT('Ctrl Pts',(-0.310949650189556,0.701997871851442,
-1.12625));
#56583=CARTESIAN_POINT('Ctrl Pts',(-0.277963229106153,0.716874587570175,
-1.12625));
#56584=CARTESIAN_POINT('Ctrl Pts',(-0.26649732981671,0.722045652468588,
-1.12625));
#56585=CARTESIAN_POINT('Ctrl Pts',(-0.254897548952348,0.726941007906439,
-1.12625));
#56586=CARTESIAN_POINT('Ctrl Pts',(-0.243173471026141,0.731554211541609,
-1.12625));
#56587=CARTESIAN_POINT('Ctrl Pts',(-0.235772847930162,0.734466217209243,
-1.12625));
#56588=CARTESIAN_POINT('Ctrl Pts',(-0.228323386851445,0.737265362586449,
-1.12625));
#56589=CARTESIAN_POINT('Ctrl Pts',(-0.220840169223985,0.739945834211391,
-1.12625));
#56590=CARTESIAN_POINT('Ctrl Pts',(-0.196274161499892,0.748745322602708,
-1.12625));
#56591=CARTESIAN_POINT('Ctrl Pts',(-0.171310177385804,0.756280719952739,
-1.12625));
#56592=CARTESIAN_POINT('Ctrl Pts',(-0.146041756546086,0.762513765607057,
-1.12625));
#56593=CARTESIAN_POINT('Ctrl Pts',(-0.114363689392244,0.770327900097808,
-1.12625));
#56594=CARTESIAN_POINT('Ctrl Pts',(-0.0822071438969164,0.77609639727171,
-1.12625));
#56595=CARTESIAN_POINT('Ctrl Pts',(-0.0497689197316119,0.779842549380837,
-1.12625));
#56596=CARTESIAN_POINT('Ctrl Pts',(-0.0298100993332151,0.782147508393085,
-1.12625));
#56597=CARTESIAN_POINT('Ctrl Pts',(-0.00974437858899013,0.783686221448935,
-1.12625));
#56598=CARTESIAN_POINT('Ctrl Pts',(0.0103835877245399,0.784457979579496,
-1.12625));
#56599=CARTESIAN_POINT('Ctrl Pts',(0.0199668006274251,0.784825424673526,
-1.12625));
#56600=CARTESIAN_POINT('Ctrl Pts',(0.0295667334923406,0.785018756675102,
-1.12625));
#56601=CARTESIAN_POINT('Ctrl Pts',(0.0391548342268405,0.785038051041722,
-1.12625));
#56602=CARTESIAN_POINT('Ctrl Pts',(0.0764066796303495,0.785113013829703,
-1.12625));
#56603=CARTESIAN_POINT('Ctrl Pts',(0.11355304850067,0.782569361975542,-1.12625));
#56604=CARTESIAN_POINT('Ctrl Pts',(0.150309494084269,0.77745070961784,-1.12625));
#56605=CARTESIAN_POINT('Ctrl Pts',(0.181105692018343,0.773162073198822,
-1.12625));
#56606=CARTESIAN_POINT('Ctrl Pts',(0.211628935934584,0.767064947824248,
-1.12625));
#56607=CARTESIAN_POINT('Ctrl Pts',(0.241714208481684,0.759156929049666,
-1.12625));
#56608=CARTESIAN_POINT('Ctrl Pts',(0.258311234815863,0.754794342815906,
-1.12625));
#56609=CARTESIAN_POINT('Ctrl Pts',(0.274774951161081,0.74988017519975,-1.12625));
#56610=CARTESIAN_POINT('Ctrl Pts',(0.291082790748006,0.744427662964972,
-1.12625));
#56611=CARTESIAN_POINT('Ctrl Pts',(0.302253486659231,0.740692750329715,
-1.12625));
#56612=CARTESIAN_POINT('Ctrl Pts',(0.313351031748266,0.736705191681207,
-1.12625));
#56613=CARTESIAN_POINT('Ctrl Pts',(0.324367932128155,0.73246863871898,-1.12625));
#56614=CARTESIAN_POINT('Ctrl Pts',(0.331410788641081,0.729760305740237,
-1.12625));
#56615=CARTESIAN_POINT('Ctrl Pts',(0.338411390394597,0.72695377103039,-1.12625));
#56616=CARTESIAN_POINT('Ctrl Pts',(0.345367277999311,0.724051012762939,
-1.12625));
#56617=CARTESIAN_POINT('Ctrl Pts',(0.379999812823563,0.709598525532449,
-1.12625));
#56618=CARTESIAN_POINT('Ctrl Pts',(0.413530302276288,0.692762730520224,
-1.12625));
#56619=CARTESIAN_POINT('Ctrl Pts',(0.445738862386879,0.673721922806075,
-1.12625));
#56620=CARTESIAN_POINT('Ctrl Pts',(0.47805582561834,0.654617030172481,-1.12625));
#56621=CARTESIAN_POINT('Ctrl Pts',(0.509043040540198,0.63329174243941,-1.12625));
#56622=CARTESIAN_POINT('Ctrl Pts',(0.538461112130946,0.609877570946476,
-1.12625));
#56623=CARTESIAN_POINT('Ctrl Pts',(0.555983532413065,0.595931281088856,
-1.12625));
#56624=CARTESIAN_POINT('Ctrl Pts',(0.57294884620607,0.581243006920529,-1.12625));
#56625=CARTESIAN_POINT('Ctrl Pts',(0.589301091561381,0.565833523687246,
-1.12625));
#56626=CARTESIAN_POINT('Ctrl Pts',(-0.459817636075315,0.601890711574514,
-1.12625));
#56627=CARTESIAN_POINT('Ctrl Pts',(-0.466706837362038,0.596634000305894,
-1.12600649737474));
#56628=CARTESIAN_POINT('Ctrl Pts',(-0.571995661495492,0.513358547689718,
-1.12223485618063));
#56629=CARTESIAN_POINT('Ctrl Pts',(-0.731074678445063,0.297631408040504,
-1.11493507641766));
#56630=CARTESIAN_POINT('Ctrl Pts',(-0.78448657507111,-0.0873109114175063,
-1.10435066071109));
#56631=CARTESIAN_POINT('Ctrl Pts',(-0.647739858405566,-0.451090008407739,
-1.09376624500452));
#56632=CARTESIAN_POINT('Ctrl Pts',(-0.35396552579895,-0.705517309450156,
-1.08318182929794));
#56633=CARTESIAN_POINT('Ctrl Pts',(0.0256119661671881,-0.788917676587972,
-1.07259741359137));
#56634=CARTESIAN_POINT('Ctrl Pts',(0.398982356900771,-0.681072808505694,
-1.0620129978848));
#56635=CARTESIAN_POINT('Ctrl Pts',(0.675632891112322,-0.40812628276753,
-1.05142858217823));
#56636=CARTESIAN_POINT('Ctrl Pts',(0.788500750688369,-0.0362440247522399,
-1.04084416647166));
#56637=CARTESIAN_POINT('Ctrl Pts',(0.710224521156417,0.344424265850664,
-1.03025975076509));
#56638=CARTESIAN_POINT('Ctrl Pts',(0.459779801870057,0.641599200064961,
-1.01967533505852));
#56639=CARTESIAN_POINT('Ctrl Pts',(0.097877817393331,0.783241287520996,
-1.00909091935195));
#56640=CARTESIAN_POINT('Ctrl Pts',(-0.287751124101878,0.735014472176637,
-0.998506503645378));
#56641=CARTESIAN_POINT('Ctrl Pts',(-0.603625085401645,0.508609617298406,
-0.987922087938805));
#56642=CARTESIAN_POINT('Ctrl Pts',(-0.773171671953705,0.158910506780707,
-0.977337672232237));
#56643=CARTESIAN_POINT('Ctrl Pts',(-0.755290373416537,-0.229310787602246,
-0.966753256525664));
#56644=CARTESIAN_POINT('Ctrl Pts',(-0.554315867123395,-0.561943861908008,
-0.956168840819094));
#56645=CARTESIAN_POINT('Ctrl Pts',(-0.218967255152568,-0.758353694545465,
-0.945584425112524));
#56646=CARTESIAN_POINT('Ctrl Pts',(0.169462156609868,-0.770927728297873,
-0.935000009405952));
#56647=CARTESIAN_POINT('Ctrl Pts',(0.516811513855876,-0.596617837396196,
-0.924415593699383));
#56648=CARTESIAN_POINT('Ctrl Pts',(0.738878357065632,-0.277679236275888,
-0.91383117799281));
#56649=CARTESIAN_POINT('Ctrl Pts',(0.781830502198587,0.108572789396219,
-0.903246762286241));
#56650=CARTESIAN_POINT('Ctrl Pts',(0.635255734092279,0.468505215644772,
-0.892662346579669));
#56651=CARTESIAN_POINT('Ctrl Pts',(0.334685876135465,0.714865266390365,
-0.882077930873099));
#56652=CARTESIAN_POINT('Ctrl Pts',(-0.0470166324849972,0.787931736286691,
-0.871493515166528));
#56653=CARTESIAN_POINT('Ctrl Pts',(-0.417321635893157,0.669992266368472,
-0.860909099459957));
#56654=CARTESIAN_POINT('Ctrl Pts',(-0.686461896723767,0.389637073600391,
-0.850324683753386));
#56655=CARTESIAN_POINT('Ctrl Pts',(-0.78919396038351,0.0148282727314064,
-0.839740268046816));
#56656=CARTESIAN_POINT('Ctrl Pts',(-0.700614103026785,-0.363575113859107,
-0.829155852340244));
#56657=CARTESIAN_POINT('Ctrl Pts',(-0.442195350963465,-0.65384268472174,
-0.818571436633674));
#56658=CARTESIAN_POINT('Ctrl Pts',(-0.0765821114814538,-0.785609422664232,
-0.807987020927103));
#56659=CARTESIAN_POINT('Ctrl Pts',(0.307595728844424,-0.726933182881658,
-0.797402605220531));
#56660=CARTESIAN_POINT('Ctrl Pts',(0.617207958261566,-0.492037926420706,
-0.786818189513963));
#56661=CARTESIAN_POINT('Ctrl Pts',(0.77720013723641,-0.137865628267142,
-0.776233773807389));
#56662=CARTESIAN_POINT('Ctrl Pts',(0.748787869734938,0.249727273071264,
-0.765649358100821));
#56663=CARTESIAN_POINT('Ctrl Pts',(0.538858696398575,0.576782706132406,
-0.755064942394248));
#56664=CARTESIAN_POINT('Ctrl Pts',(0.198302456030381,0.764017748949666,
-0.744480526687679));
#56665=CARTESIAN_POINT('Ctrl Pts',(-0.19032514031589,0.766043945045929,
-0.733896110981107));
#56666=CARTESIAN_POINT('Ctrl Pts',(-0.532815196286458,0.582370115462682,
-0.723311695274537));
#56667=CARTESIAN_POINT('Ctrl Pts',(-0.746143216224097,0.257521427575559,
-0.712727279567965));
#56668=CARTESIAN_POINT('Ctrl Pts',(-0.778595432221923,-0.129754143290109,
-0.702142863861395));
#56669=CARTESIAN_POINT('Ctrl Pts',(-0.622304962251659,-0.485575451124495,
-0.691558448154824));
#56670=CARTESIAN_POINT('Ctrl Pts',(-0.315158855058528,-0.723686313851513,
-0.680974032448254));
#56671=CARTESIAN_POINT('Ctrl Pts',(0.0683862731776896,-0.786365247463709,
-0.670389616741681));
#56672=CARTESIAN_POINT('Ctrl Pts',(0.435353589178266,-0.658417980592417,
-0.659805201035112));
#56673=CARTESIAN_POINT('Ctrl Pts',(0.696784958823668,-0.370860763541915,
-0.64922078532854));
#56674=CARTESIAN_POINT('Ctrl Pts',(0.789305673168617,0.00659841508485966,
-0.63863636962197));
#56675=CARTESIAN_POINT('Ctrl Pts',(0.690487385718296,0.382458043374312,
-0.6280519539154));
#56676=CARTESIAN_POINT('Ctrl Pts',(0.424285064899528,0.665604363327792,
-0.617467538208828));
#56677=CARTESIAN_POINT('Ctrl Pts',(0.0552299665647739,0.787398650983763,
-0.606883122502257));
#56678=CARTESIAN_POINT('Ctrl Pts',(-0.327213666821637,0.718316226339718,
-0.596298706795687));
#56679=CARTESIAN_POINT('Ctrl Pts',(-0.630336020111223,0.475103658718956,
-0.585714291089115));
#56680=CARTESIAN_POINT('Ctrl Pts',(-0.780655892709758,0.116719158475909,
-0.575129875382546));
#56681=CARTESIAN_POINT('Ctrl Pts',(-0.741733594202337,-0.269959737756351,
-0.564545459675974));
#56682=CARTESIAN_POINT('Ctrl Pts',(-0.52300444729998,-0.591196526446356,
-0.553961043969404));
#56683=CARTESIAN_POINT('Ctrl Pts',(-0.177491530455701,-0.76911880837377,
-0.543376628262832));
#56684=CARTESIAN_POINT('Ctrl Pts',(0.211047875895708,-0.760595673704304,
-0.532792212556262));
#56685=CARTESIAN_POINT('Ctrl Pts',(0.548426253918526,-0.567693252373749,
-0.522207796849691));
#56686=CARTESIAN_POINT('Ctrl Pts',(0.752858251913653,-0.237173854594711,
-0.511623381143121));
#56687=CARTESIAN_POINT('Ctrl Pts',(0.7747866251265,0.150839882998094,-0.501038965436549));
#56688=CARTESIAN_POINT('Ctrl Pts',(0.608895621771465,0.502287872206109,
-0.490454549729979));
#56689=CARTESIAN_POINT('Ctrl Pts',(0.295399597411609,0.731974086035053,
-0.479870134023407));
#56690=CARTESIAN_POINT('Ctrl Pts',(-0.0897055208909376,0.784219296051475,
-0.469285718316837));
#56691=CARTESIAN_POINT('Ctrl Pts',(-0.453064735918984,0.646358514947002,
-0.458701302610266));
#56692=CARTESIAN_POINT('Ctrl Pts',(-0.706594568913726,0.351811170884772,
-0.448116886903695));
#56693=CARTESIAN_POINT('Ctrl Pts',(-0.788835756602106,-0.028020240612635,
-0.437532471197125));
#56694=CARTESIAN_POINT('Ctrl Pts',(-0.679851857001812,-0.401059144402238,
-0.426948055490553));
#56695=CARTESIAN_POINT('Ctrl Pts',(-0.40606212854653,-0.676875566510097,
-0.416363639783983));
#56696=CARTESIAN_POINT('Ctrl Pts',(-0.033837123384323,-0.788607655212059,
-0.405779224077412));
#56697=CARTESIAN_POINT('Ctrl Pts',(0.346590485190783,-0.709169951669662,
-0.395194808370841));
#56698=CARTESIAN_POINT('Ctrl Pts',(0.642999595336517,-0.457819293150201,
-0.38461039266427));
#56699=CARTESIAN_POINT('Ctrl Pts',(0.78353639273709,-0.0954866798140887,
-0.3740259769577));
#56700=CARTESIAN_POINT('Ctrl Pts',(0.734132744595481,0.28999327252796,-0.363441561251129));
#56701=CARTESIAN_POINT('Ctrl Pts',(0.506764802819437,0.605174701533939,
-0.352857145544558));
#56702=CARTESIAN_POINT('Ctrl Pts',(0.156549813679528,0.773653113881338,
-0.342272729837987));
#56703=CARTESIAN_POINT('Ctrl Pts',(-0.231615093084919,0.754586929064552,
-0.331688314131416));
#56704=CARTESIAN_POINT('Ctrl Pts',(-0.563633182964234,0.552598063281491,
-0.321103898424845));
#56705=CARTESIAN_POINT('Ctrl Pts',(-0.759018516340423,0.216651511277527,
-0.310519482718275));
#56706=CARTESIAN_POINT('Ctrl Pts',(-0.770406886705707,-0.171814470849831,
-0.299935067011704));
#56707=CARTESIAN_POINT('Ctrl Pts',(-0.595037595541395,-0.518630163437193,
-0.289350651305133));
#56708=CARTESIAN_POINT('Ctrl Pts',(-0.275422660164443,-0.739722476337535,
-0.278766235598562));
#56709=CARTESIAN_POINT('Ctrl Pts',(0.11095865910622,-0.78149546229302,-0.268181819891991));
#56710=CARTESIAN_POINT('Ctrl Pts',(0.470442038027593,-0.63382275802318,
-0.257597404185421));
#56711=CARTESIAN_POINT('Ctrl Pts',(0.715883472822082,-0.332502328862262,
-0.24701298847885));
#56712=CARTESIAN_POINT('Ctrl Pts',(0.787784607225333,0.0494214101901834,
-0.236428572772279));
#56713=CARTESIAN_POINT('Ctrl Pts',(0.668715255345623,0.419364726111387,
-0.225844157065708));
#56714=CARTESIAN_POINT('Ctrl Pts',(0.387540164029785,0.687647957073743,
-0.215259741359137));
#56715=CARTESIAN_POINT('Ctrl Pts',(0.0124189653016963,0.789235606485636,
-0.204675325652567));
#56716=CARTESIAN_POINT('Ctrl Pts',(-0.365711157649466,0.699500976810326,
-0.194090909945995));
#56717=CARTESIAN_POINT('Ctrl Pts',(-0.655190820886885,0.440197805626207,
-0.183506494239425));
#56718=CARTESIAN_POINT('Ctrl Pts',(-0.785836630350135,0.0741833682121523,
-0.172922078532854));
#56719=CARTESIAN_POINT('Ctrl Pts',(-0.72599658874823,-0.309812190918401,
-0.162337662826283));
#56720=CARTESIAN_POINT('Ctrl Pts',(-0.490140575868292,-0.618708756217204,
-0.151753247119713));
#56721=CARTESIAN_POINT('Ctrl Pts',(-0.135514917188131,-0.777613622822956,
-0.141168831413141));
#56722=CARTESIAN_POINT('Ctrl Pts',(0.252058240770739,-0.748030699511335,
-0.130584415706571));
#56723=CARTESIAN_POINT('Ctrl Pts',(0.469550542503088,-0.607385125337185,
-0.123528138568857));
#56724=CARTESIAN_POINT('Ctrl Pts',(0.555007866453742,-0.515351924808608,
-0.12));
#56725=CARTESIAN_POINT('Ctrl Pts',(-0.453782243834438,0.594001620520165,
-1.1425283350431));
#56726=CARTESIAN_POINT('Ctrl Pts',(-0.550881388338772,0.519823594492229,
-1.13905034750894));
#56727=CARTESIAN_POINT('Ctrl Pts',(-0.707932320584141,0.323031319671979,
-1.13209437244062));
#56728=CARTESIAN_POINT('Ctrl Pts',(-0.776614466270609,-0.0485165662670007,
-1.12166040983814));
#56729=CARTESIAN_POINT('Ctrl Pts',(-0.662248238305512,-0.408538693637006,
-1.11122644723566));
#56730=CARTESIAN_POINT('Ctrl Pts',(-0.391780881856498,-0.672308433025162,
-1.10079248463318));
#56731=CARTESIAN_POINT('Ctrl Pts',(-0.0289685614302447,-0.77758653236944,
-1.0903585220307));
#56732=CARTESIAN_POINT('Ctrl Pts',(0.340672665444815,-0.699591456600573,
-1.07992455942822));
#56733=CARTESIAN_POINT('Ctrl Pts',(0.630013764781798,-0.45669036663525,
-1.06949059682573));
#56734=CARTESIAN_POINT('Ctrl Pts',(0.770854889346007,-0.106145976774946,
-1.05905663422326));
#56735=CARTESIAN_POINT('Ctrl Pts',(0.72999817257357,0.269419497799126,-1.04862267162077));
#56736=CARTESIAN_POINT('Ctrl Pts',(0.517074073818034,0.581479511865617,
-1.03818870901829));
#56737=CARTESIAN_POINT('Ctrl Pts',(0.182270729955259,0.756479721113076,
-1.02775474641581));
#56738=CARTESIAN_POINT('Ctrl Pts',(-0.195495525574089,0.753170354596227,
-1.01732078381333));
#56739=CARTESIAN_POINT('Ctrl Pts',(-0.527181654493514,0.572331754114927,
-1.00688682121085));
#56740=CARTESIAN_POINT('Ctrl Pts',(-0.734606108414346,0.256589128857393,
-0.996452858608371));
#56741=CARTESIAN_POINT('Ctrl Pts',(-0.768876998658737,-0.119633940618216,
-0.98601889600589));
#56742=CARTESIAN_POINT('Ctrl Pts',(-0.621916351700691,-0.467658178639452,
-0.97558493340341));
#56743=CARTESIAN_POINT('Ctrl Pts',(-0.328364174807744,-0.705450981188053,
-0.965150970800929));
#56744=CARTESIAN_POINT('Ctrl Pts',(0.0425865250681738,-0.776962359283856,
-0.954717008198449));
#56745=CARTESIAN_POINT('Ctrl Pts',(0.403499180542324,-0.665336403825433,
-0.944283045595967));
#56746=CARTESIAN_POINT('Ctrl Pts',(0.669303286159026,-0.396884404409992,
-0.933849082993487));
#56747=CARTESIAN_POINT('Ctrl Pts',(0.777346315469045,-0.0348830195569247,
-0.923415120391007));
#56748=CARTESIAN_POINT('Ctrl Pts',(0.702161510858138,0.335340620697414,
-0.912981157788526));
#56749=CARTESIAN_POINT('Ctrl Pts',(0.461470637519424,0.626521324425116,
-0.902547195186045));
#56750=CARTESIAN_POINT('Ctrl Pts',(0.112006796904718,0.770025062366403,
-0.892113232583565));
#56751=CARTESIAN_POINT('Ctrl Pts',(-0.26385809865297,0.732026654580473,
-0.881679269981084));
#56752=CARTESIAN_POINT('Ctrl Pts',(-0.577529159980992,0.521482682939164,
-0.871245307378604));
#56753=CARTESIAN_POINT('Ctrl Pts',(-0.75507116928701,0.188020340781937,
-0.860811344776122));
#56754=CARTESIAN_POINT('Ctrl Pts',(-0.754635806007903,-0.189760163171063,
-0.850377382173643));
#56755=CARTESIAN_POINT('Ctrl Pts',(-0.576325689361536,-0.522812412838008,
-0.839943419571161));
#56756=CARTESIAN_POINT('Ctrl Pts',(-0.262170190030731,-0.732632862145289,
-0.829509456968681));
#56757=CARTESIAN_POINT('Ctrl Pts',(0.113781287599417,-0.769764858789943,
-0.8190754943662));
#56758=CARTESIAN_POINT('Ctrl Pts',(0.462913446150841,-0.625456042107333,
-0.808641531763721));
#56759=CARTESIAN_POINT('Ctrl Pts',(0.702932553865032,-0.333721356752229,
-0.798207569161239));
#56760=CARTESIAN_POINT('Ctrl Pts',(0.77726385077405,0.036674589509254,-0.787773606558759));
#56761=CARTESIAN_POINT('Ctrl Pts',(0.668386751451238,0.398425990267,-0.777339643956278));
#56762=CARTESIAN_POINT('Ctrl Pts',(0.401964611697131,0.666264639748313,
-0.766905681353797));
#56763=CARTESIAN_POINT('Ctrl Pts',(0.0407956343310049,0.777058450475451,
-0.756471718751316));
#56764=CARTESIAN_POINT('Ctrl Pts',(-0.329989257542916,0.704692279751986,
-0.746037756148837));
#56765=CARTESIAN_POINT('Ctrl Pts',(-0.622992579377318,0.466223514289631,
-0.735603793546355));
#56766=CARTESIAN_POINT('Ctrl Pts',(-0.769150693862395,0.11786148381372,
-0.725169830943876));
#56767=CARTESIAN_POINT('Ctrl Pts',(-0.734012759466783,-0.258281606344191,
-0.714735868341394));
#56768=CARTESIAN_POINT('Ctrl Pts',(-0.525861117638762,-0.573545293931952,
-0.704301905738914));
#56769=CARTESIAN_POINT('Ctrl Pts',(-0.19375906706945,-0.753618964174968,
-0.693867943136433));
#56770=CARTESIAN_POINT('Ctrl Pts',(0.184013817024176,-0.756057560229359,
-0.683433980533953));
#56771=CARTESIAN_POINT('Ctrl Pts',(0.518412914638575,-0.580286282081279,
-0.673000017931471));
#56772=CARTESIAN_POINT('Ctrl Pts',(0.73061721497504,-0.267736072313561,
-0.662566055328992));
#56773=CARTESIAN_POINT('Ctrl Pts',(0.770608169635336,0.107922046529214,
-0.65213209272651));
#56774=CARTESIAN_POINT('Ctrl Pts',(0.628959534674377,0.458141924492801,
-0.641698130124031));
#56775=CARTESIAN_POINT('Ctrl Pts',(0.339059224908709,0.700373444128261,
-0.631264167521549));
#56776=CARTESIAN_POINT('Ctrl Pts',(-0.0307605314660725,0.777520359180196,
-0.620830204919069));
#56777=CARTESIAN_POINT('Ctrl Pts',(-0.393329741412475,0.671398416557689,
-0.610396242316588));
#56778=CARTESIAN_POINT('Ctrl Pts',(-0.663187433844336,0.407021555727386,
-0.599962279714107));
#56779=CARTESIAN_POINT('Ctrl Pts',(-0.776725613880599,0.0467058880397525,
-0.589528317111628));
#56780=CARTESIAN_POINT('Ctrl Pts',(-0.707182265180475,-0.324618796513678,
-0.579094354509146));
#56781=CARTESIAN_POINT('Ctrl Pts',(-0.470949408769063,-0.619427779176754,
-0.568660391906666));
#56782=CARTESIAN_POINT('Ctrl Pts',(-0.123709349589915,-0.768231811408391,
-0.558226429304186));
#56783=CARTESIAN_POINT('Ctrl Pts',(0.25269016620706,-0.735956383991622,
-0.547792466701704));
#56784=CARTESIAN_POINT('Ctrl Pts',(0.569528234436074,-0.530209118571064,
-0.537358504099225));
#56785=CARTESIAN_POINT('Ctrl Pts',(0.752123144005562,-0.199486579716445,
-0.526924541496743));
#56786=CARTESIAN_POINT('Ctrl Pts',(0.757435558261681,0.178256821234392,
-0.516490578894263));
#56787=CARTESIAN_POINT('Ctrl Pts',(0.58421329122536,0.513983413731815,-0.506056616291782));
#56788=CARTESIAN_POINT('Ctrl Pts',(0.273286459598611,0.728559283954183,
-0.495622653689302));
#56789=CARTESIAN_POINT('Ctrl Pts',(-0.102056559562228,0.771406882187409,
-0.485188691086821));
#56790=CARTESIAN_POINT('Ctrl Pts',(-0.453343888260037,0.632426626742619,
-0.47475472848434));
#56791=CARTESIAN_POINT('Ctrl Pts',(-0.697773800873295,0.344377470300542,
-0.46432076588186));
#56792=CARTESIAN_POINT('Ctrl Pts',(-0.777731869256009,-0.0248446931832663,
-0.453886803279379));
#56793=CARTESIAN_POINT('Ctrl Pts',(-0.674371225051021,-0.388210728933227,
-0.443452840676899));
#56794=CARTESIAN_POINT('Ctrl Pts',(-0.412054943730932,-0.660071846531001,
-0.433018878074418));
#56795=CARTESIAN_POINT('Ctrl Pts',(-0.052613438684712,-0.776347824950466,
-0.422584915471938));
#56796=CARTESIAN_POINT('Ctrl Pts',(0.319229548446942,-0.709631323036312,
-0.412150952869457));
#56797=CARTESIAN_POINT('Ctrl Pts',(0.615827130120364,-0.475648047450975,
-0.401716990266977));
#56798=CARTESIAN_POINT('Ctrl Pts',(0.767268468189366,-0.129550055793595,
-0.391283027664495));
#56799=CARTESIAN_POINT('Ctrl Pts',(0.73785741566876,0.247084101843196,-0.380849065062015));
#56800=CARTESIAN_POINT('Ctrl Pts',(0.53452643409528,0.565478213973466,-0.370415102459534));
#56801=CARTESIAN_POINT('Ctrl Pts',(0.205202547258297,0.750583795355784,
-0.359981139857054));
#56802=CARTESIAN_POINT('Ctrl Pts',(-0.172489509004575,0.758769720339227,
-0.349547177254573));
#56803=CARTESIAN_POINT('Ctrl Pts',(-0.509524166428119,0.588106489551374,
-0.339113214652092));
#56804=CARTESIAN_POINT('Ctrl Pts',(-0.726459188269099,0.278821030603047,
-0.328679252049613));
#56805=CARTESIAN_POINT('Ctrl Pts',(-0.772160950053183,-0.0961851660426531,
-0.318245289447131));
#56806=CARTESIAN_POINT('Ctrl Pts',(-0.635857117988054,-0.448519615362855,
-0.307811326844651));
#56807=CARTESIAN_POINT('Ctrl Pts',(-0.349675784487414,-0.695133774103566,
-0.29737736424217));
#56808=CARTESIAN_POINT('Ctrl Pts',(0.0189274157531999,-0.777898369643473,
-0.28694340163969));
#56809=CARTESIAN_POINT('Ctrl Pts',(0.383069251609923,-0.677305003145055,
-0.276509439037209));
#56810=CARTESIAN_POINT('Ctrl Pts',(0.656918053157327,-0.417064487823471,
-0.266075476434728));
#56811=CARTESIAN_POINT('Ctrl Pts',(0.775925115315039,-0.0585179376441868,
-0.255641513832248));
#56812=CARTESIAN_POINT('Ctrl Pts',(0.712039292365906,0.313821812003498,
-0.245207551229767));
#56813=CARTESIAN_POINT('Ctrl Pts',(0.480319196218488,0.612190866640268,
-0.234773588627287));
#56814=CARTESIAN_POINT('Ctrl Pts',(0.135383189993233,0.766260668703223,
-0.224339626024806));
#56815=CARTESIAN_POINT('Ctrl Pts',(-0.24146359128836,0.739715845333337,
-0.213905663422326));
#56816=CARTESIAN_POINT('Ctrl Pts',(-0.561395755032477,0.538812615893194,
-0.203471700819845));
#56817=CARTESIAN_POINT('Ctrl Pts',(-0.749000440414917,0.210907029399764,
-0.193037738217364));
#56818=CARTESIAN_POINT('Ctrl Pts',(-0.760061084770159,-0.166712982541238,
-0.182603775614884));
#56819=CARTESIAN_POINT('Ctrl Pts',(-0.591963456523637,-0.50503391867701,
-0.172169813012403));
#56820=CARTESIAN_POINT('Ctrl Pts',(-0.284343786563672,-0.724320025643111,
-0.161735850409922));
#56821=CARTESIAN_POINT('Ctrl Pts',(0.0903167314019248,-0.772864465068914,
-0.151301887807442));
#56822=CARTESIAN_POINT('Ctrl Pts',(0.443652359236502,-0.639262442637615,
-0.140867925204961));
#56823=CARTESIAN_POINT('Ctrl Pts',(0.692489824641793,-0.354929918130671,
-0.130433962602481));
#56824=CARTESIAN_POINT('Ctrl Pts',(0.749438361810143,-0.109676867461668,
-0.12347798753416));
#56825=CARTESIAN_POINT('Ctrl Pts',(0.747395528060274,0.0124969850565577,
-0.12));
#56826=CARTESIAN_POINT('Ctrl Pts',(-0.453782243834438,0.594001620520165,
-1.13966850381659));
#56827=CARTESIAN_POINT('Ctrl Pts',(-0.550881059946449,0.519823845364617,
-1.13619051628243));
#56828=CARTESIAN_POINT('Ctrl Pts',(-0.707932492103508,0.323031139564102,
-1.12923454121411));
#56829=CARTESIAN_POINT('Ctrl Pts',(-0.776614348027597,-0.0485164852858499,
-1.11880057861163));
#56830=CARTESIAN_POINT('Ctrl Pts',(-0.662248261705562,-0.408538719445684,
-1.10836661600915));
#56831=CARTESIAN_POINT('Ctrl Pts',(-0.391780845205789,-0.672308389976757,
-1.09793265340667));
#56832=CARTESIAN_POINT('Ctrl Pts',(-0.0289685722792091,-0.777586516102956,
-1.08749869080419));
#56833=CARTESIAN_POINT('Ctrl Pts',(0.340672659850847,-0.699591427563091,
-1.07706472820171));
#56834=CARTESIAN_POINT('Ctrl Pts',(0.630013740257184,-0.456690353715166,
-1.06663076559923));
#56835=CARTESIAN_POINT('Ctrl Pts',(0.770854864632094,-0.106145971815379,
-1.05619680299675));
#56836=CARTESIAN_POINT('Ctrl Pts',(0.729998146909112,0.26941948793622,-1.04576284039427));
#56837=CARTESIAN_POINT('Ctrl Pts',(0.517074056599656,0.581479492398161,
-1.03532887779179));
#56838=CARTESIAN_POINT('Ctrl Pts',(0.182270723540416,0.756479695159438,
-1.02489491518931));
#56839=CARTESIAN_POINT('Ctrl Pts',(-0.195495518808872,0.753170329021128,
-1.01446095258683));
#56840=CARTESIAN_POINT('Ctrl Pts',(-0.527181636582193,0.572331734566928,
-1.00402698998435));
#56841=CARTESIAN_POINT('Ctrl Pts',(-0.73460608335552,0.25658912013712,-0.993593027381866));
#56842=CARTESIAN_POINT('Ctrl Pts',(-0.768876972472472,-0.119633936553384,
-0.983159064779384));
#56843=CARTESIAN_POINT('Ctrl Pts',(-0.621916330501673,-0.467658162697795,
-0.972725102176904));
#56844=CARTESIAN_POINT('Ctrl Pts',(-0.328364163622084,-0.705450957152497,
-0.962291139574423));
#56845=CARTESIAN_POINT('Ctrl Pts',(0.0425865236188016,-0.776962332806938,
-0.951857176971944));
#56846=CARTESIAN_POINT('Ctrl Pts',(0.403499166791982,-0.665336381154549,
-0.941423214369461));
#56847=CARTESIAN_POINT('Ctrl Pts',(0.669303263352646,-0.396884390885562,
-0.930989251766982));
#56848=CARTESIAN_POINT('Ctrl Pts',(0.777346288980351,-0.0348830183684705,
-0.920555289164501));
#56849=CARTESIAN_POINT('Ctrl Pts',(0.702161486931755,0.335340609270619,
-0.910121326562021));
#56850=CARTESIAN_POINT('Ctrl Pts',(0.461470621794524,0.626521303076041,
-0.899687363959539));
#56851=CARTESIAN_POINT('Ctrl Pts',(0.112006793088061,0.770025036127443,
-0.889253401357059));
#56852=CARTESIAN_POINT('Ctrl Pts',(-0.26385808966189,0.73202662963629,-0.878819438754579));
#56853=CARTESIAN_POINT('Ctrl Pts',(-0.577529140301392,0.52148266516939,
-0.868385476152097));
#56854=CARTESIAN_POINT('Ctrl Pts',(-0.755071143557591,0.188020334375048,
-0.857951513549617));
#56855=CARTESIAN_POINT('Ctrl Pts',(-0.754635780293312,-0.189760156704889,
-0.847517550947137));
#56856=CARTESIAN_POINT('Ctrl Pts',(-0.576325669722955,-0.522812395022917,
-0.837083588344655));
#56857=CARTESIAN_POINT('Ctrl Pts',(-0.262170181097151,-0.732632837180461,
-0.826649625742176));
#56858=CARTESIAN_POINT('Ctrl Pts',(0.113781283722264,-0.769764832559824,
-0.816215663139694));
#56859=CARTESIAN_POINT('Ctrl Pts',(0.462913430376835,-0.62545602079461,
-0.805781700537214));
#56860=CARTESIAN_POINT('Ctrl Pts',(0.702932529912258,-0.333721345380508,
-0.795347737934733));
#56861=CARTESIAN_POINT('Ctrl Pts',(0.7772638242884,0.0366745882595488,-0.784913775332253));
#56862=CARTESIAN_POINT('Ctrl Pts',(0.668386728675628,0.398425976690438,
-0.774479812729773));
#56863=CARTESIAN_POINT('Ctrl Pts',(0.401964597999988,0.666264617045015,
-0.764045850127292));
#56864=CARTESIAN_POINT('Ctrl Pts',(0.0407956329408735,0.7770584239968,-0.753611887524811));
#56865=CARTESIAN_POINT('Ctrl Pts',(-0.329989246298369,0.704692255739247,
-0.743177924922331));
#56866=CARTESIAN_POINT('Ctrl Pts',(-0.622992558148537,0.466223498402834,
-0.73274396231985));
#56867=CARTESIAN_POINT('Ctrl Pts',(-0.769150667653205,0.117861479797531,
-0.722309999717369));
#56868=CARTESIAN_POINT('Ctrl Pts',(-0.734012734454935,-0.258281597543118,
-0.711876037114889));
#56869=CARTESIAN_POINT('Ctrl Pts',(-0.525861099719784,-0.573545274388111,
-0.701442074512408));
#56870=CARTESIAN_POINT('Ctrl Pts',(-0.193759060467014,-0.75361893849503,
-0.691008111909928));
#56871=CARTESIAN_POINT('Ctrl Pts',(0.184013810753815,-0.756057534466323,
-0.680574149307446));
#56872=CARTESIAN_POINT('Ctrl Pts',(0.518412896973398,-0.580286262307737,
-0.670140186704967));
#56873=CARTESIAN_POINT('Ctrl Pts',(0.730617190078898,-0.267736063190322,
-0.659706224102485));
#56874=CARTESIAN_POINT('Ctrl Pts',(0.770608143376481,0.107922042851716,
-0.649272261500006));
#56875=CARTESIAN_POINT('Ctrl Pts',(0.62895951324227,0.458141908881389,-0.638838298897524));
#56876=CARTESIAN_POINT('Ctrl Pts',(0.339059213355098,0.700373420262689,
-0.628404336295044));
#56877=CARTESIAN_POINT('Ctrl Pts',(-0.0307605304178917,0.777520332685806,
-0.617970373692564));
#56878=CARTESIAN_POINT('Ctrl Pts',(-0.39332972800957,0.671398393679455,
-0.607536411090082));
#56879=CARTESIAN_POINT('Ctrl Pts',(-0.663187411245896,0.407021541857926,
-0.597102448487602));
#56880=CARTESIAN_POINT('Ctrl Pts',(-0.77672558741329,0.0467058864482261,
-0.586668485885121));
#56881=CARTESIAN_POINT('Ctrl Pts',(-0.70718224108289,-0.324618785452132,
-0.576234523282641));
#56882=CARTESIAN_POINT('Ctrl Pts',(-0.470949392721229,-0.619427758069446,
-0.56580056068016));
#56883=CARTESIAN_POINT('Ctrl Pts',(-0.123709345374458,-0.768231785230511,
-0.55536659807768));
#56884=CARTESIAN_POINT('Ctrl Pts',(0.252690157596518,-0.735956358913544,
-0.544932635475199));
#56885=CARTESIAN_POINT('Ctrl Pts',(0.569528215029118,-0.530209100503925,
-0.534498672872719));
#56886=CARTESIAN_POINT('Ctrl Pts',(0.752123118376594,-0.199486572918841,
-0.524064710270237));
#56887=CARTESIAN_POINT('Ctrl Pts',(0.757435532451691,0.178256815160203,
-0.513630747667758));
#56888=CARTESIAN_POINT('Ctrl Pts',(0.584213271318003,0.513983396217576,
-0.503196785065276));
#56889=CARTESIAN_POINT('Ctrl Pts',(0.27328645028624,0.728559259128164,-0.492762822462796));
#56890=CARTESIAN_POINT('Ctrl Pts',(-0.1020565560846,0.771406855901339,-0.482328859860315));
#56891=CARTESIAN_POINT('Ctrl Pts',(-0.45334387281212,0.632426605192368,
-0.471894897257835));
#56892=CARTESIAN_POINT('Ctrl Pts',(-0.697773777096307,0.344377458565709,
-0.461460934655354));
#56893=CARTESIAN_POINT('Ctrl Pts',(-0.777731842754411,-0.0248446923366709,
-0.451026972052874));
#56894=CARTESIAN_POINT('Ctrl Pts',(-0.674371202071488,-0.388210715704755,
-0.440593009450393));
#56895=CARTESIAN_POINT('Ctrl Pts',(-0.412054929689956,-0.660071824038725,
-0.430159046847913));
#56896=CARTESIAN_POINT('Ctrl Pts',(-0.0526134368918829,-0.776347798496032,
-0.419725084245432));
#56897=CARTESIAN_POINT('Ctrl Pts',(0.319229537569037,-0.70963129885527,
-0.409291121642951));
#56898=CARTESIAN_POINT('Ctrl Pts',(0.61582710913575,-0.475648031243039,
-0.398857159040471));
#56899=CARTESIAN_POINT('Ctrl Pts',(0.767268442044313,-0.129550051379102,
-0.38842319643799));
#56900=CARTESIAN_POINT('Ctrl Pts',(0.737857390525903,0.247084093423662,
-0.37798923383551));
#56901=CARTESIAN_POINT('Ctrl Pts',(0.534526415881029,0.565478194704557,
-0.367555271233028));
#56902=CARTESIAN_POINT('Ctrl Pts',(0.205202540265916,0.750583769779189,
-0.357121308630549));
#56903=CARTESIAN_POINT('Ctrl Pts',(-0.172489503126903,0.758769694483931,
-0.346687346028067));
#56904=CARTESIAN_POINT('Ctrl Pts',(-0.509524149065844,0.588106469511045,
-0.336253383425587));
#56905=CARTESIAN_POINT('Ctrl Pts',(-0.726459163514617,0.278821021102691,
-0.325819420823107));
#56906=CARTESIAN_POINT('Ctrl Pts',(-0.772160923741468,-0.0961851627662938,
-0.315385458220626));
#56907=CARTESIAN_POINT('Ctrl Pts',(-0.635857096320805,-0.44851960007697,
-0.304951495618145));
#56908=CARTESIAN_POINT('Ctrl Pts',(-0.349675772572242,-0.695133750421177,
-0.294517533015665));
#56909=CARTESIAN_POINT('Ctrl Pts',(0.018927415108638,-0.777898343127076,
-0.284083570413184));
#56910=CARTESIAN_POINT('Ctrl Pts',(0.383069238555864,-0.677304980083509,
-0.273649607810704));
#56911=CARTESIAN_POINT('Ctrl Pts',(0.656918030774064,-0.417064473576457,
-0.263215645208223));
#56912=CARTESIAN_POINT('Ctrl Pts',(0.775925088871969,-0.0585179357196898,
-0.252781682605742));
#56913=CARTESIAN_POINT('Ctrl Pts',(0.712039268108792,0.313821801446683,
-0.242347720003261));
#56914=CARTESIAN_POINT('Ctrl Pts',(0.480319179839611,0.612190845510341,
-0.231913757400781));
#56915=CARTESIAN_POINT('Ctrl Pts',(0.135383185403131,0.766260643122266,
-0.2214797947983));
#56916=CARTESIAN_POINT('Ctrl Pts',(-0.241463583105916,0.739715819084738,
-0.21104583219582));
#56917=CARTESIAN_POINT('Ctrl Pts',(-0.561395735813014,0.538812599584084,
-0.200611869593339));
#56918=CARTESIAN_POINT('Ctrl Pts',(-0.749000415068715,0.210907018176785,
-0.190177906990858));
#56919=CARTESIAN_POINT('Ctrl Pts',(-0.760061058523673,-0.166712968918104,
-0.179743944388378));
#56920=CARTESIAN_POINT('Ctrl Pts',(-0.591963437035102,-0.505033917097275,
-0.169309981785897));
#56921=CARTESIAN_POINT('Ctrl Pts',(-0.284343775530124,-0.724319970193128,
-0.158876019183417));
#56922=CARTESIAN_POINT('Ctrl Pts',(0.0903167256721143,-0.772864499431969,
-0.148442056580936));
#56923=CARTESIAN_POINT('Ctrl Pts',(0.443652349415133,-0.639262299658953,
-0.138008093978456));
#56924=CARTESIAN_POINT('Ctrl Pts',(0.692489789754636,-0.354930164383848,
-0.127574131375975));
#56925=CARTESIAN_POINT('Ctrl Pts',(0.749438354901216,-0.109676454265903,
-0.120618156307655));
#56926=CARTESIAN_POINT('Ctrl Pts',(0.747395528060274,0.0124969850565577,
-0.117140168773494));
#56927=CARTESIAN_POINT('Ctrl Pts',(-0.454743647135459,0.595260098846585,
-1.13299148312149));
#56928=CARTESIAN_POINT('Ctrl Pts',(-0.552049078435983,0.520924481859273,
-1.12951349558733));
#56929=CARTESIAN_POINT('Ctrl Pts',(-0.709431880792852,0.323716019874448,
-1.12255752051901));
#56930=CARTESIAN_POINT('Ctrl Pts',(-0.778260040912913,-0.0486194957500408,
-1.11212355791653));
#56931=CARTESIAN_POINT('Ctrl Pts',(-0.663651266471098,-0.409404197277853,
-1.10168959531405));
#56932=CARTESIAN_POINT('Ctrl Pts',(-0.392610989723493,-0.673732890143875,
-1.09125563271157));
#56933=CARTESIAN_POINT('Ctrl Pts',(-0.0290299167445373,-0.779233990024142,
-1.08082167010908));
#56934=CARTESIAN_POINT('Ctrl Pts',(0.341394439427491,-0.701073692506759,
-1.07038770750661));
#56935=CARTESIAN_POINT('Ctrl Pts',(0.631348582478224,-0.457657953570592,
-1.05995374490413));
#56936=CARTESIAN_POINT('Ctrl Pts',(0.772488099658164,-0.106370870957127,
-1.04951978230164));
#56937=CARTESIAN_POINT('Ctrl Pts',(0.731544823668044,0.2699903190294,-1.03908581969916));
#56938=CARTESIAN_POINT('Ctrl Pts',(0.518169599805944,0.582711493978721,
-1.02865185709668));
#56939=CARTESIAN_POINT('Ctrl Pts',(0.182656907952852,0.758082477697758,
-1.0182178944942));
#56940=CARTESIAN_POINT('Ctrl Pts',(-0.195909722819775,0.754766099154425,
-1.00778393189172));
#56941=CARTESIAN_POINT('Ctrl Pts',(-0.528298596051654,0.573544355519819,
-0.997349969289241));
#56942=CARTESIAN_POINT('Ctrl Pts',(-0.736162521039284,0.25713276511868,
-0.98691600668676));
#56943=CARTESIAN_POINT('Ctrl Pts',(-0.77050602107108,-0.119887409454014,
-0.97648204408428));
#56944=CARTESIAN_POINT('Ctrl Pts',(-0.623234008102326,-0.468649007698716,
-0.966048081481799));
#56945=CARTESIAN_POINT('Ctrl Pts',(-0.329059881148497,-0.706945622689529,
-0.955614118879318));
#56946=CARTESIAN_POINT('Ctrl Pts',(0.0426767532874446,-0.778608512204756,
-0.945180156276838));
#56947=CARTESIAN_POINT('Ctrl Pts',(0.404354075695012,-0.666746054432856,
-0.934746193674357));
#56948=CARTESIAN_POINT('Ctrl Pts',(0.670721341414737,-0.397725284812046,
-0.924312231071876));
#56949=CARTESIAN_POINT('Ctrl Pts',(0.778993281877019,-0.0349569263343661,
-0.913878268469396));
#56950=CARTESIAN_POINT('Ctrl Pts',(0.703649182952155,0.336051108064824,
-0.903444305866915));
#56951=CARTESIAN_POINT('Ctrl Pts',(0.462448357003046,0.627848737386998,
-0.893010343264436));
#56952=CARTESIAN_POINT('Ctrl Pts',(0.112244106104245,0.771656517208897,
-0.882576380661953));
#56953=CARTESIAN_POINT('Ctrl Pts',(-0.264417135746447,0.733577602061107,
-0.872142418059474));
#56954=CARTESIAN_POINT('Ctrl Pts',(-0.578752773069474,0.522587550157068,
-0.861708455456993));
#56955=CARTESIAN_POINT('Ctrl Pts',(-0.756670941263008,0.188418700147705,
-0.851274492854512));
#56956=CARTESIAN_POINT('Ctrl Pts',(-0.756234655578183,-0.190162208704721,
-0.840840530252032));
#56957=CARTESIAN_POINT('Ctrl Pts',(-0.577546752652513,-0.523920097359396,
-0.830406567649551));
#56958=CARTESIAN_POINT('Ctrl Pts',(-0.262725650946226,-0.734185094000027,
-0.819972605047071));
#56959=CARTESIAN_POINT('Ctrl Pts',(0.114022356418755,-0.771395762338238,
-0.80953864244459));
#56960=CARTESIAN_POINT('Ctrl Pts',(0.463894222518143,-0.626781198051683,
-0.79910467984211));
#56961=CARTESIAN_POINT('Ctrl Pts',(0.704421859570821,-0.334428413379528,
-0.788670717239629));
#56962=CARTESIAN_POINT('Ctrl Pts',(0.778910642463375,0.0367522920926851,
-0.778236754637147));
#56963=CARTESIAN_POINT('Ctrl Pts',(0.669802864842397,0.399270136831812,
-0.767802792034668));
#56964=CARTESIAN_POINT('Ctrl Pts',(0.402816255551772,0.667676257013847,
-0.757368829432187));
#56965=CARTESIAN_POINT('Ctrl Pts',(0.0408820681867801,0.778704806982432,
-0.746934866829706));
#56966=CARTESIAN_POINT('Ctrl Pts',(-0.330688406958327,0.706185313795279,
-0.736500904227226));
#56967=CARTESIAN_POINT('Ctrl Pts',(-0.624312515974405,0.46721130371009,
-0.726066941624745));
#56968=CARTESIAN_POINT('Ctrl Pts',(-0.770780296177272,0.11811119735931,
-0.715632979022265));
#56969=CARTESIAN_POINT('Ctrl Pts',(-0.735567914914891,-0.258828828503577,
-0.705199016419784));
#56970=CARTESIAN_POINT('Ctrl Pts',(-0.526975261461872,-0.57476046638923,
-0.694765053817304));
#56971=CARTESIAN_POINT('Ctrl Pts',(-0.194169585095039,-0.755215659358831,
-0.684331091214823));
#56972=CARTESIAN_POINT('Ctrl Pts',(0.184403687753781,-0.757659422075368,
-0.673897128612342));
#56973=CARTESIAN_POINT('Ctrl Pts',(0.519511277927458,-0.581515736694161,
-0.663463166009861));
#56974=CARTESIAN_POINT('Ctrl Pts',(0.732165176270938,-0.268303325683674,
-0.653029203407381));
#56975=CARTESIAN_POINT('Ctrl Pts',(0.772240859909324,0.108150701353624,
-0.6425952408049));
#56976=CARTESIAN_POINT('Ctrl Pts',(0.630292113480908,0.459112591420171,
-0.632161278202419));
#56977=CARTESIAN_POINT('Ctrl Pts',(0.339777590896286,0.701857327839134,
-0.621727315599939));
#56978=CARTESIAN_POINT('Ctrl Pts',(-0.0308257039136614,0.779167694334796,
-0.611293352997458));
#56979=CARTESIAN_POINT('Ctrl Pts',(-0.394163090536686,0.672820910774436,
-0.600859390394977));
#56980=CARTESIAN_POINT('Ctrl Pts',(-0.664592531422761,0.407883913747357,
-0.590425427792498));
#56981=CARTESIAN_POINT('Ctrl Pts',(-0.778371265205501,0.0468048439711131,
-0.579991465190016));
#56982=CARTESIAN_POINT('Ctrl Pts',(-0.708680574764765,-0.325306567514176,
-0.569557502587537));
#56983=CARTESIAN_POINT('Ctrl Pts',(-0.471947210958991,-0.620740163018959,
-0.559123539985055));
#56984=CARTESIAN_POINT('Ctrl Pts',(-0.123971453029556,-0.769859466883739,
-0.548689577382575));
#56985=CARTESIAN_POINT('Ctrl Pts',(0.25322554176231,-0.737515657403934,
-0.538255614780094));
#56986=CARTESIAN_POINT('Ctrl Pts',(0.570734895935091,-0.531332474519237,
-0.527821652177614));
#56987=CARTESIAN_POINT('Ctrl Pts',(0.753716669989903,-0.199909232643481,
-0.517387689575133));
#56988=CARTESIAN_POINT('Ctrl Pts',(0.759040339677032,0.17863449459651,-0.506953726972652));
#56989=CARTESIAN_POINT('Ctrl Pts',(0.585451066006504,0.515072392221348,
-0.496519764370172));
#56990=CARTESIAN_POINT('Ctrl Pts',(0.273865472594036,0.730102885104296,
-0.486085801767691));
#56991=CARTESIAN_POINT('Ctrl Pts',(-0.102272787158508,0.773041264696528,
-0.475651839165211));
#56992=CARTESIAN_POINT('Ctrl Pts',(-0.45430438957095,0.633766551289465,
-0.46521787656273));
#56993=CARTESIAN_POINT('Ctrl Pts',(-0.699252176710743,0.345107104073574,
-0.45478391396025));
#56994=CARTESIAN_POINT('Ctrl Pts',(-0.77937965253776,-0.0248973317232137,
-0.444349951357768));
#56995=CARTESIAN_POINT('Ctrl Pts',(-0.675800017767713,-0.389033232387461,
-0.433915988755288));
#56996=CARTESIAN_POINT('Ctrl Pts',(-0.412927966007995,-0.661470343103489,
-0.423482026152807));
#56997=CARTESIAN_POINT('Ctrl Pts',(-0.0527249109646674,-0.777992675852613,
-0.413048063550327));
#56998=CARTESIAN_POINT('Ctrl Pts',(0.319905901228363,-0.711134821448211,
-0.402614100947846));
#56999=CARTESIAN_POINT('Ctrl Pts',(0.617131885254587,-0.476655804663405,
-0.392180138345366));
#57000=CARTESIAN_POINT('Ctrl Pts',(0.768894082626004,-0.129824533958293,
-0.381746175742885));
#57001=CARTESIAN_POINT('Ctrl Pts',(0.739420716803659,0.247607599809944,
-0.371312213140405));
#57002=CARTESIAN_POINT('Ctrl Pts',(0.535658937155231,0.566676294679631,
-0.360878250537924));
#57003=CARTESIAN_POINT('Ctrl Pts',(0.205637310626131,0.752174059916795,
-0.350444287935443));
#57004=CARTESIAN_POINT('Ctrl Pts',(-0.172854963141739,0.760377328448251,
-0.340010325332963));
#57005=CARTESIAN_POINT('Ctrl Pts',(-0.510603697094482,0.589352512866214,
-0.329576362730482));
#57006=CARTESIAN_POINT('Ctrl Pts',(-0.727998339939051,0.279411769712721,
-0.319142400128002));
#57007=CARTESIAN_POINT('Ctrl Pts',(-0.773796930208484,-0.0963889538944966,
-0.308708437525521));
#57008=CARTESIAN_POINT('Ctrl Pts',(-0.6372043107291,-0.449469895473673,
-0.29827447492304));
#57009=CARTESIAN_POINT('Ctrl Pts',(-0.350416643817236,-0.69660655649887,
-0.28784051232056));
#57010=CARTESIAN_POINT('Ctrl Pts',(0.0189675173356873,-0.779546505705978,
-0.277406549718079));
#57011=CARTESIAN_POINT('Ctrl Pts',(0.383880861799198,-0.678740011636774,
-0.266972587115598));
#57012=CARTESIAN_POINT('Ctrl Pts',(0.658309867773886,-0.417948123900588,
-0.256538624513118));
#57013=CARTESIAN_POINT('Ctrl Pts',(0.777569070626036,-0.0586419196868113,
-0.246104661910637));
#57014=CARTESIAN_POINT('Ctrl Pts',(0.71354789254065,0.314486707157718,-0.235670699308157));
#57015=CARTESIAN_POINT('Ctrl Pts',(0.481336850230815,0.613487918075936,
-0.225236736705676));
#57016=CARTESIAN_POINT('Ctrl Pts',(0.135670026800068,0.767884146994866,
-0.214802774103195));
#57017=CARTESIAN_POINT('Ctrl Pts',(-0.24197518098053,0.741283085733479,
-0.204368811500715));
#57018=CARTESIAN_POINT('Ctrl Pts',(-0.562585186373488,0.539954196552602,
-0.193934848898234));
#57019=CARTESIAN_POINT('Ctrl Pts',(-0.750587350010887,0.211353885858101,
-0.183500886295754));
#57020=CARTESIAN_POINT('Ctrl Pts',(-0.761671429498338,-0.167066211673786,
-0.173066923693273));
#57021=CARTESIAN_POINT('Ctrl Pts',(-0.59321765042596,-0.506103908795656,
-0.162632961090792));
#57022=CARTESIAN_POINT('Ctrl Pts',(-0.284946229083329,-0.725854698300198,
-0.152198998488312));
#57023=CARTESIAN_POINT('Ctrl Pts',(0.0905080903716103,-0.774501830736828,
-0.141765035885831));
#57024=CARTESIAN_POINT('Ctrl Pts',(0.444592317906142,-0.640617059956728,
-0.131331073283351));
#57025=CARTESIAN_POINT('Ctrl Pts',(0.693957024835477,-0.35568146239315,
-0.12089711068087));
#57026=CARTESIAN_POINT('Ctrl Pts',(0.751026167303855,-0.109909948718264,
-0.11394113561255));
#57027=CARTESIAN_POINT('Ctrl Pts',(0.748978993560761,0.012523461726479,
-0.110463148078389));
#57028=CARTESIAN_POINT('Ctrl Pts',(-0.457725546467597,0.599163409431307,
-1.12801069747057));
#57029=CARTESIAN_POINT('Ctrl Pts',(-0.555667179198615,0.524341772031445,
-1.12453270993641));
#57030=CARTESIAN_POINT('Ctrl Pts',(-0.714084824405274,0.325837708337138,
-1.11757673486809));
#57031=CARTESIAN_POINT('Ctrl Pts',(-0.783362670351873,-0.0489378503027498,
-1.10714277226561));
#57032=CARTESIAN_POINT('Ctrl Pts',(-0.668003172418794,-0.412088937642732,
-1.09670880966312));
#57033=CARTESIAN_POINT('Ctrl Pts',(-0.395185257636937,-0.67815052788145,
-1.08627484706065));
#57034=CARTESIAN_POINT('Ctrl Pts',(-0.0292203366733351,-0.784343583971593,
-1.07584088445816));
#57035=CARTESIAN_POINT('Ctrl Pts',(0.343633040095591,-0.705670692032951,
-1.06540692185568));
#57036=CARTESIAN_POINT('Ctrl Pts',(0.635488397768254,-0.460658889708482,
-1.0549729592532));
#57037=CARTESIAN_POINT('Ctrl Pts',(0.777553410767087,-0.107068350619836,
-1.04453899665072));
#57038=CARTESIAN_POINT('Ctrl Pts',(0.736341651251885,0.271760675877952,
-1.03410503404824));
#57039=CARTESIAN_POINT('Ctrl Pts',(0.521567305771502,0.586532409010019,
-1.02367107144576));
#57040=CARTESIAN_POINT('Ctrl Pts',(0.183854611276035,0.763053319515687,
-1.01323710884328));
#57041=CARTESIAN_POINT('Ctrl Pts',(-0.197194327096822,0.759715196564629,
-1.0028031462408));
#57042=CARTESIAN_POINT('Ctrl Pts',(-0.531762717152964,0.577305158239887,
-0.99236918363832));
#57043=CARTESIAN_POINT('Ctrl Pts',(-0.740989631772395,0.258818817356293,
-0.981935221035839));
#57044=CARTESIAN_POINT('Ctrl Pts',(-0.775558326712227,-0.12067352644806,
-0.971501258433358));
#57045=CARTESIAN_POINT('Ctrl Pts',(-0.627320632386313,-0.471721998562319,
-0.961067295830878));
#57046=CARTESIAN_POINT('Ctrl Pts',(-0.331217568484237,-0.711581154688746,
-0.950633333228397));
#57047=CARTESIAN_POINT('Ctrl Pts',(0.0429565901738399,-0.783713946820615,
-0.940199370625917));
#57048=CARTESIAN_POINT('Ctrl Pts',(0.407005476575287,-0.671117992759011,
-0.929765408023434));
#57049=CARTESIAN_POINT('Ctrl Pts',(0.675119346199268,-0.400333219873854,
-0.919331445420956));
#57050=CARTESIAN_POINT('Ctrl Pts',(0.784101239483766,-0.035186143328752,
-0.908897482818474));
#57051=CARTESIAN_POINT('Ctrl Pts',(0.70826309976199,0.338254637741563,-0.898463520215994));
#57052=CARTESIAN_POINT('Ctrl Pts',(0.465480689448246,0.631965621074233,
-0.888029557613513));
#57053=CARTESIAN_POINT('Ctrl Pts',(0.112980104923762,0.776716366721998,
-0.877595595011033));
#57054=CARTESIAN_POINT('Ctrl Pts',(-0.266150952393821,0.738387763304697,
-0.867161632408552));
#57055=CARTESIAN_POINT('Ctrl Pts',(-0.582547728300969,0.526014222908736,
-0.856727669806072));
#57056=CARTESIAN_POINT('Ctrl Pts',(-0.761632528456596,0.189654185427614,
-0.846293707203591));
#57057=CARTESIAN_POINT('Ctrl Pts',(-0.761193381991244,-0.191409126391062,
-0.83585974460111));
#57058=CARTESIAN_POINT('Ctrl Pts',(-0.581333799855445,-0.527355507791801,
-0.825425781998629));
#57059=CARTESIAN_POINT('Ctrl Pts',(-0.264448376313448,-0.738999238645272,
-0.81499181939615));
#57060=CARTESIAN_POINT('Ctrl Pts',(0.114770015450621,-0.776453902048481,
-0.804557856793668));
#57061=CARTESIAN_POINT('Ctrl Pts',(0.466936035686987,-0.630891081748588,
-0.794123894191188));
#57062=CARTESIAN_POINT('Ctrl Pts',(0.709040842918429,-0.33662130284112,
-0.783689931588706));
#57063=CARTESIAN_POINT('Ctrl Pts',(0.784018058194349,0.0369932815265828,
-0.773255968986227));
#57064=CARTESIAN_POINT('Ctrl Pts',(0.674194847057106,0.401888201686226,
-0.762822006383745));
#57065=CARTESIAN_POINT('Ctrl Pts',(0.405457572755745,0.672054294791692,
-0.752388043781266));
#57066=CARTESIAN_POINT('Ctrl Pts',(0.0411501370855586,0.783810873024088,
-0.741954081178784));
#57067=CARTESIAN_POINT('Ctrl Pts',(-0.332856772724146,0.710815860335577,
-0.731520118576304));
#57068=CARTESIAN_POINT('Ctrl Pts',(-0.628406212210275,0.470274867400415,
-0.721086155973823));
#57069=CARTESIAN_POINT('Ctrl Pts',(-0.775834400197946,0.118885667439073,
-0.710652193371343));
#57070=CARTESIAN_POINT('Ctrl Pts',(-0.74039112689201,-0.260526001912516,
-0.700218230768863));
#57071=CARTESIAN_POINT('Ctrl Pts',(-0.530430704992227,-0.578529243560247,
-0.689784268166381));
#57072=CARTESIAN_POINT('Ctrl Pts',(-0.195442779655913,-0.760167704084639,
-0.679350305563902));
#57073=CARTESIAN_POINT('Ctrl Pts',(0.185612846088945,-0.762627490862809,
-0.66891634296142));
#57074=CARTESIAN_POINT('Ctrl Pts',(0.52291777917247,-0.585328809028116,
-0.65848238035894));
#57075=CARTESIAN_POINT('Ctrl Pts',(0.736966076059816,-0.27006262457056,
-0.648048417756459));
#57076=CARTESIAN_POINT('Ctrl Pts',(0.777304541031368,0.10885985919959,-0.637614455153979));
#57077=CARTESIAN_POINT('Ctrl Pts',(0.634425018694938,0.462123050828315,
-0.627180492551498));
#57078=CARTESIAN_POINT('Ctrl Pts',(0.342005555592323,0.706459495227383,
-0.616746529949017));
#57079=CARTESIAN_POINT('Ctrl Pts',(-0.0310278319582717,0.784276795587445,
-0.606312567346537));
#57080=CARTESIAN_POINT('Ctrl Pts',(-0.396747667841739,0.677232682698555,
-0.595878604744056));
#57081=CARTESIAN_POINT('Ctrl Pts',(-0.668950348821354,0.410558460227934,
-0.585444642141576));
#57082=CARTESIAN_POINT('Ctrl Pts',(-0.783475144171483,0.0471117492608237,
-0.575010679539095));
#57083=CARTESIAN_POINT('Ctrl Pts',(-0.713327483047262,-0.327439643877154,
-0.564576716936614));
#57084=CARTESIAN_POINT('Ctrl Pts',(-0.475041828592944,-0.624810434884064,
-0.554142754334134));
#57085=CARTESIAN_POINT('Ctrl Pts',(-0.124784349547945,-0.774907532910113,
-0.543708791731654));
#57086=CARTESIAN_POINT('Ctrl Pts',(0.254885973710435,-0.742351640975235,
-0.533274829129173));
#57087=CARTESIAN_POINT('Ctrl Pts',(0.574477276930804,-0.534816488847445,
-0.522840866526692));
#57088=CARTESIAN_POINT('Ctrl Pts',(0.758658885652574,-0.201220062800251,
-0.512406903924211));
#57089=CARTESIAN_POINT('Ctrl Pts',(0.764017463316078,0.179805823601479,
-0.501972941321731));
#57090=CARTESIAN_POINT('Ctrl Pts',(0.589289942793166,0.518449787130605,
-0.49153897871925));
#57091=CARTESIAN_POINT('Ctrl Pts',(0.275661243182654,0.734890262188806,
-0.48110501611677));
#57092=CARTESIAN_POINT('Ctrl Pts',(-0.102943402776664,0.778110194174132,
-0.470671053514289));
#57093=CARTESIAN_POINT('Ctrl Pts',(-0.457283320990613,0.63792223883224,
-0.460237090911809));
#57094=CARTESIAN_POINT('Ctrl Pts',(-0.703837261793103,0.347370015062493,
-0.449803128309327));
#57095=CARTESIAN_POINT('Ctrl Pts',(-0.78449014362719,-0.0250605866805469,
-0.439369165706848));
#57096=CARTESIAN_POINT('Ctrl Pts',(-0.680231324073688,-0.391584172562941,
-0.428935203104366));
#57097=CARTESIAN_POINT('Ctrl Pts',(-0.415635586978069,-0.665807687917846,
-0.418501240501886));
#57098=CARTESIAN_POINT('Ctrl Pts',(-0.0530706348834263,-0.783094072360267,
-0.408067277899405));
#57099=CARTESIAN_POINT('Ctrl Pts',(0.322003564738517,-0.715797822537025,
-0.397633315296925));
#57100=CARTESIAN_POINT('Ctrl Pts',(0.621178497185405,-0.479781297142647,
-0.387199352694444));
#57101=CARTESIAN_POINT('Ctrl Pts',(0.773935818505537,-0.13067580986956,
-0.376765390091964));
#57102=CARTESIAN_POINT('Ctrl Pts',(0.744269192090712,0.249231194201064,
-0.366331427489483));
#57103=CARTESIAN_POINT('Ctrl Pts',(0.539171320646896,0.570392062913125,
-0.355897464887002));
#57104=CARTESIAN_POINT('Ctrl Pts',(0.206985700515669,0.757106160489393,
-0.345463502284522));
#57105=CARTESIAN_POINT('Ctrl Pts',(-0.173988395026948,0.765363218892889,
-0.335029539682041));
#57106=CARTESIAN_POINT('Ctrl Pts',(-0.513951790203912,0.593216971932297,
-0.324595577079561));
#57107=CARTESIAN_POINT('Ctrl Pts',(-0.732771917254223,0.28124390807743,
-0.31416161447708));
#57108=CARTESIAN_POINT('Ctrl Pts',(-0.778870814680851,-0.0970209884795471,
-0.3037276518746));
#57109=CARTESIAN_POINT('Ctrl Pts',(-0.641382540095327,-0.452417126489898,
-0.293293689272119));
#57110=CARTESIAN_POINT('Ctrl Pts',(-0.352714370131851,-0.701174293940722,
-0.282859726669638));
#57111=CARTESIAN_POINT('Ctrl Pts',(0.0190918897513369,-0.784658090821038,
-0.272425764067158));
#57112=CARTESIAN_POINT('Ctrl Pts',(0.386398017223737,-0.68319059595668,
-0.261991801464677));
#57113=CARTESIAN_POINT('Ctrl Pts',(0.662626488959991,-0.420688662481479,
-0.251557838862196));
#57114=CARTESIAN_POINT('Ctrl Pts',(0.782667689483343,-0.0590264425752508,
-0.241123876259716));
#57115=CARTESIAN_POINT('Ctrl Pts',(0.718226716476131,0.316548837101509,
-0.230689913657235));
#57116=CARTESIAN_POINT('Ctrl Pts',(0.484493036851988,0.617510634526491,
-0.220255951054755));
#57117=CARTESIAN_POINT('Ctrl Pts',(0.136559632479484,0.772919263601256,
-0.209821988452274));
#57118=CARTESIAN_POINT('Ctrl Pts',(-0.243561843146326,0.746143766900964,
-0.199388025849794));
#57119=CARTESIAN_POINT('Ctrl Pts',(-0.566274128183453,0.543494756230501,
-0.188954063247313));
#57120=CARTESIAN_POINT('Ctrl Pts',(-0.75550904732574,0.212739737177773,
-0.178520100644832));
#57121=CARTESIAN_POINT('Ctrl Pts',(-0.766665803559575,-0.168161640964736,
-0.168086138042352));
#57122=CARTESIAN_POINT('Ctrl Pts',(-0.597107457561111,-0.509422584813054,
-0.157652175439871));
#57123=CARTESIAN_POINT('Ctrl Pts',(-0.286814649975467,-0.730614045087357,
-0.14721821283739));
#57124=CARTESIAN_POINT('Ctrl Pts',(0.0911015483498812,-0.779580681377717,
-0.13678425023491));
#57125=CARTESIAN_POINT('Ctrl Pts',(0.447507596061856,-0.644816980204467,
-0.126350287632429));
#57126=CARTESIAN_POINT('Ctrl Pts',(0.698507324942254,-0.358015175128548,
-0.115916325029948));
#57127=CARTESIAN_POINT('Ctrl Pts',(0.755950846588164,-0.110628321320808,
-0.108960349961628));
#57128=CARTESIAN_POINT('Ctrl Pts',(0.753890288033488,0.0126055820648136,
-0.105482362427468));
#57129=CARTESIAN_POINT('Ctrl Pts',(-0.459778808448974,0.601851132366397,
-1.12625));
#57130=CARTESIAN_POINT('Ctrl Pts',(-0.558161082255848,0.52669287114394,
-1.12277201246584));
#57131=CARTESIAN_POINT('Ctrl Pts',(-0.717287384517956,0.32730005915496,
-1.11581603739752));
#57132=CARTESIAN_POINT('Ctrl Pts',(-0.786877139371749,-0.0491576947563774,
-1.10538207479504));
#57133=CARTESIAN_POINT('Ctrl Pts',(-0.670999603978847,-0.413937381459674,
-1.09494811219256));
#57134=CARTESIAN_POINT('Ctrl Pts',(-0.396958121390906,-0.681192740453029,
-1.08451414959008));
#57135=CARTESIAN_POINT('Ctrl Pts',(-0.0293513702614997,-0.787862050964758,
-1.0740801869876));
#57136=CARTESIAN_POINT('Ctrl Pts',(0.345174528791172,-0.708836299099991,
-1.06364622438512));
#57137=CARTESIAN_POINT('Ctrl Pts',(0.638339163802785,-0.46272536101763,
-1.05321226178264));
#57138=CARTESIAN_POINT('Ctrl Pts',(0.78104145176708,-0.107548656621837,
-1.04277829918016));
#57139=CARTESIAN_POINT('Ctrl Pts',(0.739644828584922,0.272979776873327,
-1.03234433657767));
#57140=CARTESIAN_POINT('Ctrl Pts',(0.523907016570379,0.589163548674698,
-1.02191037397519));
#57141=CARTESIAN_POINT('Ctrl Pts',(0.184679370276396,0.766476320999639,
-1.01147641137271));
#57142=CARTESIAN_POINT('Ctrl Pts',(-0.198078926680867,0.763123222427558,
-1.00104244877023));
#57143=CARTESIAN_POINT('Ctrl Pts',(-0.53414816518828,0.579894906686743,
-0.990608486167753));
#57144=CARTESIAN_POINT('Ctrl Pts',(-0.74431365659454,0.259979859348694,
-0.980174523565271));
#57145=CARTESIAN_POINT('Ctrl Pts',(-0.779037423985492,-0.121214858921556,
-0.969740560962791));
#57146=CARTESIAN_POINT('Ctrl Pts',(-0.63013474640097,-0.473838108603285,
-0.95930659836031));
#57147=CARTESIAN_POINT('Ctrl Pts',(-0.332703386000087,-0.714773255138959,
-0.94887263575783));
#57148=CARTESIAN_POINT('Ctrl Pts',(0.0431492902551101,-0.78722962966257,
-0.938438673155349));
#57149=CARTESIAN_POINT('Ctrl Pts',(0.40883127306227,-0.674128578464592,
-0.928004710552868));
#57150=CARTESIAN_POINT('Ctrl Pts',(0.678147881681891,-0.40212908510846,
-0.917570747950388));
#57151=CARTESIAN_POINT('Ctrl Pts',(0.787618659686819,-0.0353439857660817,
-0.907136785347908));
#57152=CARTESIAN_POINT('Ctrl Pts',(0.711440315674566,0.339772023043391,
-0.896702822745426));
#57153=CARTESIAN_POINT('Ctrl Pts',(0.467568801414541,0.634800572137749,
-0.886268860142948));
#57154=CARTESIAN_POINT('Ctrl Pts',(0.113486925323209,0.78020065893068,-0.875834897540464));
#57155=CARTESIAN_POINT('Ctrl Pts',(-0.267344885893191,0.741700116231731,
-0.865400934937986));
#57156=CARTESIAN_POINT('Ctrl Pts',(-0.58516099435014,0.528373883831429,
-0.854966972335504));
#57157=CARTESIAN_POINT('Ctrl Pts',(-0.765049155681855,0.190504960084841,
-0.844533009733024));
#57158=CARTESIAN_POINT('Ctrl Pts',(-0.764608039237945,-0.192267773583724,
-0.834099047130543));
#57159=CARTESIAN_POINT('Ctrl Pts',(-0.583941620311303,-0.52972118561936,
-0.823665084528063));
#57160=CARTESIAN_POINT('Ctrl Pts',(-0.265634672182434,-0.742314334605434,
-0.813231121925582));
#57161=CARTESIAN_POINT('Ctrl Pts',(0.11528486525651,-0.77993701686014,-0.802797159323101));
#57162=CARTESIAN_POINT('Ctrl Pts',(0.469030676228696,-0.633721212507912,
-0.792363196720621));
#57163=CARTESIAN_POINT('Ctrl Pts',(0.712221547729785,-0.338131361123721,
-0.781929234118141));
#57164=CARTESIAN_POINT('Ctrl Pts',(0.787535105251362,0.0371592306530882,
-0.77149527151566));
#57165=CARTESIAN_POINT('Ctrl Pts',(0.67721923530673,0.403691042452732,-0.761061308913179));
#57166=CARTESIAN_POINT('Ctrl Pts',(0.407276425457032,0.675069080682076,
-0.750627346310698));
#57167=CARTESIAN_POINT('Ctrl Pts',(0.0413347335588412,0.787326990663742,
-0.740193383708218));
#57168=CARTESIAN_POINT('Ctrl Pts',(-0.334349943602905,0.714004527743863,
-0.729759421105736));
#57169=CARTESIAN_POINT('Ctrl Pts',(-0.631225196028521,0.472384485694395,
-0.719325458503257));
#57170=CARTESIAN_POINT('Ctrl Pts',(-0.779314735970098,0.119418979755566,
-0.708891495900776));
#57171=CARTESIAN_POINT('Ctrl Pts',(-0.743712466759962,-0.261694702299868,
-0.698457533298295));
#57172=CARTESIAN_POINT('Ctrl Pts',(-0.532810177927122,-0.581124482983871,
-0.688023570695815));
#57173=CARTESIAN_POINT('Ctrl Pts',(-0.196319521518959,-0.763577760216057,
-0.677589608093334));
#57174=CARTESIAN_POINT('Ctrl Pts',(0.186445491596607,-0.766048581415893,
-0.667155645490853));
#57175=CARTESIAN_POINT('Ctrl Pts',(0.525263549677469,-0.587954550799829,
-0.656721682888373));
#57176=CARTESIAN_POINT('Ctrl Pts',(0.740272051402902,-0.271274105542238,
-0.646287720285892));
#57177=CARTESIAN_POINT('Ctrl Pts',(0.780791471746631,0.109348196481395,
-0.635853757683412));
#57178=CARTESIAN_POINT('Ctrl Pts',(0.637271002434184,0.464196100675709,
-0.625419795080931));
#57179=CARTESIAN_POINT('Ctrl Pts',(0.34353976723478,0.709628620303801,-0.614985832478451));
#57180=CARTESIAN_POINT('Ctrl Pts',(-0.0311670205189606,0.787795003321278,
-0.604551869875969));
#57181=CARTESIAN_POINT('Ctrl Pts',(-0.39852744855339,0.68027069845432,-0.594117907273489));
#57182=CARTESIAN_POINT('Ctrl Pts',(-0.671951210639548,0.41240019513338,
-0.583683944671008));
#57183=CARTESIAN_POINT('Ctrl Pts',(-0.78698975575632,0.0473230890856614,
-0.573249982068528));
#57184=CARTESIAN_POINT('Ctrl Pts',(-0.716527417409383,-0.328908513916321,
-0.562816019466047));
#57185=CARTESIAN_POINT('Ctrl Pts',(-0.477172831122476,-0.627613288311015,
-0.552382056863567));
#57186=CARTESIAN_POINT('Ctrl Pts',(-0.125344122916367,-0.778383710824121,
-0.541948094261087));
#57187=CARTESIAN_POINT('Ctrl Pts',(0.256029373348164,-0.745681775564449,
-0.531514131658606));
#57188=CARTESIAN_POINT('Ctrl Pts',(0.577054339531638,-0.537215636084532,
-0.521080169056125));
#57189=CARTESIAN_POINT('Ctrl Pts',(0.762062173336032,-0.202122721128445,
-0.510646206453644));
#57190=CARTESIAN_POINT('Ctrl Pts',(0.767444789182846,0.180612419235498,
-0.500212243851164));
#57191=CARTESIAN_POINT('Ctrl Pts',(0.591933453918155,0.520775514553564,
-0.489778281248683));
#57192=CARTESIAN_POINT('Ctrl Pts',(0.276897839143596,0.738186925584304,
-0.479344318646203));
#57193=CARTESIAN_POINT('Ctrl Pts',(-0.103405199272281,0.781600738989842,
-0.468910356043722));
#57194=CARTESIAN_POINT('Ctrl Pts',(-0.459334660167692,0.640783910842519,
-0.458476393441241));
#57195=CARTESIAN_POINT('Ctrl Pts',(-0.706994623724163,0.34892829127361,
-0.448042430838761));
#57196=CARTESIAN_POINT('Ctrl Pts',(-0.78800930842456,-0.0251730066200001,
-0.43760846823628));
#57197=CARTESIAN_POINT('Ctrl Pts',(-0.683282791513013,-0.393340790216438,
-0.4271745056338));
#57198=CARTESIAN_POINT('Ctrl Pts',(-0.417500097498832,-0.668794451991525,
-0.416740543031318));
#57199=CARTESIAN_POINT('Ctrl Pts',(-0.0533087058287059,-0.786606974485122,
-0.406306580428839));
#57200=CARTESIAN_POINT('Ctrl Pts',(0.323448048928484,-0.719008838659507,
-0.395872617826358));
#57201=CARTESIAN_POINT('Ctrl Pts',(0.623965058008301,-0.481933560577747,
-0.385438655223877));
#57202=CARTESIAN_POINT('Ctrl Pts',(0.777407637380551,-0.131262011893549,
-0.375004692621397));
#57203=CARTESIAN_POINT('Ctrl Pts',(0.747607928672496,0.250349226915978,
-0.364570730018916));
#57204=CARTESIAN_POINT('Ctrl Pts',(0.541590003337533,0.57295079954568,-0.354136767416435));
#57205=CARTESIAN_POINT('Ctrl Pts',(0.207914223068492,0.760502482762858,
-0.343702804813955));
#57206=CARTESIAN_POINT('Ctrl Pts',(-0.174768894106414,0.768796581719081,
-0.333268842211474));
#57207=CARTESIAN_POINT('Ctrl Pts',(-0.51625733994508,0.595878099420951,
-0.322834879608994));
#57208=CARTESIAN_POINT('Ctrl Pts',(-0.736059077911031,0.282505547458036,
-0.312400917006513));
#57209=CARTESIAN_POINT('Ctrl Pts',(-0.782364771583724,-0.0974562174576689,
-0.301966954404032));
#57210=CARTESIAN_POINT('Ctrl Pts',(-0.644259734761704,-0.454446636287435,
-0.291532991801552));
#57211=CARTESIAN_POINT('Ctrl Pts',(-0.354296620723973,-0.704319709976542,
-0.281099029199071));
#57212=CARTESIAN_POINT('Ctrl Pts',(0.0191775345559786,-0.788178009053098,
-0.270665066596591));
#57213=CARTESIAN_POINT('Ctrl Pts',(0.388131370170823,-0.686255338400107,
-0.26023110399411));
#57214=CARTESIAN_POINT('Ctrl Pts',(0.665598982404196,-0.422575840864808,
-0.24979714139163));
#57215=CARTESIAN_POINT('Ctrl Pts',(0.786178678898117,-0.0592912305593693,
-0.239363178789148));
#57216=CARTESIAN_POINT('Ctrl Pts',(0.721448628413698,0.317968851246876,
-0.228929216186668));
#57217=CARTESIAN_POINT('Ctrl Pts',(0.486666436849563,0.620280742650438,
-0.218495253584187));
#57218=CARTESIAN_POINT('Ctrl Pts',(0.137172228805453,0.776386520196726,
-0.208061290981707));
#57219=CARTESIAN_POINT('Ctrl Pts',(-0.244654443391746,0.749490916798133,
-0.197627328379226));
#57220=CARTESIAN_POINT('Ctrl Pts',(-0.568814392418841,0.545932825443547,
-0.187193365776746));
#57221=CARTESIAN_POINT('Ctrl Pts',(-0.758898204371725,0.213694087832833,
-0.176759403174265));
#57222=CARTESIAN_POINT('Ctrl Pts',(-0.770105011053623,-0.168916032981121,
-0.166325440571785));
#57223=CARTESIAN_POINT('Ctrl Pts',(-0.599786034786049,-0.511707755229732,
-0.155891477969304));
#57224=CARTESIAN_POINT('Ctrl Pts',(-0.288101284597228,-0.733891647041669,
-0.145457515366823));
#57225=CARTESIAN_POINT('Ctrl Pts',(0.0915102336223925,-0.783077583290337,
-0.135023552764343));
#57226=CARTESIAN_POINT('Ctrl Pts',(0.449515061170523,-0.647710059517752,
-0.124589590161862));
#57227=CARTESIAN_POINT('Ctrl Pts',(0.701640821699951,-0.359620185801168,
-0.114155627559381));
#57228=CARTESIAN_POINT('Ctrl Pts',(0.759341912736313,-0.111126206723813,
-0.107199652491061));
#57229=CARTESIAN_POINT('Ctrl Pts',(0.757272083693561,0.0126621280946486,
-0.103721664956901));
#57230=CARTESIAN_POINT('Ctrl Pts',(0.555007866453738,-0.515351924808612,
-0.12));
#57231=CARTESIAN_POINT('Ctrl Pts',(0.591072083605962,-0.472049785910241,
-0.12));
#57232=CARTESIAN_POINT('Ctrl Pts',(0.641266713589833,-0.405214104043363,
-0.12));
#57233=CARTESIAN_POINT('Ctrl Pts',(0.703252213124767,-0.263984626534931,
-0.12));
#57234=CARTESIAN_POINT('Ctrl Pts',(0.719761895146739,-0.212714660677385,
-0.12));
#57235=CARTESIAN_POINT('Ctrl Pts',(0.742808661707171,-0.103336683918306,
-0.12));
#57236=CARTESIAN_POINT('Ctrl Pts',(0.748364886323481,-0.0454765203713869,
-0.12));
#57237=CARTESIAN_POINT('Ctrl Pts',(0.747395528060274,0.0124969850565566,
-0.12));
#57238=CARTESIAN_POINT('',(-0.738674446606902,0.114170753859872,-1.12625));
#57239=CARTESIAN_POINT('Ctrl Pts',(-0.738728321778976,0.114178441930245,
-1.12625));
#57240=CARTESIAN_POINT('Ctrl Pts',(-0.729872306490505,0.171476380149593,
-1.12625));
#57241=CARTESIAN_POINT('Ctrl Pts',(-0.714604763127107,0.227558322531754,
-1.12625));
#57242=CARTESIAN_POINT('Ctrl Pts',(-0.673382241080463,0.331452140304371,
-1.12625));
#57243=CARTESIAN_POINT('Ctrl Pts',(-0.648435827358875,0.379185799077549,
-1.12625));
#57244=CARTESIAN_POINT('Ctrl Pts',(-0.563441537104104,0.507894222797762,
-1.12625));
#57245=CARTESIAN_POINT('Ctrl Pts',(-0.502653830377742,0.565275533421067,
-1.12625));
#57246=CARTESIAN_POINT('Ctrl Pts',(-0.459778808448976,0.601851132366395,
-1.12625));
#57247=CARTESIAN_POINT('Ctrl Pts',(-0.73867444479349,0.114170753601095,
-1.12625));
#57248=CARTESIAN_POINT('Ctrl Pts',(-0.744523251396961,0.0764015856923683,
-1.12516243468899));
#57249=CARTESIAN_POINT('Ctrl Pts',(-0.747504748693495,0.0381902463136735,
-1.12407486937799));
#57250=CARTESIAN_POINT('Ctrl Pts',(-0.747536615034749,-1.54000427278079E-5,
-1.12298730406698));
#57251=CARTESIAN_POINT('Origin',(-9.99409214431492E-17,0.,-1.12625));
#57252=CARTESIAN_POINT('',(-0.82685,-1.01259920587499E-16,-1.12625));
#57253=CARTESIAN_POINT('Origin',(0.,0.,-1.12625));
#57254=CARTESIAN_POINT('Origin',(0.,0.,-1.12625));
#57255=CARTESIAN_POINT('',(0.589301091561366,-0.565833523687262,-1.12625));
#57256=CARTESIAN_POINT('Ctrl Pts',(0.82685,-1.28508315100362E-14,-1.12625));
#57257=CARTESIAN_POINT('Ctrl Pts',(0.826849999999999,-0.0640849384885683,
-1.12625));
#57258=CARTESIAN_POINT('Ctrl Pts',(0.819177389464159,-0.127972397977417,
-1.12625));
#57259=CARTESIAN_POINT('Ctrl Pts',(0.789918090291951,-0.247778859616496,
-1.12625));
#57260=CARTESIAN_POINT('Ctrl Pts',(0.769494724754838,-0.303642805552855,
-1.12625));
#57261=CARTESIAN_POINT('Ctrl Pts',(0.695180543122699,-0.452454840062382,
-1.12625));
#57262=CARTESIAN_POINT('Ctrl Pts',(0.63618267061235,-0.521654825860835,
-1.12625));
#57263=CARTESIAN_POINT('Ctrl Pts',(0.589301091561366,-0.565833523687262,
-1.12625));
#57264=CARTESIAN_POINT('',(-0.459778808448989,-0.601851132366385,-1.12625));
#57265=CARTESIAN_POINT('Ctrl Pts',(0.589349009255739,-0.565869316348666,
-1.12625));
#57266=CARTESIAN_POINT('Ctrl Pts',(0.561797955794756,-0.591801457111598,
-1.12625));
#57267=CARTESIAN_POINT('Ctrl Pts',(0.53250376759911,-0.61571900169366,-1.12625));
#57268=CARTESIAN_POINT('Ctrl Pts',(0.501718244977289,-0.637497823098473,
-1.12625));
#57269=CARTESIAN_POINT('Ctrl Pts',(0.471023065979674,-0.659212732070133,
-1.12625));
#57270=CARTESIAN_POINT('Ctrl Pts',(0.438844183868204,-0.67880200460138,
-1.12625));
#57271=CARTESIAN_POINT('Ctrl Pts',(0.405405868387118,-0.696097894311475,
-1.12625));
#57272=CARTESIAN_POINT('Ctrl Pts',(0.39491538256918,-0.701524073325039,
-1.12625));
#57273=CARTESIAN_POINT('Ctrl Pts',(0.384300816323107,-0.706724162922387,
-1.12625));
#57274=CARTESIAN_POINT('Ctrl Pts',(0.373568843076448,-0.711691937718432,
-1.12625));
#57275=CARTESIAN_POINT('Ctrl Pts',(0.36393057823419,-0.716153440562365,
-1.12625));
#57276=CARTESIAN_POINT('Ctrl Pts',(0.354194037390873,-0.720428823534973,
-1.12625));
#57277=CARTESIAN_POINT('Ctrl Pts',(0.344389136281756,-0.724503440481216,
-1.12625));
#57278=CARTESIAN_POINT('Ctrl Pts',(0.31940466556717,-0.734886222177191,
-1.12625));
#57279=CARTESIAN_POINT('Ctrl Pts',(0.293946819979983,-0.743981294593248,
-1.12625));
#57280=CARTESIAN_POINT('Ctrl Pts',(0.268101859965993,-0.751732914379289,
-1.12625));
#57281=CARTESIAN_POINT('Ctrl Pts',(0.236780787659364,-0.76112697200912,
-1.12625));
#57282=CARTESIAN_POINT('Ctrl Pts',(0.204890853635392,-0.768548833828937,
-1.12625));
#57283=CARTESIAN_POINT('Ctrl Pts',(0.172622384826076,-0.773986220742675,
-1.12625));
#57284=CARTESIAN_POINT('Ctrl Pts',(0.153540924365838,-0.777201535482726,
-1.12625));
#57285=CARTESIAN_POINT('Ctrl Pts',(0.134327020168851,-0.779722340056188,
-1.12625));
#57286=CARTESIAN_POINT('Ctrl Pts',(0.115020357875884,-0.781541004368767,
-1.12625));
#57287=CARTESIAN_POINT('Ctrl Pts',(0.103888024742991,-0.782589656729145,
-1.12625));
#57288=CARTESIAN_POINT('Ctrl Pts',(0.092719076500179,-0.783404877147977,
-1.12625));
#57289=CARTESIAN_POINT('Ctrl Pts',(0.0815541189292635,-0.783983582560274,
-1.12625));
#57290=CARTESIAN_POINT('Ctrl Pts',(0.0448646731874593,-0.785885280859626,
-1.12625));
#57291=CARTESIAN_POINT('Ctrl Pts',(0.00816270548319765,-0.785244764668238,
-1.12625));
#57292=CARTESIAN_POINT('Ctrl Pts',(-0.0282824614477115,-0.782055278068263,
-1.12625));
#57293=CARTESIAN_POINT('Ctrl Pts',(-0.0590932645529008,-0.779358880934872,
-1.12625));
#57294=CARTESIAN_POINT('Ctrl Pts',(-0.0897210642543918,-0.774839835383059,
-1.12625));
#57295=CARTESIAN_POINT('Ctrl Pts',(-0.119998031533351,-0.768465408942047,
-1.12625));
#57296=CARTESIAN_POINT('Ctrl Pts',(-0.136473000057102,-0.764996816001246,
-1.12625));
#57297=CARTESIAN_POINT('Ctrl Pts',(-0.152843949864888,-0.760978380225147,
-1.12625));
#57298=CARTESIAN_POINT('Ctrl Pts',(-0.169085499191347,-0.756419224292614,
-1.12625));
#57299=CARTESIAN_POINT('Ctrl Pts',(-0.177940972571241,-0.753933409473855,
-1.12625));
#57300=CARTESIAN_POINT('Ctrl Pts',(-0.186757956437418,-0.75128681397849,
-1.12625));
#57301=CARTESIAN_POINT('Ctrl Pts',(-0.195532162352344,-0.748480681726736,
-1.12625));
#57302=CARTESIAN_POINT('Ctrl Pts',(-0.202583374982168,-0.746225590455074,
-1.12625));
#57303=CARTESIAN_POINT('Ctrl Pts',(-0.209606136429063,-0.743867596216528,
-1.12625));
#57304=CARTESIAN_POINT('Ctrl Pts',(-0.216586046830733,-0.741412001954268,
-1.12625));
#57305=CARTESIAN_POINT('Ctrl Pts',(-0.250777745036905,-0.729383059876171,
-1.12625));
#57306=CARTESIAN_POINT('Ctrl Pts',(-0.284021591240393,-0.714991447732211,
-1.12625));
#57307=CARTESIAN_POINT('Ctrl Pts',(-0.316082870424553,-0.698370323834583,
-1.12625));
#57308=CARTESIAN_POINT('Ctrl Pts',(-0.347689999411748,-0.681984639285725,
-1.12625));
#57309=CARTESIAN_POINT('Ctrl Pts',(-0.378148790578374,-0.663431461246423,
-1.12625));
#57310=CARTESIAN_POINT('Ctrl Pts',(-0.40720704752179,-0.64279703590621,
-1.12625));
#57311=CARTESIAN_POINT('Ctrl Pts',(-0.425297299274875,-0.629951050343084,
-1.12625));
#57312=CARTESIAN_POINT('Ctrl Pts',(-0.442844152591749,-0.616297659809349,
-1.12625));
#57313=CARTESIAN_POINT('Ctrl Pts',(-0.459778808448986,-0.601851132366388,
-1.12625));
#57314=CARTESIAN_POINT('Ctrl Pts',(-0.459778808448986,-0.601851132366387,
-1.12625));
#57315=CARTESIAN_POINT('Ctrl Pts',(-0.506938887193883,-0.5616200596157,
-1.12625));
#57316=CARTESIAN_POINT('Ctrl Pts',(-0.580457877279435,-0.492400554929899,
-1.12625));
#57317=CARTESIAN_POINT('Ctrl Pts',(-0.691141067841613,-0.302309651856746,
-1.12625));
#57318=CARTESIAN_POINT('Ctrl Pts',(-0.723888788631576,-0.210189415916568,
-1.12625));
#57319=CARTESIAN_POINT('Ctrl Pts',(-0.738728321778979,-0.114178441930225,
-1.12625));
#57320=CARTESIAN_POINT('Origin',(0.,0.,-1.12625));
#57321=CARTESIAN_POINT('Origin',(0.,0.,-1.33003901172249));
#57322=CARTESIAN_POINT('Ctrl Pts',(-0.748490343485036,-0.115687267834994,
-1.1425283350431));
#57323=CARTESIAN_POINT('Ctrl Pts',(-0.729579393836473,-0.238040085590791,
-1.13905034750894));
#57324=CARTESIAN_POINT('Ctrl Pts',(-0.630653629844322,-0.473183377928875,
-1.13209437244062));
#57325=CARTESIAN_POINT('Ctrl Pts',(-0.333406559150436,-0.714445366112156,
-1.12166040983814));
#57326=CARTESIAN_POINT('Ctrl Pts',(0.0423441932323904,-0.787268438306116,
-1.11122644723566));
#57327=CARTESIAN_POINT('Ctrl Pts',(0.40815462829301,-0.674543622261523,
-1.10079248463318));
#57328=CARTESIAN_POINT('Ctrl Pts',(0.677738701453825,-0.402813068451867,
-1.0903585220307));
#57329=CARTESIAN_POINT('Ctrl Pts',(0.787583785039378,-0.0361404951497466,
-1.07992455942822));
#57330=CARTESIAN_POINT('Ctrl Pts',(0.711782686348956,0.339053175380459,
-1.06949059682573));
#57331=CARTESIAN_POINT('Ctrl Pts',(0.468210400798602,0.634327583870298,
-1.05905663422325));
#57332=CARTESIAN_POINT('Ctrl Pts',(0.114275158775044,0.780085648735315,
-1.04862267162077));
#57333=CARTESIAN_POINT('Ctrl Pts',(-0.266595119432196,0.741969872482332,
-1.03818870901829));
#57334=CARTESIAN_POINT('Ctrl Pts',(-0.584626774041369,0.528964985372609,
-1.02775474641581));
#57335=CARTESIAN_POINT('Ctrl Pts',(-0.764856223313064,0.191277995929144,
-1.01732078381333));
#57336=CARTESIAN_POINT('Ctrl Pts',(-0.764801961726998,-0.191494973175325,
-1.00688682121085));
#57337=CARTESIAN_POINT('Ctrl Pts',(-0.584476642087926,-0.529130798350251,
-0.996452858608371));
#57338=CARTESIAN_POINT('Ctrl Pts',(-0.26638470707097,-0.742045509438615,
-0.98601889600589));
#57339=CARTESIAN_POINT('Ctrl Pts',(0.114496619465382,-0.780053123936527,
-0.975584933403409));
#57340=CARTESIAN_POINT('Ctrl Pts',(0.468390010412389,-0.634194881491945,
-0.965150970800929));
#57341=CARTESIAN_POINT('Ctrl Pts',(0.711879475926061,-0.338850945209242,
-0.954717008198449));
#57342=CARTESIAN_POINT('Ctrl Pts',(0.787572255433586,0.0363633449241294,
-0.944283045595967));
#57343=CARTESIAN_POINT('Ctrl Pts',(0.67762685162374,0.403006452460029,-0.933849082993488));
#57344=CARTESIAN_POINT('Ctrl Pts',(0.40795842850662,0.674657150909492,-0.923415120391005));
#57345=CARTESIAN_POINT('Ctrl Pts',(0.0421303690166799,0.78728481673588,
-0.912981157788527));
#57346=CARTESIAN_POINT('Ctrl Pts',(-0.333628214598002,0.714342050500303,
-0.902547195186044));
#57347=CARTESIAN_POINT('Ctrl Pts',(-0.630747491734475,0.473022147824028,
-0.892113232583565));
#57348=CARTESIAN_POINT('Ctrl Pts',(-0.779193655806612,0.120206478312629,
-0.881679269981084));
#57349=CARTESIAN_POINT('Ctrl Pts',(-0.743976550446063,-0.260942988134431,
-0.871245307378603));
#57350=CARTESIAN_POINT('Ctrl Pts',(-0.53339717846247,-0.58058573930206,
-0.860811344776123));
#57351=CARTESIAN_POINT('Ctrl Pts',(-0.197091077355778,-0.763378973969725,
-0.850377382173642));
#57352=CARTESIAN_POINT('Ctrl Pts',(0.1856712434202,-0.766236608391143,-0.839943419571162));
#57353=CARTESIAN_POINT('Ctrl Pts',(0.524669106735824,-0.588485071271487,
-0.829509456968681));
#57354=CARTESIAN_POINT('Ctrl Pts',(0.739997529484913,-0.272022070847804,
-0.8190754943662));
#57355=CARTESIAN_POINT('Ctrl Pts',(0.780901578249223,0.108559088795519,
-0.80864153176372));
#57356=CARTESIAN_POINT('Ctrl Pts',(0.63773978421953,0.463551850709081,-0.798207569161239));
#57357=CARTESIAN_POINT('Ctrl Pts',(0.34425672802939,0.709281083829745,-0.787773606558759));
#57358=CARTESIAN_POINT('Ctrl Pts',(-0.0303708751141361,0.787826097953732,
-0.777339643956278));
#57359=CARTESIAN_POINT('Ctrl Pts',(-0.397839777494351,0.680673094896104,
-0.766905681353797));
#57360=CARTESIAN_POINT('Ctrl Pts',(-0.671534104459314,0.413079044760477,
-0.756471718751318));
#57361=CARTESIAN_POINT('Ctrl Pts',(-0.786941530302541,0.0481183806594918,
-0.746037756148836));
#57362=CARTESIAN_POINT('Ctrl Pts',(-0.716859439874856,-0.328184238095781,
-0.735603793546357));
#57363=CARTESIAN_POINT('Ctrl Pts',(-0.477806840690935,-0.627130746863161,
-0.725169830943874));
#57364=CARTESIAN_POINT('Ctrl Pts',(-0.126130677572574,-0.778256643304304,
-0.714735868341395));
#57365=CARTESIAN_POINT('Ctrl Pts',(0.255275671930622,-0.745940132981574,
-0.704301905738913));
#57366=CARTESIAN_POINT('Ctrl Pts',(0.576511145861981,-0.537798521166715,
-0.693867943136434));
#57367=CARTESIAN_POINT('Ctrl Pts',(0.761857523268443,-0.202892742382452,
-0.683433980533952));
#57368=CARTESIAN_POINT('Ctrl Pts',(0.767626920662054,0.179836763057757,
-0.673000017931472));
#57369=CARTESIAN_POINT('Ctrl Pts',(0.592459436842396,0.520177052904672,
-0.662566055328991));
#57370=CARTESIAN_POINT('Ctrl Pts',(0.277643694393171,0.7379067215007,-0.652132092726511));
#57371=CARTESIAN_POINT('Ctrl Pts',(-0.102615276791054,0.781704839208057,
-0.64169813012403));
#57372=CARTESIAN_POINT('Ctrl Pts',(-0.458686862609225,0.641247777962548,
-0.63126416752155));
#57373=CARTESIAN_POINT('Ctrl Pts',(-0.706641643062582,0.349642587454695,
-0.620830204919068));
#57374=CARTESIAN_POINT('Ctrl Pts',(-0.788034345519909,-0.0243766477023798,
-0.610396242316589));
#57375=CARTESIAN_POINT('Ctrl Pts',(-0.683679944886671,-0.392650077845349,
-0.599962279714108));
#57376=CARTESIAN_POINT('Ctrl Pts',(-0.418175754367006,-0.668372193565669,
-0.589528317111627));
#57377=CARTESIAN_POINT('Ctrl Pts',(-0.0541036075165322,-0.786552700285172,
-0.579094354509147));
#57378=CARTESIAN_POINT('Ctrl Pts',(0.322721268222067,-0.719335341624016,
-0.568660391906666));
#57379=CARTESIAN_POINT('Ctrl Pts',(0.623477707326197,-0.482563880889843,
-0.558226429304186));
#57380=CARTESIAN_POINT('Ctrl Pts',(0.777274589863052,-0.132047577128183,
-0.547792466701705));
#57381=CARTESIAN_POINT('Ctrl Pts',(0.747860544863849,0.249593581864889,
-0.537358504099224));
#57382=CARTESIAN_POINT('Ctrl Pts',(0.542168739239193,0.572403187328638,
-0.526924541496743));
#57383=CARTESIAN_POINT('Ctrl Pts',(0.208682665163577,0.760291980710321,
-0.516490578894263));
#57384=CARTESIAN_POINT('Ctrl Pts',(-0.173991874795186,0.768972807176858,
-0.506056616291782));
#57385=CARTESIAN_POINT('Ctrl Pts',(-0.515654894268529,0.596399514326687,
-0.495622653689302));
#57386=CARTESIAN_POINT('Ctrl Pts',(-0.735773207791702,0.283249249545539,
-0.485188691086821));
#57387=CARTESIAN_POINT('Ctrl Pts',(-0.782462859663332,-0.0966655260145957,
-0.47475472848434));
#57388=CARTESIAN_POINT('Ctrl Pts',(-0.644718660035084,-0.453795328396793,
-0.46432076588186));
#57389=CARTESIAN_POINT('Ctrl Pts',(-0.355008211612248,-0.703961306010574,
-0.453886803279379));
#57390=CARTESIAN_POINT('Ctrl Pts',(0.018381009512838,-0.788196986267641,
-0.443452840676898));
#57391=CARTESIAN_POINT('Ctrl Pts',(0.387437653906621,-0.686647227481264,
-0.433018878074418));
#57392=CARTESIAN_POINT('Ctrl Pts',(0.665171601199015,-0.423248262406717,
-0.422584915471937));
#57393=CARTESIAN_POINT('Ctrl Pts',(0.786118349198422,-0.0600857031737081,
-0.412150952869458));
#57394=CARTESIAN_POINT('Ctrl Pts',(0.721769612451193,0.317239621129983,
-0.401716990266976));
#57395=CARTESIAN_POINT('Ctrl Pts',(0.487292993114226,0.619788584544707,
-0.391283027664496));
#57396=CARTESIAN_POINT('Ctrl Pts',(0.137956834542056,0.776247552318673,
-0.380849065062015));
#57397=CARTESIAN_POINT('Ctrl Pts',(-0.243897046781887,0.749737674945353,
-0.370415102459534));
#57398=CARTESIAN_POINT('Ctrl Pts',(-0.56826210144847,0.546507579770122,
-0.359981139857054));
#57399=CARTESIAN_POINT('Ctrl Pts',(-0.758682436896786,0.214460510585709,
-0.349547177254573));
#57400=CARTESIAN_POINT('Ctrl Pts',(-0.770274190049176,-0.168136916847529,
-0.339113214652093));
#57401=CARTESIAN_POINT('Ctrl Pts',(-0.600305075684723,-0.511102892647924,
-0.328679252049612));
#57402=CARTESIAN_POINT('Ctrl Pts',(-0.288838411909716,-0.733597111627555,
-0.318245289447132));
#57403=CARTESIAN_POINT('Ctrl Pts',(0.0907101808453047,-0.783175596150041,
-0.307811326844651));
#57404=CARTESIAN_POINT('Ctrl Pts',(0.448877531081795,-0.648152228766215,
-0.29737736424217));
#57405=CARTESIAN_POINT('Ctrl Pts',(0.701240227960024,-0.360353291538606,
-0.28694340163969));
#57406=CARTESIAN_POINT('Ctrl Pts',(0.788314010461381,0.0123843106225132,
-0.276509439037209));
#57407=CARTESIAN_POINT('Ctrl Pts',(0.689574771586226,0.382202801273034,
-0.266075476434728));
#57408=CARTESIAN_POINT('Ctrl Pts',(0.428296274062381,0.661932524534914,
-0.255641513832248));
#57409=CARTESIAN_POINT('Ctrl Pts',(0.0660643238823166,0.785638478676652,
-0.245207551229767));
#57410=CARTESIAN_POINT('Ctrl Pts',(-0.311739618905992,0.72416215772478,
-0.234773588627286));
#57411=CARTESIAN_POINT('Ctrl Pts',(-0.616063582497875,0.491993812660686,
-0.224339626024806));
#57412=CARTESIAN_POINT('Ctrl Pts',(-0.775175608854643,0.14385828691005,
-0.213905663422325));
#57413=CARTESIAN_POINT('Ctrl Pts',(-0.751571377703367,-0.238186748774525,
-0.203471700819845));
#57414=CARTESIAN_POINT('Ctrl Pts',(-0.550814864235516,-0.5640874344097,
-0.193037738217364));
#57415=CARTESIAN_POINT('Ctrl Pts',(-0.220225801435357,-0.757030349608771,
-0.182603775614884));
#57416=CARTESIAN_POINT('Ctrl Pts',(0.162271947040142,-0.771528308468151,
-0.172169813012403));
#57417=CARTESIAN_POINT('Ctrl Pts',(0.506521864189483,-0.604181181458603,
-0.161735850409922));
#57418=CARTESIAN_POINT('Ctrl Pts',(0.73137747471038,-0.294400431622848,
-0.151301887807442));
#57419=CARTESIAN_POINT('Ctrl Pts',(0.78384510265579,0.0847288019872882,
-0.140867925204961));
#57420=CARTESIAN_POINT('Ctrl Pts',(0.651544586453749,0.443977659175339,
-0.13043396260248));
#57421=CARTESIAN_POINT('Ctrl Pts',(0.460967102820788,0.613562143858204,
-0.12347798753416));
#57422=CARTESIAN_POINT('Ctrl Pts',(0.351283760559796,0.670985139773185,
-0.12));
#57423=CARTESIAN_POINT('Ctrl Pts',(-0.745983409600528,-0.115299794123053,
-1.14120781194017));
#57424=CARTESIAN_POINT('Ctrl Pts',(-0.727135791628743,-0.237242859367687,
-1.13772982440601));
#57425=CARTESIAN_POINT('Ctrl Pts',(-0.628541377473358,-0.471598508427924,
-1.13077384933769));
#57426=CARTESIAN_POINT('Ctrl Pts',(-0.332289872157592,-0.71205247591253,
-1.12033988673521));
#57427=CARTESIAN_POINT('Ctrl Pts',(0.0422023676688991,-0.78463162043964,
-1.10990592413273));
#57428=CARTESIAN_POINT('Ctrl Pts',(0.406787590016801,-0.672284365610765,
-1.09947196153025));
#57429=CARTESIAN_POINT('Ctrl Pts',(0.67546873968711,-0.401463918278459,
-1.08903799892777));
#57430=CARTESIAN_POINT('Ctrl Pts',(0.784945917892682,-0.03601945007418,
-1.07860403632529));
#57431=CARTESIAN_POINT('Ctrl Pts',(0.709398700781981,0.33791757944523,-1.06817007372281));
#57432=CARTESIAN_POINT('Ctrl Pts',(0.466642216044099,0.632203019823099,
-1.05773611112033));
#57433=CARTESIAN_POINT('Ctrl Pts',(0.113892415079309,0.777472895144442,
-1.04730214851785));
#57434=CARTESIAN_POINT('Ctrl Pts',(-0.265702207996823,0.73948478051424,
-1.03686818591537));
#57435=CARTESIAN_POINT('Ctrl Pts',(-0.582668673968474,0.527193314268243,
-1.02643422331289));
#57436=CARTESIAN_POINT('Ctrl Pts',(-0.762294477768732,0.190637345373097,
-1.01600026071041));
#57437=CARTESIAN_POINT('Ctrl Pts',(-0.76224039792685,-0.190853595901268,
-1.00556629810793));
#57438=CARTESIAN_POINT('Ctrl Pts',(-0.582519044847132,-0.527358571859842,
-0.995132335505446));
#57439=CARTESIAN_POINT('Ctrl Pts',(-0.265492500386352,-0.739560164195111,
-0.984698372902964));
#57440=CARTESIAN_POINT('Ctrl Pts',(0.114113134052997,-0.777440479167041,
-0.974264410300485));
#57441=CARTESIAN_POINT('Ctrl Pts',(0.46682122403901,-0.632070762133708,
-0.963830447698003));
#57442=CARTESIAN_POINT('Ctrl Pts',(0.709495166277286,-0.337716026160002,
-0.953396485095522));
#57443=CARTESIAN_POINT('Ctrl Pts',(0.784934426712148,0.0362415525744356,
-0.942962522493043));
#57444=CARTESIAN_POINT('Ctrl Pts',(0.67535726485342,0.401656656313793,-0.932528559890562));
#57445=CARTESIAN_POINT('Ctrl Pts',(0.406592046625545,0.672397510606688,
-0.922094597288081));
#57446=CARTESIAN_POINT('Ctrl Pts',(0.0419892610781171,0.784647950737613,
-0.911660634685601));
#57447=CARTESIAN_POINT('Ctrl Pts',(-0.332510788126124,0.711949492909918,
-0.90122667208312));
#57448=CARTESIAN_POINT('Ctrl Pts',(-0.628634918776022,0.471437846956661,
-0.890792709480639));
#57449=CARTESIAN_POINT('Ctrl Pts',(-0.776583889666875,0.119803868775785,
-0.88035874687816));
#57450=CARTESIAN_POINT('Ctrl Pts',(-0.741484737537108,-0.260069007488208,
-0.869924784275677));
#57451=CARTESIAN_POINT('Ctrl Pts',(-0.531610662510999,-0.578641173926874,
-0.859490821673199));
#57452=CARTESIAN_POINT('Ctrl Pts',(-0.196430956965558,-0.760822176204229,
-0.849056859070716));
#57453=CARTESIAN_POINT('Ctrl Pts',(0.185049371667793,-0.763670239503633,
-0.838622896468238));
#57454=CARTESIAN_POINT('Ctrl Pts',(0.522911823858683,-0.586514048533684,
-0.828188933865755));
#57455=CARTESIAN_POINT('Ctrl Pts',(0.737519043576373,-0.271110982847447,
-0.817754971263275));
#57456=CARTESIAN_POINT('Ctrl Pts',(0.778286091736729,0.10819549005214,-0.807321008660795));
#57457=CARTESIAN_POINT('Ctrl Pts',(0.63560379186074,0.461999268863761,-0.796887046058314));
#57458=CARTESIAN_POINT('Ctrl Pts',(0.343103703302491,0.706905477018341,
-0.786453083455834));
#57459=CARTESIAN_POINT('Ctrl Pts',(-0.030269153442102,0.785187419033389,
-0.776019120853353));
#57460=CARTESIAN_POINT('Ctrl Pts',(-0.396507286177708,0.678393305293027,
-0.765585158250872));
#57461=CARTESIAN_POINT('Ctrl Pts',(-0.669284924227368,0.411695512315086,
-0.755151195648393));
#57462=CARTESIAN_POINT('Ctrl Pts',(-0.784305814079196,0.0479572169749462,
-0.74471723304591));
#57463=CARTESIAN_POINT('Ctrl Pts',(-0.714458450750783,-0.327085045224027,
-0.734283270443432));
#57464=CARTESIAN_POINT('Ctrl Pts',(-0.476206514372981,-0.625030287527851,
-0.723849307840949));
#57465=CARTESIAN_POINT('Ctrl Pts',(-0.125708226017612,-0.775650015515965,
-0.71341534523847));
#57466=CARTESIAN_POINT('Ctrl Pts',(0.254420672919864,-0.743441743413307,
-0.702981382635988));
#57467=CARTESIAN_POINT('Ctrl Pts',(0.574580227589687,-0.535997263725662,
-0.692547420033508));
#57468=CARTESIAN_POINT('Ctrl Pts',(0.75930582132283,-0.202213190380042,
-0.682113457431027));
#57469=CARTESIAN_POINT('Ctrl Pts',(0.765055895178765,0.179234432826484,
-0.671679494828547));
#57470=CARTESIAN_POINT('Ctrl Pts',(0.590475102696554,0.518434815337383,
-0.661245532226066));
#57471=CARTESIAN_POINT('Ctrl Pts',(0.276713777796521,0.735435238369764,
-0.650811569623585));
#57472=CARTESIAN_POINT('Ctrl Pts',(-0.10227158575508,0.779086662320408,
-0.640377607021105));
#57473=CARTESIAN_POINT('Ctrl Pts',(-0.457150575148642,0.63910003622256,
-0.629943644418625));
#57474=CARTESIAN_POINT('Ctrl Pts',(-0.704274876573596,0.348471523780152,
-0.619509681816143));
#57475=CARTESIAN_POINT('Ctrl Pts',(-0.785394969112563,-0.0242950025949024,
-0.609075719213664));
#57476=CARTESIAN_POINT('Ctrl Pts',(-0.681390084391417,-0.391334968475181,
-0.598641756611182));
#57477=CARTESIAN_POINT('Ctrl Pts',(-0.416775151428219,-0.666133603573935,
-0.588207794008702));
#57478=CARTESIAN_POINT('Ctrl Pts',(-0.0539223974131361,-0.783918286376605,
-0.577773831406221));
#57479=CARTESIAN_POINT('Ctrl Pts',(0.321640372565251,-0.716926059921453,
-0.567339868803741));
#57480=CARTESIAN_POINT('Ctrl Pts',(0.621389483176351,-0.480947621738832,
-0.55690590620126));
#57481=CARTESIAN_POINT('Ctrl Pts',(0.774671251282473,-0.131605308004127,
-0.54647194359878));
#57482=CARTESIAN_POINT('Ctrl Pts',(0.745355723228447,0.248757613971936,
-0.536037980996299));
#57483=CARTESIAN_POINT('Ctrl Pts',(0.5403528445548,0.570486027909492,-0.525604018393818));
#57484=CARTESIAN_POINT('Ctrl Pts',(0.207983720877473,0.757745522262172,
-0.515170055791338));
#57485=CARTESIAN_POINT('Ctrl Pts',(-0.173409120944399,0.766397273893707,
-0.504736093188857));
#57486=CARTESIAN_POINT('Ctrl Pts',(-0.51392780284161,0.594401983614459,
-0.494302130586377));
#57487=CARTESIAN_POINT('Ctrl Pts',(-0.733308870473358,0.282300558170729,
-0.483868167983896));
#57488=CARTESIAN_POINT('Ctrl Pts',(-0.779842143925293,-0.0963417625768507,
-0.473434205381416));
#57489=CARTESIAN_POINT('Ctrl Pts',(-0.642559293212627,-0.452275424232282,
-0.463000242778934));
#57490=CARTESIAN_POINT('Ctrl Pts',(-0.353819176764376,-0.701603516818604,
-0.452566280176454));
#57491=CARTESIAN_POINT('Ctrl Pts',(0.0183194456950587,-0.785557065124961,
-0.442132317573973));
#57492=CARTESIAN_POINT('Ctrl Pts',(0.386140002593766,-0.684347428617565,
-0.431698354971493));
#57493=CARTESIAN_POINT('Ctrl Pts',(0.662943731003988,-0.42183067003324,
-0.421264392369012));
#57494=CARTESIAN_POINT('Ctrl Pts',(0.783485390069101,-0.0598844571388412,
-0.410830429766532));
#57495=CARTESIAN_POINT('Ctrl Pts',(0.719352177605271,0.316177085244022,
-0.400396467164051));
#57496=CARTESIAN_POINT('Ctrl Pts',(0.485660894669784,0.617712716434528,
-0.389962504561571));
#57497=CARTESIAN_POINT('Ctrl Pts',(0.137494773444854,0.773647653611852,
-0.37952854195909));
#57498=CARTESIAN_POINT('Ctrl Pts',(-0.243080158387669,0.747226566207261,
-0.369094579356609));
#57499=CARTESIAN_POINT('Ctrl Pts',(-0.566358811836447,0.544677152935712,
-0.358660616754129));
#57500=CARTESIAN_POINT('Ctrl Pts',(-0.756141369320216,0.213742214466799,
-0.348226654151648));
#57501=CARTESIAN_POINT('Ctrl Pts',(-0.767694298022974,-0.167573773103771,
-0.337792691549167));
#57502=CARTESIAN_POINT('Ctrl Pts',(-0.598294464011481,-0.509391047315011,
-0.327358728946687));
#57503=CARTESIAN_POINT('Ctrl Pts',(-0.287871000661499,-0.731140062743849,
-0.316924766344206));
#57504=CARTESIAN_POINT('Ctrl Pts',(0.0904063637434109,-0.78055249323209,
-0.306490803741726));
#57505=CARTESIAN_POINT('Ctrl Pts',(0.447374098176345,-0.645981361835208,
-0.296056841139245));
#57506=CARTESIAN_POINT('Ctrl Pts',(0.698891552520453,-0.359146354327071,
-0.285622878536764));
#57507=CARTESIAN_POINT('Ctrl Pts',(0.7856736973659,0.0123428316481057,-0.275188915934284));
#57508=CARTESIAN_POINT('Ctrl Pts',(0.687265167454286,0.380922683136222,
-0.264754953331803));
#57509=CARTESIAN_POINT('Ctrl Pts',(0.42686177429361,0.659715503036756,-0.254320990729322));
#57510=CARTESIAN_POINT('Ctrl Pts',(0.0658430535679579,0.783007126777561,
-0.243887028126842));
#57511=CARTESIAN_POINT('Ctrl Pts',(-0.310695504294158,0.721736709503344,
-0.233453065524361));
#57512=CARTESIAN_POINT('Ctrl Pts',(-0.614000190546963,0.490345969652932,
-0.223019102921881));
#57513=CARTESIAN_POINT('Ctrl Pts',(-0.77257930052689,0.1433764600423,-0.2125851403194));
#57514=CARTESIAN_POINT('Ctrl Pts',(-0.749054127115345,-0.237388986095524,
-0.202151177716919));
#57515=CARTESIAN_POINT('Ctrl Pts',(-0.54897001133411,-0.562198126842408,
-0.191717215114439));
#57516=CARTESIAN_POINT('Ctrl Pts',(-0.219488194761937,-0.754494815860373,
-0.181283252511958));
#57517=CARTESIAN_POINT('Ctrl Pts',(0.16172844541913,-0.768944215087348,
-0.170849289909478));
#57518=CARTESIAN_POINT('Ctrl Pts',(0.504825365157446,-0.602157589282072,
-0.160415327306997));
#57519=CARTESIAN_POINT('Ctrl Pts',(0.728927854200651,-0.293414387856205,
-0.149981364704517));
#57520=CARTESIAN_POINT('Ctrl Pts',(0.781219769114279,0.0844450113192236,
-0.139547402102036));
#57521=CARTESIAN_POINT('Ctrl Pts',(0.649362332362849,0.442490652619726,
-0.129113439499555));
#57522=CARTESIAN_POINT('Ctrl Pts',(0.459423217828204,0.611507106016679,
-0.122157464431235));
#57523=CARTESIAN_POINT('Ctrl Pts',(0.350107198737603,0.668737795639035,
-0.118679476897075));
#57524=CARTESIAN_POINT('Ctrl Pts',(-0.74085300492036,-0.114506834660713,
-1.13671995863906));
#57525=CARTESIAN_POINT('Ctrl Pts',(-0.722134886980708,-0.2356120417266,
-1.1332419711049));
#57526=CARTESIAN_POINT('Ctrl Pts',(-0.624218812318242,-0.468354692822244,
-1.12628599603658));
#57527=CARTESIAN_POINT('Ctrl Pts',(-0.330004563367702,-0.707155702503661,
-1.1158520334341));
#57528=CARTESIAN_POINT('Ctrl Pts',(0.0419121041683188,-0.779235354142127,
-1.10541807083161));
#57529=CARTESIAN_POINT('Ctrl Pts',(0.403990000027003,-0.667660918672009,
-1.09498410822914));
#57530=CARTESIAN_POINT('Ctrl Pts',(0.670823328245093,-0.39870289862725,
-1.08455014562665));
#57531=CARTESIAN_POINT('Ctrl Pts',(0.779547608102048,-0.0357717483197839,
-1.07411618302417));
#57532=CARTESIAN_POINT('Ctrl Pts',(0.704519947383167,0.335593624574007,
-1.06368222042169));
#57533=CARTESIAN_POINT('Ctrl Pts',(0.463432975704649,0.627855162501337,
-1.05324825781921));
#57534=CARTESIAN_POINT('Ctrl Pts',(0.113109141693873,0.77212597832659,-1.04281429521673));
#57535=CARTESIAN_POINT('Ctrl Pts',(-0.263874892464704,0.734399116602391,
-1.03238033261425));
#57536=CARTESIAN_POINT('Ctrl Pts',(-0.578661483474969,0.52356764518171,
-1.02194637001177));
#57537=CARTESIAN_POINT('Ctrl Pts',(-0.757051945540771,0.189326273808817,
-1.01151240740929));
#57538=CARTESIAN_POINT('Ctrl Pts',(-0.756998237707175,-0.189541037243187,
-1.00107844480681));
#57539=CARTESIAN_POINT('Ctrl Pts',(-0.578512883273855,-0.523731765804212,
-0.99064448220433));
#57540=CARTESIAN_POINT('Ctrl Pts',(-0.263666627302361,-0.734473982814123,
-0.980210519601848));
#57541=CARTESIAN_POINT('Ctrl Pts',(0.113328343147262,-0.772093783330432,
-0.969776556999368));
#57542=CARTESIAN_POINT('Ctrl Pts',(0.463610751763093,-0.627723818257466,
-0.959342594396887));
#57543=CARTESIAN_POINT('Ctrl Pts',(0.704615751113339,-0.335393449806217,
-0.948908631794406));
#57544=CARTESIAN_POINT('Ctrl Pts',(0.779536192689488,0.0359923083398992,
-0.938474669191926));
#57545=CARTESIAN_POINT('Ctrl Pts',(0.670712626473466,0.398894340692947,
-0.928040706589444));
#57546=CARTESIAN_POINT('Ctrl Pts',(0.403795788817704,0.667773227361877,
-0.917606743986965));
#57547=CARTESIAN_POINT('Ctrl Pts',(0.041700488092816,0.779251686898005,
-0.907172781384485));
#57548=CARTESIAN_POINT('Ctrl Pts',(-0.330224009781218,0.707053198590566,
-0.896738818782003));
#57549=CARTESIAN_POINT('Ctrl Pts',(-0.624311604253704,0.468195624755375,
-0.886304856179523));
#57550=CARTESIAN_POINT('Ctrl Pts',(-0.771243084840893,0.118979940943888,
-0.875870893577043));
#57551=CARTESIAN_POINT('Ctrl Pts',(-0.736385320310805,-0.258280433415595,
-0.865436930974561));
#57552=CARTESIAN_POINT('Ctrl Pts',(-0.527954613461228,-0.574661681671944,
-0.855002968372082));
#57553=CARTESIAN_POINT('Ctrl Pts',(-0.195080041221754,-0.755589769500391,
-0.8445690057696));
#57554=CARTESIAN_POINT('Ctrl Pts',(0.183776730565653,-0.758418245797769,
-0.834135043167121));
#57555=CARTESIAN_POINT('Ctrl Pts',(0.519315599381726,-0.582480412113204,
-0.823701080564639));
#57556=CARTESIAN_POINT('Ctrl Pts',(0.732446899639829,-0.269246469734522,
-0.813267117962159));
#57557=CARTESIAN_POINT('Ctrl Pts',(0.772933580346711,0.107451396589593,
-0.802833155359677));
#57558=CARTESIAN_POINT('Ctrl Pts',(0.631232550267713,0.458821958649652,
-0.792399192757198));
#57559=CARTESIAN_POINT('Ctrl Pts',(0.340744074241427,0.702043871938179,
-0.781965230154717));
#57560=CARTESIAN_POINT('Ctrl Pts',(-0.0300609832200139,0.779787445105682,
-0.771531267552236));
#57561=CARTESIAN_POINT('Ctrl Pts',(-0.393780384350699,0.673727787134543,
-0.761097304949755));
#57562=CARTESIAN_POINT('Ctrl Pts',(-0.664682047190082,0.408864156413596,
-0.750663342347275));
#57563=CARTESIAN_POINT('Ctrl Pts',(-0.778911903218282,0.0476274005323591,
-0.740229379744795));
#57564=CARTESIAN_POINT('Ctrl Pts',(-0.709544901561172,-0.324835581371784,
-0.729795417142313));
#57565=CARTESIAN_POINT('Ctrl Pts',(-0.472931496588076,-0.620731763156647,
-0.719361454539834));
#57566=CARTESIAN_POINT('Ctrl Pts',(-0.124843692115848,-0.770315633228018,
-0.708927491937352));
#57567=CARTESIAN_POINT('Ctrl Pts',(0.252670944170862,-0.7383288672593,-0.698493529334872));
#57568=CARTESIAN_POINT('Ctrl Pts',(0.570628663704239,-0.532311046678268,
-0.688059566732391));
#57569=CARTESIAN_POINT('Ctrl Pts',(0.754083843055084,-0.200822508449306,
-0.67762560412991));
#57570=CARTESIAN_POINT('Ctrl Pts',(0.759794371895204,0.178001782836496,
-0.667191641527431));
#57571=CARTESIAN_POINT('Ctrl Pts',(0.586414224895624,0.514869380616735,
-0.656757678924949));
#57572=CARTESIAN_POINT('Ctrl Pts',(0.274810732549848,0.730377425398687,
-0.64632371632247));
#57573=CARTESIAN_POINT('Ctrl Pts',(-0.101568232793435,0.773728645161736,
-0.635889753719988));
#57574=CARTESIAN_POINT('Ctrl Pts',(-0.454006610883554,0.634704749888187,
-0.625455791117508));
#57575=CARTESIAN_POINT('Ctrl Pts',(-0.699431362936916,0.346074978576616,
-0.615021828515027));
#57576=CARTESIAN_POINT('Ctrl Pts',(-0.779993567799511,-0.0241279184346039,
-0.604587865912547));
#57577=CARTESIAN_POINT('Ctrl Pts',(-0.6767039564669,-0.388643638258292,
-0.594153903310066));
#57578=CARTESIAN_POINT('Ctrl Pts',(-0.413908861295605,-0.661552399132201,
-0.583719940707586));
#57579=CARTESIAN_POINT('Ctrl Pts',(-0.0535515566010041,-0.778527040662178,
-0.573285978105104));
#57580=CARTESIAN_POINT('Ctrl Pts',(0.319428353391424,-0.711995540229179,
-0.562852015502625));
#57581=CARTESIAN_POINT('Ctrl Pts',(0.617115997729737,-0.477639997909124,
-0.552418052900143));
#57582=CARTESIAN_POINT('Ctrl Pts',(0.769343600255385,-0.130700218066689,
-0.541984090297664));
#57583=CARTESIAN_POINT('Ctrl Pts',(0.740229684050112,0.247046831810626,
-0.531550127695182));
#57584=CARTESIAN_POINT('Ctrl Pts',(0.536636672846458,0.566562621086921,
-0.521116165092702));
#57585=CARTESIAN_POINT('Ctrl Pts',(0.206553353244344,0.752534274648081,
-0.510682202490221));
#57586=CARTESIAN_POINT('Ctrl Pts',(-0.172216533405134,0.761126525538638,
-0.500248239887741));
#57587=CARTESIAN_POINT('Ctrl Pts',(-0.510393364223778,0.590314099452934,
-0.48981427728526));
#57588=CARTESIAN_POINT('Ctrl Pts',(-0.728265681184375,0.280359090927436,
-0.479380314682779));
#57589=CARTESIAN_POINT('Ctrl Pts',(-0.77447893108866,-0.0956791908220655,
-0.468946352080299));
#57590=CARTESIAN_POINT('Ctrl Pts',(-0.638140216510372,-0.449164987870472,
-0.458512389477818));
#57591=CARTESIAN_POINT('Ctrl Pts',(-0.351385854116387,-0.696778374939647,
-0.448078426875338));
#57592=CARTESIAN_POINT('Ctrl Pts',(0.0181934572664038,-0.780154549028074,
-0.437644464272857));
#57593=CARTESIAN_POINT('Ctrl Pts',(0.383484399745446,-0.679640962132688,
-0.427210501670377));
#57594=CARTESIAN_POINT('Ctrl Pts',(0.658384464291122,-0.418929611553607,
-0.416776539067895));
#57595=CARTESIAN_POINT('Ctrl Pts',(0.778097121514929,-0.0594726134192606,
-0.406342576465415));
#57596=CARTESIAN_POINT('Ctrl Pts',(0.714404972759966,0.31400263876734,-0.395908613862935));
#57597=CARTESIAN_POINT('Ctrl Pts',(0.482320856221208,0.613464517236846,
-0.385474651260454));
#57598=CARTESIAN_POINT('Ctrl Pts',(0.136549179853022,0.768327042178899,
-0.375040688657973));
#57599=CARTESIAN_POINT('Ctrl Pts',(-0.241408421824054,0.742087660669768,
-0.364606726055493));
#57600=CARTESIAN_POINT('Ctrl Pts',(-0.562463789140712,0.540931241636688,
-0.354172763453012));
#57601=CARTESIAN_POINT('Ctrl Pts',(-0.750941153956067,0.212272243912615,
-0.343738800850532));
#57602=CARTESIAN_POINT('Ctrl Pts',(-0.762414629636954,-0.166421317035277,
-0.333304838248051));
#57603=CARTESIAN_POINT('Ctrl Pts',(-0.594179810071251,-0.505887809352516,
-0.32287087564557));
#57604=CARTESIAN_POINT('Ctrl Pts',(-0.285891223784188,-0.726111789007474,
-0.31243691304309));
#57605=CARTESIAN_POINT('Ctrl Pts',(0.0897846115448724,-0.775184395108459,
-0.302002950440609));
#57606=CARTESIAN_POINT('Ctrl Pts',(0.444297369724572,-0.641538750516211,
-0.291568987838128));
#57607=CARTESIAN_POINT('Ctrl Pts',(0.694085061664188,-0.356676395059477,
-0.281135025235648));
#57608=CARTESIAN_POINT('Ctrl Pts',(0.780270379123696,0.0122579462393565,
-0.270701062633167));
#57609=CARTESIAN_POINT('Ctrl Pts',(0.682538634845942,0.378302961353548,
-0.260267100030687));
#57610=CARTESIAN_POINT('Ctrl Pts',(0.423926115256713,0.655178437904013,
-0.249833137428206));
#57611=CARTESIAN_POINT('Ctrl Pts',(0.065390230985686,0.777622147249572,
-0.239399174825725));
#57612=CARTESIAN_POINT('Ctrl Pts',(-0.308558756771416,0.716773105772149,
-0.228965212223245));
#57613=CARTESIAN_POINT('Ctrl Pts',(-0.609777522647318,0.4869737099821,-0.218531249620764));
#57614=CARTESIAN_POINT('Ctrl Pts',(-0.767266038211424,0.142390417335102,
-0.208097287018283));
#57615=CARTESIAN_POINT('Ctrl Pts',(-0.743902649484962,-0.235756391513143,
-0.197663324415803));
#57616=CARTESIAN_POINT('Ctrl Pts',(-0.545194583421667,-0.558331714416415,
-0.187229361813322));
#57617=CARTESIAN_POINT('Ctrl Pts',(-0.217978694187369,-0.749305932283903,
-0.176795399210842));
#57618=CARTESIAN_POINT('Ctrl Pts',(0.160616163563419,-0.763655935021632,
-0.166361436608361));
#57619=CARTESIAN_POINT('Ctrl Pts',(0.501353577761121,-0.59801639819481,
-0.155927474005881));
#57620=CARTESIAN_POINT('Ctrl Pts',(0.723914693935945,-0.291396426753052,
-0.1454935114034));
#57621=CARTESIAN_POINT('Ctrl Pts',(0.775847282725172,0.0838641360470794,
-0.135059548800919));
#57622=CARTESIAN_POINT('Ctrl Pts',(0.644896041046773,0.439447767297564,
-0.124625586198439));
#57623=CARTESIAN_POINT('Ctrl Pts',(0.456264301675177,0.607301174227483,
-0.117669611130118));
#57624=CARTESIAN_POINT('Ctrl Pts',(0.347699381636247,0.664138637705498,
-0.114191623595958));
#57625=CARTESIAN_POINT('Ctrl Pts',(-0.738728321778979,-0.114178441930225,
-1.13006310830201));
#57626=CARTESIAN_POINT('Ctrl Pts',(-0.720064366806756,-0.234933217536761,
-1.12658512076785));
#57627=CARTESIAN_POINT('Ctrl Pts',(-0.622428042508289,-0.467013310191969,
-1.11962914569953));
#57628=CARTESIAN_POINT('Ctrl Pts',(-0.329058258071172,-0.705126571760283,
-1.10919518309705));
#57629=CARTESIAN_POINT('Ctrl Pts',(0.0417919924060011,-0.777000845426074,
-1.09876122049457));
#57630=CARTESIAN_POINT('Ctrl Pts',(0.402831247473451,-0.665745739445225,
-1.08832725789209));
#57631=CARTESIAN_POINT('Ctrl Pts',(0.668899333621664,-0.397559476691646,
-1.0778932952896));
#57632=CARTESIAN_POINT('Ctrl Pts',(0.777311738081327,-0.0356690904367969,
-1.06745933268712));
#57633=CARTESIAN_POINT('Ctrl Pts',(0.702499287124515,0.334631062607011,
-1.05702537008464));
#57634=CARTESIAN_POINT('Ctrl Pts',(0.462103778469499,0.626054396882009,
-1.04659140748216));
#57635=CARTESIAN_POINT('Ctrl Pts',(0.112784729733045,0.769911399718676,
-1.03615744487968));
#57636=CARTESIAN_POINT('Ctrl Pts',(-0.263118061333196,0.732292755908012,
-1.0257234822772));
#57637=CARTESIAN_POINT('Ctrl Pts',(-0.577001796823254,0.522065974186611,
-1.01528951967472));
#57638=CARTESIAN_POINT('Ctrl Pts',(-0.754880609472422,0.18878325923917,
-1.00485555707224));
#57639=CARTESIAN_POINT('Ctrl Pts',(-0.754827055346663,-0.188997406198552,
-0.994421594469759));
#57640=CARTESIAN_POINT('Ctrl Pts',(-0.57685362332253,-0.522229625831563,
-0.98398763186728));
#57641=CARTESIAN_POINT('Ctrl Pts',(-0.262910392619023,-0.732367403574914,
-0.973553669264798));
#57642=CARTESIAN_POINT('Ctrl Pts',(0.113003300781565,-0.769879304770087,
-0.963119706662318));
#57643=CARTESIAN_POINT('Ctrl Pts',(0.462281047969407,-0.625923414086448,
-0.952685744059838));
#57644=CARTESIAN_POINT('Ctrl Pts',(0.702594809534995,-0.334431492061374,
-0.942251781457356));
#57645=CARTESIAN_POINT('Ctrl Pts',(0.777300368274831,0.035889077098665,
-0.931817818854877));
#57646=CARTESIAN_POINT('Ctrl Pts',(0.668788924044229,0.397750253078557,
-0.921383856252395));
#57647=CARTESIAN_POINT('Ctrl Pts',(0.40263764312539,0.665857955560153,-0.910949893649916));
#57648=CARTESIAN_POINT('Ctrl Pts',(0.0415808849614484,0.777016678487024,
-0.900515931047433));
#57649=CARTESIAN_POINT('Ctrl Pts',(-0.329276878767881,0.705025266057697,
-0.890081968444955));
#57650=CARTESIAN_POINT('Ctrl Pts',(-0.62252098677963,0.466852770864623,
-0.879648005842472));
#57651=CARTESIAN_POINT('Ctrl Pts',(-0.769031046276919,0.118638688979372,
-0.869214043239994));
#57652=CARTESIAN_POINT('Ctrl Pts',(-0.734273258940724,-0.257539647157259,
-0.858780080637511));
#57653=CARTESIAN_POINT('Ctrl Pts',(-0.526440362004134,-0.573013467475886,
-0.848346118035032));
#57654=CARTESIAN_POINT('Ctrl Pts',(-0.194520522980727,-0.753422626946348,
-0.837912155432552));
#57655=CARTESIAN_POINT('Ctrl Pts',(0.183249631881523,-0.756242990757862,
-0.82747819283007));
#57656=CARTESIAN_POINT('Ctrl Pts',(0.517826125887222,-0.5808097726486,-0.81704423022759));
#57657=CARTESIAN_POINT('Ctrl Pts',(0.730346134239288,-0.268474231271757,
-0.806610267625109));
#57658=CARTESIAN_POINT('Ctrl Pts',(0.770716693193102,0.107143210185493,
-0.796176305022629));
#57659=CARTESIAN_POINT('Ctrl Pts',(0.629422082502814,0.457505989811208,
-0.785742342420148));
#57660=CARTESIAN_POINT('Ctrl Pts',(0.33976677013657,0.700030306891271,-0.775308379817668));
#57661=CARTESIAN_POINT('Ctrl Pts',(-0.0299747639002427,0.777550900060216,
-0.764874417215187));
#57662=CARTESIAN_POINT('Ctrl Pts',(-0.392650964310472,0.671795436782193,
-0.754440454612706));
#57663=CARTESIAN_POINT('Ctrl Pts',(-0.662775641349895,0.40769147389731,
-0.744006492010226));
#57664=CARTESIAN_POINT('Ctrl Pts',(-0.776677869355681,0.0474907981449293,
-0.733572529407746));
#57665=CARTESIAN_POINT('Ctrl Pts',(-0.70750982245842,-0.323903905163519,
-0.723138566805264));
#57666=CARTESIAN_POINT('Ctrl Pts',(-0.471575059520285,-0.618951413193122,
-0.712704604202784));
#57667=CARTESIAN_POINT('Ctrl Pts',(-0.124485622050971,-0.768106254731666,
-0.702270641600303));
#57668=CARTESIAN_POINT('Ctrl Pts',(0.251946246752527,-0.736211231510793,
-0.691836678997822));
#57669=CARTESIAN_POINT('Ctrl Pts',(0.56899201679665,-0.530784300330185,
-0.681402716395342));
#57670=CARTESIAN_POINT('Ctrl Pts',(0.751921019719525,-0.200246519967946,
-0.670968753792861));
#57671=CARTESIAN_POINT('Ctrl Pts',(0.757615169923306,0.177491247551546,
-0.66053479119038));
#57672=CARTESIAN_POINT('Ctrl Pts',(0.584732302677573,0.513392659531383,
-0.6501008285879));
#57673=CARTESIAN_POINT('Ctrl Pts',(0.274022534963207,0.728282595554542,
-0.639666865985419));
#57674=CARTESIAN_POINT('Ctrl Pts',(-0.101276920168108,0.771509477645341,
-0.629232903382939));
#57675=CARTESIAN_POINT('Ctrl Pts',(-0.452704453170509,0.632884323344254,
-0.618798940780458));
#57676=CARTESIAN_POINT('Ctrl Pts',(-0.697425290949942,0.345082384654319,
-0.608364978177977));
#57677=CARTESIAN_POINT('Ctrl Pts',(-0.777756431563853,-0.0240587160169824,
-0.597931015575497));
#57678=CARTESIAN_POINT('Ctrl Pts',(-0.674763070023314,-0.387528951161117,
-0.587497052973016));
#57679=CARTESIAN_POINT('Ctrl Pts',(-0.412721709823989,-0.659654969582801,
-0.577063090370536));
#57680=CARTESIAN_POINT('Ctrl Pts',(-0.0533979628629348,-0.776294110641974,
-0.566629127768055));
#57681=CARTESIAN_POINT('Ctrl Pts',(0.318512185908037,-0.709953432334409,
-0.556195165165575));
#57682=CARTESIAN_POINT('Ctrl Pts',(0.615346018313085,-0.476270056167249,
-0.545761202563094));
#57683=CARTESIAN_POINT('Ctrl Pts',(0.767137009692519,-0.130325350624294,
-0.535327239960614));
#57684=CARTESIAN_POINT('Ctrl Pts',(0.738106596479569,0.246338265173458,
-0.524893277358132));
#57685=CARTESIAN_POINT('Ctrl Pts',(0.535097519966525,0.564937636187393,
-0.514459314755653));
#57686=CARTESIAN_POINT('Ctrl Pts',(0.205960927857499,0.750375895702547,
-0.504025352153171));
#57687=CARTESIAN_POINT('Ctrl Pts',(-0.171722591066164,0.758943502754222,
-0.493591389550691));
#57688=CARTESIAN_POINT('Ctrl Pts',(-0.508929481011554,0.58862099182125,
-0.48315742694821));
#57689=CARTESIAN_POINT('Ctrl Pts',(-0.726176908133129,0.279554979833187,
-0.47272346434573));
#57690=CARTESIAN_POINT('Ctrl Pts',(-0.772257611641911,-0.0954047688349832,
-0.462289501743249));
#57691=CARTESIAN_POINT('Ctrl Pts',(-0.636309936543045,-0.447876716644097,
-0.451855539140768));
#57692=CARTESIAN_POINT('Ctrl Pts',(-0.35037802782218,-0.69477991211232,
-0.441421576538288));
#57693=CARTESIAN_POINT('Ctrl Pts',(0.0181412757559645,-0.777916951074585,
-0.430987613935807));
#57694=CARTESIAN_POINT('Ctrl Pts',(0.382384510102889,-0.677691651925019,
-0.420553651333326));
#57695=CARTESIAN_POINT('Ctrl Pts',(0.65649612084464,-0.41772805983205,-0.410119688730846));
#57696=CARTESIAN_POINT('Ctrl Pts',(0.775865424566032,-0.0593020372196476,
-0.399685726128365));
#57697=CARTESIAN_POINT('Ctrl Pts',(0.712355954258471,0.313102033031223,
-0.389251763525885));
#57698=CARTESIAN_POINT('Ctrl Pts',(0.480937489089394,0.61170501080317,-0.378817800923404));
#57699=CARTESIAN_POINT('Ctrl Pts',(0.13615753672838,0.766123367253981,-0.368383838320923));
#57700=CARTESIAN_POINT('Ctrl Pts',(-0.240716026976013,0.739959244149259,
-0.357949875718443));
#57701=CARTESIAN_POINT('Ctrl Pts',(-0.56085056029334,0.539379771301716,
-0.347515913115962));
#57702=CARTESIAN_POINT('Ctrl Pts',(-0.748787344315943,0.2116634159071,-0.337081950513482));
#57703=CARTESIAN_POINT('Ctrl Pts',(-0.760227912378572,-0.165943996230152,
-0.326647987911001));
#57704=CARTESIAN_POINT('Ctrl Pts',(-0.592475615017111,-0.504436848731719,
-0.31621402530852));
#57705=CARTESIAN_POINT('Ctrl Pts',(-0.285071245711685,-0.724029193640402,
-0.30578006270604));
#57706=CARTESIAN_POINT('Ctrl Pts',(0.0895270960624426,-0.772961052277887,
-0.295346100103559));
#57707=CARTESIAN_POINT('Ctrl Pts',(0.443023059573035,-0.639698723071945,
-0.284912137501079));
#57708=CARTESIAN_POINT('Ctrl Pts',(0.692094323595702,-0.355653394680001,
-0.274478174898598));
#57709=CARTESIAN_POINT('Ctrl Pts',(0.778032449069809,0.0122227885764639,
-0.264044212296118));
#57710=CARTESIAN_POINT('Ctrl Pts',(0.680581013455967,0.377217932977417,
-0.253610249693637));
#57711=CARTESIAN_POINT('Ctrl Pts',(0.422710233282295,0.653299289538508,
-0.243176287091156));
#57712=CARTESIAN_POINT('Ctrl Pts',(0.0652026812946528,0.775391813136049,
-0.232742324488676));
#57713=CARTESIAN_POINT('Ctrl Pts',(-0.307673763129744,0.714717294055671,
-0.222308361886195));
#57714=CARTESIAN_POINT('Ctrl Pts',(-0.608028594518636,0.485576999870035,
-0.211874399283715));
#57715=CARTESIAN_POINT('Ctrl Pts',(-0.765065399588575,0.141982016572882,
-0.201440436681234));
#57716=CARTESIAN_POINT('Ctrl Pts',(-0.741769040716875,-0.235080199432132,
-0.191006474078753));
#57717=CARTESIAN_POINT('Ctrl Pts',(-0.543630858812925,-0.556730352880343,
-0.180572511476273));
#57718=CARTESIAN_POINT('Ctrl Pts',(-0.217353551159851,-0.747156781385142,
-0.170138548873792));
#57719=CARTESIAN_POINT('Ctrl Pts',(0.160155594960686,-0.761465719142779,
-0.159704586271311));
#57720=CARTESIAN_POINT('Ctrl Pts',(0.49991542084712,-0.596301077920988,
-0.149270623668831));
#57721=CARTESIAN_POINT('Ctrl Pts',(0.72183879696572,-0.290560898293592,
-0.13883666106635));
#57722=CARTESIAN_POINT('Ctrl Pts',(0.773621246330563,0.0836240792666318,
-0.12840269846387));
#57723=CARTESIAN_POINT('Ctrl Pts',(0.643048073335987,0.438186347774592,
-0.117968735861389));
#57724=CARTESIAN_POINT('Ctrl Pts',(0.454952994195824,0.605560964824554,
-0.111012760793069));
#57725=CARTESIAN_POINT('Ctrl Pts',(0.346702218893402,0.662233962746091,
-0.107534773258908));
#57726=CARTESIAN_POINT('Ctrl Pts',(-0.738728321778979,-0.114178441930225,
-1.12625));
#57727=CARTESIAN_POINT('Ctrl Pts',(-0.720064014057808,-0.234935499803312,
-1.12277201246584));
#57728=CARTESIAN_POINT('Ctrl Pts',(-0.622428467720147,-0.467011987146758,
-1.11581603739752));
#57729=CARTESIAN_POINT('Ctrl Pts',(-0.329058176975973,-0.705127368582215,
-1.10538207479504));
#57730=CARTESIAN_POINT('Ctrl Pts',(0.0417919283474016,-0.77700066177415,
-1.09494811219256));
#57731=CARTESIAN_POINT('Ctrl Pts',(0.402831360764571,-0.66574603450436,
-1.08451414959008));
#57732=CARTESIAN_POINT('Ctrl Pts',(0.66889944257465,-0.397559467050142,
-1.0740801869876));
#57733=CARTESIAN_POINT('Ctrl Pts',(0.77731189566657,-0.0356691406410475,
-1.06364622438512));
#57734=CARTESIAN_POINT('Ctrl Pts',(0.70249941623784,0.334631148448006,-1.05321226178264));
#57735=CARTESIAN_POINT('Ctrl Pts',(0.462103868983754,0.626054505003761,
-1.04277829918016));
#57736=CARTESIAN_POINT('Ctrl Pts',(0.112784749994043,0.769911552166373,
-1.03234433657767));
#57737=CARTESIAN_POINT('Ctrl Pts',(-0.263118110857165,0.732292892594137,
-1.02191037397519));
#57738=CARTESIAN_POINT('Ctrl Pts',(-0.577001907123833,0.522066075167691,
-1.01147641137271));
#57739=CARTESIAN_POINT('Ctrl Pts',(-0.754880753196469,0.188783294475205,
-1.00104244877023));
#57740=CARTESIAN_POINT('Ctrl Pts',(-0.754827199305279,-0.188997441843078,
-0.990608486167753));
#57741=CARTESIAN_POINT('Ctrl Pts',(-0.576853733233579,-0.522229725565813,
-0.980174523565272));
#57742=CARTESIAN_POINT('Ctrl Pts',(-0.262910442753169,-0.732367543071951,
-0.969740560962791));
#57743=CARTESIAN_POINT('Ctrl Pts',(0.113003322331731,-0.769879451565163,
-0.95930659836031));
#57744=CARTESIAN_POINT('Ctrl Pts',(0.462281136078411,-0.625923533367173,
-0.948872635757831));
#57745=CARTESIAN_POINT('Ctrl Pts',(0.70259494345804,-0.334431555819595,
-0.938438673155348));
#57746=CARTESIAN_POINT('Ctrl Pts',(0.777300516433144,0.0358890839459567,
-0.928004710552869));
#57747=CARTESIAN_POINT('Ctrl Pts',(0.668789051521525,0.397750328889645,
-0.917570747950388));
#57748=CARTESIAN_POINT('Ctrl Pts',(0.402637719871012,0.665858082479752,
-0.907136785347908));
#57749=CARTESIAN_POINT('Ctrl Pts',(0.0415808928872875,0.777016826591824,
-0.896702822745427));
#57750=CARTESIAN_POINT('Ctrl Pts',(-0.32927694153081,0.705025400441648,
-0.886268860142946));
#57751=CARTESIAN_POINT('Ctrl Pts',(-0.622521105437113,0.466852859850313,
-0.875834897540466));
#57752=CARTESIAN_POINT('Ctrl Pts',(-0.769031192860477,0.118638711592977,
-0.865400934937984));
#57753=CARTESIAN_POINT('Ctrl Pts',(-0.73427339889913,-0.257539696246454,
-0.854966972335505));
#57754=CARTESIAN_POINT('Ctrl Pts',(-0.526440462347929,-0.573013576696856,
-0.844533009733024));
#57755=CARTESIAN_POINT('Ctrl Pts',(-0.194520560057908,-0.753422770554805,
-0.834099047130543));
#57756=CARTESIAN_POINT('Ctrl Pts',(0.183249666810382,-0.756243134903882,
-0.823665084528063));
#57757=CARTESIAN_POINT('Ctrl Pts',(0.517826224589069,-0.580809883355641,
-0.813231121925582));
#57758=CARTESIAN_POINT('Ctrl Pts',(0.730346273449163,-0.268474282445114,
-0.802797159323102));
#57759=CARTESIAN_POINT('Ctrl Pts',(0.770716840097935,0.107143230607854,
-0.79236319672062));
#57760=CARTESIAN_POINT('Ctrl Pts',(0.62942220247575,0.457506077015547,-0.781929234118141));
#57761=CARTESIAN_POINT('Ctrl Pts',(0.339766834898864,0.700030440322706,
-0.77149527151566));
#57762=CARTESIAN_POINT('Ctrl Pts',(-0.0299747696136753,0.777551048267701,
-0.761061308913179));
#57763=CARTESIAN_POINT('Ctrl Pts',(-0.392651039152919,0.671795564831833,
-0.750627346310698));
#57764=CARTESIAN_POINT('Ctrl Pts',(-0.66277576768029,0.4076915516066,-0.740193383708219));
#57765=CARTESIAN_POINT('Ctrl Pts',(-0.776678017396761,0.0474908071970595,
-0.729759421105736));
#57766=CARTESIAN_POINT('Ctrl Pts',(-0.707509957315512,-0.323903966902222,
-0.719325458503257));
#57767=CARTESIAN_POINT('Ctrl Pts',(-0.471575149406303,-0.618951531170264,
-0.708891495900775));
#57768=CARTESIAN_POINT('Ctrl Pts',(-0.124485645778937,-0.768106401138926,
-0.698457533298296));
#57769=CARTESIAN_POINT('Ctrl Pts',(0.251946294775518,-0.736211371838604,
-0.688023570695814));
#57770=CARTESIAN_POINT('Ctrl Pts',(0.568992125251127,-0.530784401501963,
-0.677589608093334));
#57771=CARTESIAN_POINT('Ctrl Pts',(0.751921163041749,-0.200246558136551,
-0.667155645490854));
#57772=CARTESIAN_POINT('Ctrl Pts',(0.757615314330881,0.177491281382813,
-0.656721682888373));
#57773=CARTESIAN_POINT('Ctrl Pts',(0.584732414132277,0.513392757388173,
-0.646287720285892));
#57774=CARTESIAN_POINT('Ctrl Pts',(0.274022587194117,0.728282734371093,
-0.635853757683412));
#57775=CARTESIAN_POINT('Ctrl Pts',(-0.101276939472307,0.771509624701283,
-0.625419795080931));
#57776=CARTESIAN_POINT('Ctrl Pts',(-0.452704539459636,0.632884443977122,
-0.61498583247845));
#57777=CARTESIAN_POINT('Ctrl Pts',(-0.69742542388484,0.345082450429811,
-0.60455186987597));
#57778=CARTESIAN_POINT('Ctrl Pts',(-0.777756579810515,-0.0240587206027681,
-0.594117907273489));
#57779=CARTESIAN_POINT('Ctrl Pts',(-0.674763198638609,-0.387529025027267,
-0.583683944671009));
#57780=CARTESIAN_POINT('Ctrl Pts',(-0.412721788492083,-0.659655095318369,
-0.573249982068528));
#57781=CARTESIAN_POINT('Ctrl Pts',(-0.0533979730410179,-0.776294258609907,
-0.562816019466048));
#57782=CARTESIAN_POINT('Ctrl Pts',(0.318512246619034,-0.709953567657271,
-0.552382056863567));
#57783=CARTESIAN_POINT('Ctrl Pts',(0.615346135603011,-0.476270146948171,
-0.541948094261087));
#57784=CARTESIAN_POINT('Ctrl Pts',(0.767137155915032,-0.130325375465359,
-0.531514131658606));
#57785=CARTESIAN_POINT('Ctrl Pts',(0.738106737168653,0.246338312127523,
-0.521080169056125));
#57786=CARTESIAN_POINT('Ctrl Pts',(0.535097621960437,0.564937743869073,
-0.510646206453644));
#57787=CARTESIAN_POINT('Ctrl Pts',(0.205960967115317,0.750376038730258,
-0.500212243851164));
#57788=CARTESIAN_POINT('Ctrl Pts',(-0.171722623797879,0.758943647414989,
-0.489778281248683));
#57789=CARTESIAN_POINT('Ctrl Pts',(-0.508929578017626,0.588621104017168,
-0.479344318646203));
#57790=CARTESIAN_POINT('Ctrl Pts',(-0.726177046548319,0.279555033118626,
-0.468910356043722));
#57791=CARTESIAN_POINT('Ctrl Pts',(-0.772257758840452,-0.0954047870199036,
-0.458476393441242));
#57792=CARTESIAN_POINT('Ctrl Pts',(-0.636310057828864,-0.447876802013019,
-0.448042430838761));
#57793=CARTESIAN_POINT('Ctrl Pts',(-0.350378094607062,-0.694780044542988,
-0.43760846823628));
#57794=CARTESIAN_POINT('Ctrl Pts',(0.018141279213836,-0.777917099351843,
-0.4271745056338));
#57795=CARTESIAN_POINT('Ctrl Pts',(0.382384582988471,-0.677691781098527,
-0.416740543031318));
#57796=CARTESIAN_POINT('Ctrl Pts',(0.656496245978099,-0.417728139454391,
-0.406306580428839));
#57797=CARTESIAN_POINT('Ctrl Pts',(0.775865572452268,-0.0593020485231031,
-0.395872617826358));
#57798=CARTESIAN_POINT('Ctrl Pts',(0.712356090039248,0.313102092711016,
-0.385438655223878));
#57799=CARTESIAN_POINT('Ctrl Pts',(0.480937580760017,0.611705127399059,
-0.375004692621396));
#57800=CARTESIAN_POINT('Ctrl Pts',(0.136157562681009,0.766123513283346,
-0.364570730018916));
#57801=CARTESIAN_POINT('Ctrl Pts',(-0.240716072858239,0.739959385191355,
-0.354136767416435));
#57802=CARTESIAN_POINT('Ctrl Pts',(-0.560850667196372,0.539379874112091,
-0.343702804813955));
#57803=CARTESIAN_POINT('Ctrl Pts',(-0.74878748704011,0.211663456251404,
-0.333268842211474));
#57804=CARTESIAN_POINT('Ctrl Pts',(-0.760228057285639,-0.165944027859526,
-0.322834879608993));
#57805=CARTESIAN_POINT('Ctrl Pts',(-0.592475727944838,-0.504436944883217,
-0.312400917006513));
#57806=CARTESIAN_POINT('Ctrl Pts',(-0.285071300054302,-0.724029331642761,
-0.301966954404033));
#57807=CARTESIAN_POINT('Ctrl Pts',(0.0895271131383138,-0.772961199617316,
-0.291532991801552));
#57808=CARTESIAN_POINT('Ctrl Pts',(0.443023143994609,-0.639698844990302,
-0.281099029199071));
#57809=CARTESIAN_POINT('Ctrl Pts',(0.692094455558162,-0.355653462496763,
-0.270665066596591));
#57810=CARTESIAN_POINT('Ctrl Pts',(0.778032597283113,0.0122227909580791,
-0.26023110399411));
#57811=CARTESIAN_POINT('Ctrl Pts',(0.68058114334938,0.377218004776167,-0.249797141391629));
#57812=CARTESIAN_POINT('Ctrl Pts',(0.42271031352139,0.65329941426342,-0.239363178789149));
#57813=CARTESIAN_POINT('Ctrl Pts',(0.0652026943778764,0.775391960536891,
-0.228929216186668));
#57814=CARTESIAN_POINT('Ctrl Pts',(-0.307673823063886,0.714717431064047,
-0.218495253584187));
#57815=CARTESIAN_POINT('Ctrl Pts',(-0.608028707877244,0.485577090895009,
-0.208061290981707));
#57816=CARTESIAN_POINT('Ctrl Pts',(-0.765065550407648,0.141982046646383,
-0.197627328379226));
#57817=CARTESIAN_POINT('Ctrl Pts',(-0.741769172281945,-0.235080250164528,
-0.187193365776746));
#57818=CARTESIAN_POINT('Ctrl Pts',(-0.543630981761295,-0.556730447339991,
-0.176759403174265));
#57819=CARTESIAN_POINT('Ctrl Pts',(-0.217353554555276,-0.747156946739449,
-0.166325440571785));
#57820=CARTESIAN_POINT('Ctrl Pts',(0.160155550638935,-0.76146581913925,
-0.155891477969304));
#57821=CARTESIAN_POINT('Ctrl Pts',(0.499915663487163,-0.596301280456369,
-0.145457515366823));
#57822=CARTESIAN_POINT('Ctrl Pts',(0.721838643854927,-0.290560778341026,
-0.135023552764342));
#57823=CARTESIAN_POINT('Ctrl Pts',(0.7736219742308,0.0836237451066917,-0.124589590161862));
#57824=CARTESIAN_POINT('Ctrl Pts',(0.643046958594169,0.43818717759652,-0.114155627559381));
#57825=CARTESIAN_POINT('Ctrl Pts',(0.454955040136635,0.605559893704287,
-0.107199652491061));
#57826=CARTESIAN_POINT('Ctrl Pts',(0.346702218893402,0.662233962746091,
-0.103721664956901));
#57827=CARTESIAN_POINT('',(0.351283760559806,0.670985139773179,-0.12));
#57828=CARTESIAN_POINT('Ctrl Pts',(0.70874660020474,0.237559480337499,-0.12));
#57829=CARTESIAN_POINT('Ctrl Pts',(0.677871308579866,0.329674339059915,
-0.12));
#57830=CARTESIAN_POINT('Ctrl Pts',(0.630004482514656,0.41492357712479,-0.12));
#57831=CARTESIAN_POINT('Ctrl Pts',(0.488745407170175,0.583538685988193,
-0.12));
#57832=CARTESIAN_POINT('Ctrl Pts',(0.40457236631853,0.63931629107315,-0.12));
#57833=CARTESIAN_POINT('Ctrl Pts',(0.351283760559796,0.670985139773185,
-0.12));
#57834=CARTESIAN_POINT('Ctrl Pts',(-0.459745842892912,-0.601806928197387,
-1.12625));
#57835=CARTESIAN_POINT('Ctrl Pts',(-0.416468302643136,-0.634888226084004,
-1.12472013661271));
#57836=CARTESIAN_POINT('Ctrl Pts',(-0.263250172568355,-0.728042154867829,
-1.11971228569127));
#57837=CARTESIAN_POINT('Ctrl Pts',(0.0423441932323904,-0.787268438306116,
-1.11122644723566));
#57838=CARTESIAN_POINT('Ctrl Pts',(0.40815462829301,-0.674543622261523,
-1.10079248463318));
#57839=CARTESIAN_POINT('Ctrl Pts',(0.677738701453825,-0.402813068451867,
-1.0903585220307));
#57840=CARTESIAN_POINT('Ctrl Pts',(0.787583785039378,-0.0361404951497466,
-1.07992455942822));
#57841=CARTESIAN_POINT('Ctrl Pts',(0.711782686348956,0.339053175380459,
-1.06949059682573));
#57842=CARTESIAN_POINT('Ctrl Pts',(0.468210400798602,0.634327583870298,
-1.05905663422325));
#57843=CARTESIAN_POINT('Ctrl Pts',(0.114275158775044,0.780085648735315,
-1.04862267162077));
#57844=CARTESIAN_POINT('Ctrl Pts',(-0.266595119432196,0.741969872482332,
-1.03818870901829));
#57845=CARTESIAN_POINT('Ctrl Pts',(-0.584626774041369,0.528964985372609,
-1.02775474641581));
#57846=CARTESIAN_POINT('Ctrl Pts',(-0.764856223313064,0.191277995929144,
-1.01732078381333));
#57847=CARTESIAN_POINT('Ctrl Pts',(-0.764801961726998,-0.191494973175325,
-1.00688682121085));
#57848=CARTESIAN_POINT('Ctrl Pts',(-0.584476642087926,-0.529130798350251,
-0.996452858608371));
#57849=CARTESIAN_POINT('Ctrl Pts',(-0.26638470707097,-0.742045509438615,
-0.98601889600589));
#57850=CARTESIAN_POINT('Ctrl Pts',(0.114496619465382,-0.780053123936527,
-0.975584933403409));
#57851=CARTESIAN_POINT('Ctrl Pts',(0.468390010412389,-0.634194881491945,
-0.965150970800929));
#57852=CARTESIAN_POINT('Ctrl Pts',(0.711879475926061,-0.338850945209242,
-0.954717008198449));
#57853=CARTESIAN_POINT('Ctrl Pts',(0.787572255433586,0.0363633449241294,
-0.944283045595967));
#57854=CARTESIAN_POINT('Ctrl Pts',(0.67762685162374,0.403006452460029,-0.933849082993488));
#57855=CARTESIAN_POINT('Ctrl Pts',(0.40795842850662,0.674657150909492,-0.923415120391005));
#57856=CARTESIAN_POINT('Ctrl Pts',(0.0421303690166799,0.78728481673588,
-0.912981157788527));
#57857=CARTESIAN_POINT('Ctrl Pts',(-0.333628214598002,0.714342050500303,
-0.902547195186044));
#57858=CARTESIAN_POINT('Ctrl Pts',(-0.630747491734475,0.473022147824028,
-0.892113232583565));
#57859=CARTESIAN_POINT('Ctrl Pts',(-0.779193655806612,0.120206478312629,
-0.881679269981084));
#57860=CARTESIAN_POINT('Ctrl Pts',(-0.743976550446063,-0.260942988134431,
-0.871245307378603));
#57861=CARTESIAN_POINT('Ctrl Pts',(-0.53339717846247,-0.58058573930206,
-0.860811344776123));
#57862=CARTESIAN_POINT('Ctrl Pts',(-0.197091077355778,-0.763378973969725,
-0.850377382173642));
#57863=CARTESIAN_POINT('Ctrl Pts',(0.1856712434202,-0.766236608391143,-0.839943419571162));
#57864=CARTESIAN_POINT('Ctrl Pts',(0.524669106735824,-0.588485071271487,
-0.829509456968681));
#57865=CARTESIAN_POINT('Ctrl Pts',(0.739997529484913,-0.272022070847804,
-0.8190754943662));
#57866=CARTESIAN_POINT('Ctrl Pts',(0.780901578249223,0.108559088795519,
-0.80864153176372));
#57867=CARTESIAN_POINT('Ctrl Pts',(0.63773978421953,0.463551850709081,-0.798207569161239));
#57868=CARTESIAN_POINT('Ctrl Pts',(0.34425672802939,0.709281083829745,-0.787773606558759));
#57869=CARTESIAN_POINT('Ctrl Pts',(-0.0303708751141361,0.787826097953732,
-0.777339643956278));
#57870=CARTESIAN_POINT('Ctrl Pts',(-0.397839777494351,0.680673094896104,
-0.766905681353797));
#57871=CARTESIAN_POINT('Ctrl Pts',(-0.671534104459314,0.413079044760477,
-0.756471718751318));
#57872=CARTESIAN_POINT('Ctrl Pts',(-0.786941530302541,0.0481183806594918,
-0.746037756148836));
#57873=CARTESIAN_POINT('Ctrl Pts',(-0.716859439874856,-0.328184238095781,
-0.735603793546357));
#57874=CARTESIAN_POINT('Ctrl Pts',(-0.477806840690935,-0.627130746863161,
-0.725169830943874));
#57875=CARTESIAN_POINT('Ctrl Pts',(-0.126130677572574,-0.778256643304304,
-0.714735868341395));
#57876=CARTESIAN_POINT('Ctrl Pts',(0.255275671930622,-0.745940132981574,
-0.704301905738913));
#57877=CARTESIAN_POINT('Ctrl Pts',(0.576511145861981,-0.537798521166715,
-0.693867943136434));
#57878=CARTESIAN_POINT('Ctrl Pts',(0.761857523268443,-0.202892742382452,
-0.683433980533952));
#57879=CARTESIAN_POINT('Ctrl Pts',(0.767626920662054,0.179836763057757,
-0.673000017931472));
#57880=CARTESIAN_POINT('Ctrl Pts',(0.592459436842396,0.520177052904672,
-0.662566055328991));
#57881=CARTESIAN_POINT('Ctrl Pts',(0.277643694393171,0.7379067215007,-0.652132092726511));
#57882=CARTESIAN_POINT('Ctrl Pts',(-0.102615276791054,0.781704839208057,
-0.64169813012403));
#57883=CARTESIAN_POINT('Ctrl Pts',(-0.458686862609225,0.641247777962548,
-0.63126416752155));
#57884=CARTESIAN_POINT('Ctrl Pts',(-0.706641643062582,0.349642587454695,
-0.620830204919068));
#57885=CARTESIAN_POINT('Ctrl Pts',(-0.788034345519909,-0.0243766477023798,
-0.610396242316589));
#57886=CARTESIAN_POINT('Ctrl Pts',(-0.683679944886671,-0.392650077845349,
-0.599962279714108));
#57887=CARTESIAN_POINT('Ctrl Pts',(-0.418175754367006,-0.668372193565669,
-0.589528317111627));
#57888=CARTESIAN_POINT('Ctrl Pts',(-0.0541036075165322,-0.786552700285172,
-0.579094354509147));
#57889=CARTESIAN_POINT('Ctrl Pts',(0.322721268222067,-0.719335341624016,
-0.568660391906666));
#57890=CARTESIAN_POINT('Ctrl Pts',(0.623477707326197,-0.482563880889843,
-0.558226429304186));
#57891=CARTESIAN_POINT('Ctrl Pts',(0.777274589863052,-0.132047577128183,
-0.547792466701705));
#57892=CARTESIAN_POINT('Ctrl Pts',(0.747860544863849,0.249593581864889,
-0.537358504099224));
#57893=CARTESIAN_POINT('Ctrl Pts',(0.542168739239193,0.572403187328638,
-0.526924541496743));
#57894=CARTESIAN_POINT('Ctrl Pts',(0.208682665163577,0.760291980710321,
-0.516490578894263));
#57895=CARTESIAN_POINT('Ctrl Pts',(-0.173991874795186,0.768972807176858,
-0.506056616291782));
#57896=CARTESIAN_POINT('Ctrl Pts',(-0.515654894268529,0.596399514326687,
-0.495622653689302));
#57897=CARTESIAN_POINT('Ctrl Pts',(-0.735773207791702,0.283249249545539,
-0.485188691086821));
#57898=CARTESIAN_POINT('Ctrl Pts',(-0.782462859663332,-0.0966655260145957,
-0.47475472848434));
#57899=CARTESIAN_POINT('Ctrl Pts',(-0.644718660035084,-0.453795328396793,
-0.46432076588186));
#57900=CARTESIAN_POINT('Ctrl Pts',(-0.355008211612248,-0.703961306010574,
-0.453886803279379));
#57901=CARTESIAN_POINT('Ctrl Pts',(0.018381009512838,-0.788196986267641,
-0.443452840676898));
#57902=CARTESIAN_POINT('Ctrl Pts',(0.387437653906621,-0.686647227481264,
-0.433018878074418));
#57903=CARTESIAN_POINT('Ctrl Pts',(0.665171601199015,-0.423248262406717,
-0.422584915471937));
#57904=CARTESIAN_POINT('Ctrl Pts',(0.786118349198422,-0.0600857031737081,
-0.412150952869458));
#57905=CARTESIAN_POINT('Ctrl Pts',(0.721769612451193,0.317239621129983,
-0.401716990266976));
#57906=CARTESIAN_POINT('Ctrl Pts',(0.487292993114226,0.619788584544707,
-0.391283027664496));
#57907=CARTESIAN_POINT('Ctrl Pts',(0.137956834542056,0.776247552318673,
-0.380849065062015));
#57908=CARTESIAN_POINT('Ctrl Pts',(-0.243897046781887,0.749737674945353,
-0.370415102459534));
#57909=CARTESIAN_POINT('Ctrl Pts',(-0.56826210144847,0.546507579770122,
-0.359981139857054));
#57910=CARTESIAN_POINT('Ctrl Pts',(-0.758682436896786,0.214460510585709,
-0.349547177254573));
#57911=CARTESIAN_POINT('Ctrl Pts',(-0.770274190049176,-0.168136916847529,
-0.339113214652093));
#57912=CARTESIAN_POINT('Ctrl Pts',(-0.600305075684723,-0.511102892647924,
-0.328679252049612));
#57913=CARTESIAN_POINT('Ctrl Pts',(-0.288838411909716,-0.733597111627555,
-0.318245289447132));
#57914=CARTESIAN_POINT('Ctrl Pts',(0.0907101808453047,-0.783175596150041,
-0.307811326844651));
#57915=CARTESIAN_POINT('Ctrl Pts',(0.448877531081795,-0.648152228766215,
-0.29737736424217));
#57916=CARTESIAN_POINT('Ctrl Pts',(0.701240227960024,-0.360353291538606,
-0.28694340163969));
#57917=CARTESIAN_POINT('Ctrl Pts',(0.788314010461381,0.0123843106225132,
-0.276509439037209));
#57918=CARTESIAN_POINT('Ctrl Pts',(0.689574771586226,0.382202801273034,
-0.266075476434728));
#57919=CARTESIAN_POINT('Ctrl Pts',(0.428296274062381,0.661932524534914,
-0.255641513832248));
#57920=CARTESIAN_POINT('Ctrl Pts',(0.0660643238823166,0.785638478676652,
-0.245207551229767));
#57921=CARTESIAN_POINT('Ctrl Pts',(-0.311739618905992,0.72416215772478,
-0.234773588627286));
#57922=CARTESIAN_POINT('Ctrl Pts',(-0.616063582497875,0.491993812660686,
-0.224339626024806));
#57923=CARTESIAN_POINT('Ctrl Pts',(-0.775175608854643,0.14385828691005,
-0.213905663422325));
#57924=CARTESIAN_POINT('Ctrl Pts',(-0.751571377703367,-0.238186748774525,
-0.203471700819845));
#57925=CARTESIAN_POINT('Ctrl Pts',(-0.550814864235516,-0.5640874344097,
-0.193037738217364));
#57926=CARTESIAN_POINT('Ctrl Pts',(-0.220225801435357,-0.757030349608771,
-0.182603775614884));
#57927=CARTESIAN_POINT('Ctrl Pts',(0.162271947040142,-0.771528308468151,
-0.172169813012403));
#57928=CARTESIAN_POINT('Ctrl Pts',(0.506521864189483,-0.604181181458603,
-0.161735850409922));
#57929=CARTESIAN_POINT('Ctrl Pts',(0.73137747471038,-0.294400431622848,
-0.151301887807442));
#57930=CARTESIAN_POINT('Ctrl Pts',(0.78384510265579,0.0847288019872882,
-0.140867925204961));
#57931=CARTESIAN_POINT('Ctrl Pts',(0.651544586453749,0.443977659175339,
-0.13043396260248));
#57932=CARTESIAN_POINT('Ctrl Pts',(0.460967102820788,0.613562143858204,
-0.12347798753416));
#57933=CARTESIAN_POINT('Ctrl Pts',(0.351283760559796,0.670985139773185,
-0.12));
#57934=CARTESIAN_POINT('Ctrl Pts',(-0.49595640971927,-0.649207665313752,
-1.15727273924394));
#57935=CARTESIAN_POINT('Ctrl Pts',(-0.388302693694886,-0.73144876218464,
-1.15374460067508));
#57936=CARTESIAN_POINT('Ctrl Pts',(-0.131404556932686,-0.841265750467437,
-1.14668832353737));
#57937=CARTESIAN_POINT('Ctrl Pts',(0.286034174319597,-0.801958781222047,
-1.1361039078308));
#57938=CARTESIAN_POINT('Ctrl Pts',(0.634034477218431,-0.568280999134348,
-1.12551949212423));
#57939=CARTESIAN_POINT('Ctrl Pts',(0.828384689818385,-0.196826841568892,
-1.11493507641766));
#57940=CARTESIAN_POINT('Ctrl Pts',(0.821897829369208,0.222332451391623,
-1.10435066071109));
#57941=CARTESIAN_POINT('Ctrl Pts',(0.616183750099592,0.587599496275829,
-1.09376624500452));
#57942=CARTESIAN_POINT('Ctrl Pts',(0.261091496307321,0.810421806269904,
-1.08318182929794));
#57943=CARTESIAN_POINT('Ctrl Pts',(-0.157289815040408,0.836787381022574,
-1.07259741359137));
#57944=CARTESIAN_POINT('Ctrl Pts',(-0.537543482173718,0.66030313786295,
-1.0620129978848));
#57945=CARTESIAN_POINT('Ctrl Pts',(-0.787488063987499,0.323752245535049,
-1.05142858217823));
#57946=CARTESIAN_POINT('Ctrl Pts',(-0.846534688677586,-0.0912809764781274,
-1.04084416647166));
#57947=CARTESIAN_POINT('Ctrl Pts',(-0.700368959446378,-0.484186307032685,
-1.03025975076509));
#57948=CARTESIAN_POINT('Ctrl Pts',(-0.384423873291054,-0.759717979177559,
-1.01967533505852));
#57949=CARTESIAN_POINT('Ctrl Pts',(0.0247111232736737,-0.851083110906004,
-1.00909091935195));
#57950=CARTESIAN_POINT('Ctrl Pts',(0.427855760691938,-0.736133514901143,
-0.998506503645379));
#57951=CARTESIAN_POINT('Ctrl Pts',(0.727282047487867,-0.442734604895684,
-0.987922087938806));
#57952=CARTESIAN_POINT('Ctrl Pts',(0.850404740342968,-0.0420104871635237,
-0.977337672232236));
#57953=CARTESIAN_POINT('Ctrl Pts',(0.767377146099822,0.368897575755565,
-0.966753256525666));
#57954=CARTESIAN_POINT('Ctrl Pts',(0.498326337204488,0.690379581274125,
-0.956168840819094));
#57955=CARTESIAN_POINT('Ctrl Pts',(0.108474086749782,0.844503687104732,
-0.945584425112523));
#57956=CARTESIAN_POINT('Ctrl Pts',(-0.307673836701549,0.793908001690771,
-0.935000009405954));
#57957=CARTESIAN_POINT('Ctrl Pts',(-0.649237214524838,0.550857644208326,
-0.92441559369938));
#57958=CARTESIAN_POINT('Ctrl Pts',(-0.833416191506256,0.174271502818133,
-0.913831177992813));
#57959=CARTESIAN_POINT('Ctrl Pts',(-0.815563145108209,-0.244560547230943,
-0.90324676228624));
#57960=CARTESIAN_POINT('Ctrl Pts',(-0.600005909618339,-0.604107617370173,
-0.892662346579669));
#57961=CARTESIAN_POINT('Ctrl Pts',(-0.238998646675456,-0.817210347352623,
-0.882077930873099));
#57962=CARTESIAN_POINT('Ctrl Pts',(0.179945311812538,-0.832209582792671,
-0.871493515166528));
#57963=CARTESIAN_POINT('Ctrl Pts',(0.555267949047112,-0.645469294154581,
-0.860909099459957));
#57964=CARTESIAN_POINT('Ctrl Pts',(0.795985681346874,-0.302258002417496,
-0.850324683753386));
#57965=CARTESIAN_POINT('Ctrl Pts',(0.843745082180559,0.114224958881187,
-0.839740268046816));
#57966=CARTESIAN_POINT('Ctrl Pts',(0.686968588642089,0.503018153901045,
-0.829155852340245));
#57967=CARTESIAN_POINT('Ctrl Pts',(0.363661068552688,0.769872542797965,
-0.818571436633674));
#57968=CARTESIAN_POINT('Ctrl Pts',(-0.0478031039138072,0.850098799076459,
-0.807987020927103));
#57969=CARTESIAN_POINT('Ctrl Pts',(-0.447679119223231,0.724248928992339,
-0.797402605220533));
#57970=CARTESIAN_POINT('Ctrl Pts',(-0.739031303134287,0.422830743823914,
-0.786818189513961));
#57971=CARTESIAN_POINT('Ctrl Pts',(-0.851231712714971,0.0189123294010497,
-0.776233773807391));
#57972=CARTESIAN_POINT('Ctrl Pts',(-0.757081361438326,-0.389590704583328,
-0.76564935810082));
#57973=CARTESIAN_POINT('Ctrl Pts',(-0.47940364313556,-0.703651370980966,
-0.755064942394249));
#57974=CARTESIAN_POINT('Ctrl Pts',(-0.0855116143916544,-0.847136865411472,
-0.744480526687677));
#57975=CARTESIAN_POINT('Ctrl Pts',(0.32910965461467,-0.785264248628736,
-0.733896110981108));
#57976=CARTESIAN_POINT('Ctrl Pts',(0.663950028923554,-0.533032329251662,
-0.723311695274536));
#57977=CARTESIAN_POINT('Ctrl Pts',(0.837839405292465,-0.151585737700515,
-0.712727279567966));
#57978=CARTESIAN_POINT('Ctrl Pts',(0.808624507964924,0.266607408099483,
-0.702142863861395));
#57979=CARTESIAN_POINT('Ctrl Pts',(0.583387446549701,0.620171099087391,
-0.691558448154824));
#57980=CARTESIAN_POINT('Ctrl Pts',(0.216728911202076,0.823396431850541,
-0.680974032448253));
#57981=CARTESIAN_POINT('Ctrl Pts',(-0.202467816811901,0.82701867457178,
-0.670389616741682));
#57982=CARTESIAN_POINT('Ctrl Pts',(-0.572583445726546,0.630159743727697,
-0.659805201035112));
#57983=CARTESIAN_POINT('Ctrl Pts',(-0.803896645273109,0.28054106411305,
-0.64922078532854));
#57984=CARTESIAN_POINT('Ctrl Pts',(-0.840333782374011,-0.13708478812774,
-0.63863636962197));
#57985=CARTESIAN_POINT('Ctrl Pts',(-0.67306197304253,-0.521479324018831,
-0.628051953915399));
#57986=CARTESIAN_POINT('Ctrl Pts',(-0.342630299990165,-0.779459801698389,
-0.617467538208829));
#57987=CARTESIAN_POINT('Ctrl Pts',(0.0708598658787425,-0.848488057866866,
-0.606883122502257));
#57988=CARTESIAN_POINT('Ctrl Pts',(0.467172585207633,-0.711830654415401,
-0.596298706795688));
#57989=CARTESIAN_POINT('Ctrl Pts',(0.750235977744157,-0.402615303525972,
-0.585714291089115));
#57990=CARTESIAN_POINT('Ctrl Pts',(0.851431422320549,0.00419976430822538,
-0.575129875382545));
#57991=CARTESIAN_POINT('Ctrl Pts',(0.746227693570421,0.409996749113468,
-0.564545459675974));
#57992=CARTESIAN_POINT('Ctrl Pts',(0.460127682361608,0.71640464882605,-0.553961043969404));
#57993=CARTESIAN_POINT('Ctrl Pts',(0.0624861297268915,0.849145799334127,
-0.543376628262832));
#57994=CARTESIAN_POINT('Ctrl Pts',(-0.350302955852823,0.776041844268604,
-0.532792212556262));
#57995=CARTESIAN_POINT('Ctrl Pts',(-0.678173586925882,0.514814229534424,
-0.522207796849691));
#57996=CARTESIAN_POINT('Ctrl Pts',(-0.841645225850066,0.128788270967645,
-0.51162338114312));
#57997=CARTESIAN_POINT('Ctrl Pts',(-0.801090005657138,-0.288457809343555,
-0.501038965436549));
#57998=CARTESIAN_POINT('Ctrl Pts',(-0.56633909266593,-0.635777584579214,
-0.490454549729979));
#57999=CARTESIAN_POINT('Ctrl Pts',(-0.19429947093741,-0.828975765947642,
-0.479870134023407));
#58000=CARTESIAN_POINT('Ctrl Pts',(0.224841125840782,-0.821218346766365,
-0.469285718316837));
#58001=CARTESIAN_POINT('Ctrl Pts',(0.5894770129187,-0.61438583656814,-0.458701302610266));
#58002=CARTESIAN_POINT('Ctrl Pts',(0.811215227944599,-0.258617398652356,
-0.448116886903695));
#58003=CARTESIAN_POINT('Ctrl Pts',(0.836303251248599,0.159843601330512,
-0.437532471197125));
#58004=CARTESIAN_POINT('Ctrl Pts',(0.65865938660081,0.539556222628661,-0.426948055490553));
#58005=CARTESIAN_POINT('Ctrl Pts',(0.321347051500512,0.788472686544896,
-0.416363639783983));
#58006=CARTESIAN_POINT('Ctrl Pts',(-0.0938644121072754,0.84625207655581,
-0.405779224077412));
#58007=CARTESIAN_POINT('Ctrl Pts',(-0.486321797629799,0.698887840846451,
-0.395194808370841));
#58008=CARTESIAN_POINT('Ctrl Pts',(-0.760887812970074,0.382103181111091,
-0.38461039266427));
#58009=CARTESIAN_POINT('Ctrl Pts',(-0.851003722888248,-0.0273087632644477,
-0.374025976957699));
#58010=CARTESIAN_POINT('Ctrl Pts',(-0.734824139984661,-0.430100672232773,
-0.363441561251129));
#58011=CARTESIAN_POINT('Ctrl Pts',(-0.440512659294734,-0.728630017160838,
-0.352857145544558));
#58012=CARTESIAN_POINT('Ctrl Pts',(-0.0394145998886097,-0.850529008473493,
-0.342272729837987));
#58013=CARTESIAN_POINT('Ctrl Pts',(0.37123812340591,-0.766247584504999,
-0.331688314131417));
#58014=CARTESIAN_POINT('Ctrl Pts',(0.691897407156199,-0.496216769731138,
-0.321103898424845));
#58015=CARTESIAN_POINT('Ctrl Pts',(0.844830849187049,-0.105895901792893,
-0.310519482718275));
#58016=CARTESIAN_POINT('Ctrl Pts',(0.792965189320112,0.310095649688973,
-0.299935067011704));
#58017=CARTESIAN_POINT('Ctrl Pts',(0.5488734125492,0.650915573609111,-0.289350651305133));
#58018=CARTESIAN_POINT('Ctrl Pts',(0.17172685017993,0.833944238330878,-0.278766235598562));
#58019=CARTESIAN_POINT('Ctrl Pts',(-0.247048745074766,0.814812873511378,
-0.268181819891991));
#58020=CARTESIAN_POINT('Ctrl Pts',(-0.605936216145875,0.598159196372129,
-0.257597404185421));
#58021=CARTESIAN_POINT('Ctrl Pts',(-0.81793600853748,0.236503161103032,
-0.24701298847885));
#58022=CARTESIAN_POINT('Ctrl Pts',(-0.831656513568511,-0.182484627408247,
-0.236428572772279));
#58023=CARTESIAN_POINT('Ctrl Pts',(-0.643771334910437,-0.557235529878883,
-0.225844157065708));
#58024=CARTESIAN_POINT('Ctrl Pts',(-0.299827217601208,-0.796904554312887,
-0.215259741359137));
#58025=CARTESIAN_POINT('Ctrl Pts',(0.116800205661499,-0.843392505842621,
-0.204675325652566));
#58026=CARTESIAN_POINT('Ctrl Pts',(0.50511183077168,-0.685430019722108,
-0.194090909945995));
#58027=CARTESIAN_POINT('Ctrl Pts',(0.770980560490101,-0.361309503413311,
-0.183506494239425));
#58028=CARTESIAN_POINT('Ctrl Pts',(0.849945784476039,0.0503976618012852,
-0.172922078532854));
#58029=CARTESIAN_POINT('Ctrl Pts',(0.722885284777076,0.449887613677294,
-0.162337662826283));
#58030=CARTESIAN_POINT('Ctrl Pts',(0.420560857927933,0.74031856457724,-0.151753247119713));
#58031=CARTESIAN_POINT('Ctrl Pts',(0.0163382438423926,0.851285203351961,
-0.141168831413141));
#58032=CARTESIAN_POINT('Ctrl Pts',(-0.391950752487257,0.755890089971345,
-0.130584415706571));
#58033=CARTESIAN_POINT('Ctrl Pts',(-0.600629835243716,0.570122859256891,
-0.123528138568857));
#58034=CARTESIAN_POINT('Ctrl Pts',(-0.676565692095429,0.457932546695683,
-0.12));
#58035=CARTESIAN_POINT('Ctrl Pts',(-0.483897209295843,-0.633422154331296,
-1.14693182616263));
#58036=CARTESIAN_POINT('Ctrl Pts',(-0.378861097787549,-0.713663555562057,
-1.14340368759377));
#58037=CARTESIAN_POINT('Ctrl Pts',(-0.128209449746755,-0.820810339275165,
-1.13634741045605));
#58038=CARTESIAN_POINT('Ctrl Pts',(0.279079241651177,-0.782459120597522,
-1.12576299474949));
#58039=CARTESIAN_POINT('Ctrl Pts',(0.618617902926213,-0.554463223355898,
-1.11517857904291));
#58040=CARTESIAN_POINT('Ctrl Pts',(0.808242482143576,-0.192040988851446,
-1.10459416333634));
#58041=CARTESIAN_POINT('Ctrl Pts',(0.801913349972012,0.216926428726283,
-1.09400974762977));
#58042=CARTESIAN_POINT('Ctrl Pts',(0.601201216968675,0.573311990447837,
-1.0834253319232));
#58043=CARTESIAN_POINT('Ctrl Pts',(0.254743045876759,0.79071636684458,-1.07284091621663));
#58044=CARTESIAN_POINT('Ctrl Pts',(-0.153465306742976,0.816440861566848,
-1.06225650051006));
#58045=CARTESIAN_POINT('Ctrl Pts',(-0.524473090379592,0.644247840010839,
-1.05167208480349));
#58046=CARTESIAN_POINT('Ctrl Pts',(-0.768340259445449,0.31588019641958,
-1.04108766909692));
#58047=CARTESIAN_POINT('Ctrl Pts',(-0.825951163036847,-0.0890614757949546,
-1.03050325339035));
#58048=CARTESIAN_POINT('Ctrl Pts',(-0.683339459500826,-0.472413297138347,
-1.01991883768378));
#58049=CARTESIAN_POINT('Ctrl Pts',(-0.375076591060765,-0.741245405385502,
-1.00933442197721));
#58050=CARTESIAN_POINT('Ctrl Pts',(0.0241102712987718,-0.830388990192416,
-0.998750006270636));
#58051=CARTESIAN_POINT('Ctrl Pts',(0.417452430339938,-0.718234398324307,
-0.988165590564064));
#58052=CARTESIAN_POINT('Ctrl Pts',(0.709598154703862,-0.431969494837231,
-0.977581174857494));
#58053=CARTESIAN_POINT('Ctrl Pts',(0.829727114237415,-0.0409890004468223,
-0.966996759150922));
#58054=CARTESIAN_POINT('Ctrl Pts',(0.748718339350227,0.35992781608602,-0.956412343444353));
#58055=CARTESIAN_POINT('Ctrl Pts',(0.486209511897154,0.673592973468133,
-0.94582792773778));
#58056=CARTESIAN_POINT('Ctrl Pts',(0.105836534885891,0.823969545350454,
-0.935243512031211));
#58057=CARTESIAN_POINT('Ctrl Pts',(-0.300192734755657,0.77460409610042,
-0.924659096324639));
#58058=CARTESIAN_POINT('Ctrl Pts',(-0.633450985052105,0.537463518018798,
-0.914074680618068));
#58059=CARTESIAN_POINT('Ctrl Pts',(-0.813151642661748,0.170034084086585,
-0.903490264911498));
#58060=CARTESIAN_POINT('Ctrl Pts',(-0.795732693818375,-0.238614047504506,
-0.892905849204928));
#58061=CARTESIAN_POINT('Ctrl Pts',(-0.585416741341587,-0.589418715901375,
-0.882321433498355));
#58062=CARTESIAN_POINT('Ctrl Pts',(-0.233187384788915,-0.797339844272722,
-0.871737017791786));
#58063=CARTESIAN_POINT('Ctrl Pts',(0.175569934182816,-0.811974372688474,
-0.861152602085214));
#58064=CARTESIAN_POINT('Ctrl Pts',(0.541766586114726,-0.629774681820034,
-0.850568186378644));
#58065=CARTESIAN_POINT('Ctrl Pts',(0.776631256890553,-0.294908586704127,
-0.839983770672073));
#58066=CARTESIAN_POINT('Ctrl Pts',(0.823229385936095,0.111447574325788,
-0.829399354965502));
#58067=CARTESIAN_POINT('Ctrl Pts',(0.670264919261704,0.490787246878494,
-0.818814939258932));
#58068=CARTESIAN_POINT('Ctrl Pts',(0.354818634770339,0.75115306037541,-0.80823052355236));
#58069=CARTESIAN_POINT('Ctrl Pts',(-0.04664076948348,0.829428611945336,
-0.797646107845791));
#58070=CARTESIAN_POINT('Ctrl Pts',(-0.436793783096309,0.706638786608829,
-0.787061692139218));
#58071=CARTESIAN_POINT('Ctrl Pts',(-0.721061726717831,0.412549596962952,
-0.776477276432649));
#58072=CARTESIAN_POINT('Ctrl Pts',(-0.830533978742308,0.0184524753367573,
-0.765892860726077));
#58073=CARTESIAN_POINT('Ctrl Pts',(-0.73867289711463,-0.380117790638465,
-0.755308445019506));
#58074=CARTESIAN_POINT('Ctrl Pts',(-0.467746923909842,-0.686542059064459,
-0.744724029312936));
#58075=CARTESIAN_POINT('Ctrl Pts',(-0.0834323959840052,-0.826538697818775,
-0.734139613606364));
#58076=CARTESIAN_POINT('Ctrl Pts',(0.321107339877919,-0.766170516248253,
-0.723555197899794));
#58077=CARTESIAN_POINT('Ctrl Pts',(0.647806056765878,-0.520071626325673,
-0.712970782193223));
#58078=CARTESIAN_POINT('Ctrl Pts',(0.817467305823513,-0.147899924277319,
-0.702386366486652));
#58079=CARTESIAN_POINT('Ctrl Pts',(0.788962769921528,0.260124838047689,
-0.691801950780082));
#58080=CARTESIAN_POINT('Ctrl Pts',(0.569202356883381,0.60509161340246,-0.681217535073511));
#58081=CARTESIAN_POINT('Ctrl Pts',(0.211459138846042,0.803375513872609,
-0.67063311936694));
#58082=CARTESIAN_POINT('Ctrl Pts',(-0.197544803550293,0.806909681613663,
-0.660048703660368));
#58083=CARTESIAN_POINT('Ctrl Pts',(-0.55866105578292,0.614837383739067,
-0.649464287953799));
#58084=CARTESIAN_POINT('Ctrl Pts',(-0.784349865404783,0.273719696644373,
-0.638879872247227));
#58085=CARTESIAN_POINT('Ctrl Pts',(-0.819901032024116,-0.133751565887562,
-0.628295456540657));
#58086=CARTESIAN_POINT('Ctrl Pts',(-0.656696443590252,-0.508799532888447,
-0.617711040834086));
#58087=CARTESIAN_POINT('Ctrl Pts',(-0.334299230207119,-0.760507204682846,
-0.607126625127515));
#58088=CARTESIAN_POINT('Ctrl Pts',(0.0691369053365199,-0.827857035974253,
-0.596542209420944));
#58089=CARTESIAN_POINT('Ctrl Pts',(0.455813264656584,-0.694522462887051,
-0.585957793714374));
#58090=CARTESIAN_POINT('Ctrl Pts',(0.731993959205465,-0.392825695924154,
-0.575373378007802));
#58091=CARTESIAN_POINT('Ctrl Pts',(0.830728832400647,0.00409764686699242,
-0.564788962301232));
#58092=CARTESIAN_POINT('Ctrl Pts',(0.728083136625646,0.400027661359745,
-0.554204546594661));
#58093=CARTESIAN_POINT('Ctrl Pts',(0.448939658911915,0.698985240436193,
-0.54362013088809));
#58094=CARTESIAN_POINT('Ctrl Pts',(0.0609667769223016,0.828498784430788,
-0.533035715181519));
#58095=CARTESIAN_POINT('Ctrl Pts',(-0.3417853251281,0.757172355028012,-0.522451299474948));
#58096=CARTESIAN_POINT('Ctrl Pts',(-0.661683768372591,0.50229650044952,
-0.511866883768378));
#58097=CARTESIAN_POINT('Ctrl Pts',(-0.821180587698315,0.125656778882152,
-0.501282468061807));
#58098=CARTESIAN_POINT('Ctrl Pts',(-0.781611469346072,-0.281443945890222,
-0.490698052355236));
#58099=CARTESIAN_POINT('Ctrl Pts',(-0.552568534422826,-0.620318626560096,
-0.480113636648666));
#58100=CARTESIAN_POINT('Ctrl Pts',(-0.189575071340425,-0.808819186232532,
-0.469529220942094));
#58101=CARTESIAN_POINT('Ctrl Pts',(0.219374104653422,-0.801250389016498,
-0.458944805235524));
#58102=CARTESIAN_POINT('Ctrl Pts',(0.575143855196607,-0.599447019778407,
-0.448360389528952));
#58103=CARTESIAN_POINT('Ctrl Pts',(0.791490496438746,-0.252329106007648,
-0.437775973822382));
#58104=CARTESIAN_POINT('Ctrl Pts',(0.815968503428164,0.1559569976148,-0.427191558115811));
#58105=CARTESIAN_POINT('Ctrl Pts',(0.642644056627987,0.526436890967903,
-0.416607142409241));
#58106=CARTESIAN_POINT('Ctrl Pts',(0.313533484776543,0.76930094086502,-0.40602272670267));
#58107=CARTESIAN_POINT('Ctrl Pts',(-0.0915820950809284,0.825675422640391,
-0.395438310996099));
#58108=CARTESIAN_POINT('Ctrl Pts',(-0.474496863194093,0.681894354360343,
-0.384853895289528));
#58109=CARTESIAN_POINT('Ctrl Pts',(-0.742386794621422,0.372812326606244,
-0.374269479582957));
#58110=CARTESIAN_POINT('Ctrl Pts',(-0.830311532497563,-0.0266447495667352,
-0.363685063876386));
#58111=CARTESIAN_POINT('Ctrl Pts',(-0.71695686091257,-0.419642756764676,
-0.353100648169815));
#58112=CARTESIAN_POINT('Ctrl Pts',(-0.429801575934607,-0.710913348439002,
-0.342516232463245));
#58113=CARTESIAN_POINT('Ctrl Pts',(-0.0384562322773608,-0.829848360783256,
-0.331931816756673));
#58114=CARTESIAN_POINT('Ctrl Pts',(0.362211453224346,-0.747616243091864,
-0.321347401050103));
#58115=CARTESIAN_POINT('Ctrl Pts',(0.675073893351694,-0.484151238643356,
-0.310762985343532));
#58116=CARTESIAN_POINT('Ctrl Pts',(0.824288752473333,-0.103321038601866,
-0.300178569636962));
#58117=CARTESIAN_POINT('Ctrl Pts',(0.773684208251183,0.302555661261062,
-0.28959415393039));
#58118=CARTESIAN_POINT('Ctrl Pts',(0.535527533033765,0.635088534766474,
-0.27900973822382));
#58119=CARTESIAN_POINT('Ctrl Pts',(0.167551304781544,0.813666850006195,
-0.268425322517249));
#58120=CARTESIAN_POINT('Ctrl Pts',(-0.241041744715806,0.795000665106161,
-0.257840906810678));
#58121=CARTESIAN_POINT('Ctrl Pts',(-0.591202852222921,0.583614931003625,
-0.247256491104108));
#58122=CARTESIAN_POINT('Ctrl Pts',(-0.798047860976137,0.230752577050434,
-0.236672075397536));
#58123=CARTESIAN_POINT('Ctrl Pts',(-0.811434751365161,-0.17804750621577,
-0.226087659690966));
#58124=CARTESIAN_POINT('Ctrl Pts',(-0.628118008524482,-0.543686325137952,
-0.215503243984395));
#58125=CARTESIAN_POINT('Ctrl Pts',(-0.292536906520245,-0.77752778742275,
-0.204918828277824));
#58126=CARTESIAN_POINT('Ctrl Pts',(0.11396020387512,-0.822885382506259,
-0.194334412571253));
#58127=CARTESIAN_POINT('Ctrl Pts',(0.492830015910234,-0.668763760708055,
-0.183749996864683));
#58128=CARTESIAN_POINT('Ctrl Pts',(0.752234136571964,-0.352524248033677,
-0.173165581158112));
#58129=CARTESIAN_POINT('Ctrl Pts',(0.829279317901194,0.0491722405896154,
-0.162581165451541));
#58130=CARTESIAN_POINT('Ctrl Pts',(0.705308299458534,0.438948577917231,
-0.15199674974497));
#58131=CARTESIAN_POINT('Ctrl Pts',(0.410334903435537,0.722317688346055,
-0.1414123340384));
#58132=CARTESIAN_POINT('Ctrl Pts',(0.0159409787739283,0.830586168752267,
-0.130827918331828));
#58133=CARTESIAN_POINT('Ctrl Pts',(-0.38242045388091,0.737510591462181,
-0.120243502625258));
#58134=CARTESIAN_POINT('Ctrl Pts',(-0.58602549618982,0.556260298574094,
-0.113187225487544));
#58135=CARTESIAN_POINT('Ctrl Pts',(-0.660114969570821,0.446797898059648,
-0.109659086918687));
#58136=CARTESIAN_POINT('Ctrl Pts',(-0.471838008872417,-0.61763664334884,
-1.13659091308131));
#58137=CARTESIAN_POINT('Ctrl Pts',(-0.369419501880212,-0.695878348939475,
-1.13306277451246));
#58138=CARTESIAN_POINT('Ctrl Pts',(-0.125014342560822,-0.800354928082892,
-1.12600649737474));
#58139=CARTESIAN_POINT('Ctrl Pts',(0.272124308982756,-0.762959459972999,
-1.11542208166817));
#58140=CARTESIAN_POINT('Ctrl Pts',(0.603201328633994,-0.540645447577447,
-1.1048376659616));
#58141=CARTESIAN_POINT('Ctrl Pts',(0.788100274468769,-0.187255136134001,
-1.09425325025503));
#58142=CARTESIAN_POINT('Ctrl Pts',(0.781928870574815,0.211520406060943,
-1.08366883454846));
#58143=CARTESIAN_POINT('Ctrl Pts',(0.586218683837759,0.559024484619844,
-1.07308441884189));
#58144=CARTESIAN_POINT('Ctrl Pts',(0.248394595446197,0.771010927419258,
-1.06250000313532));
#58145=CARTESIAN_POINT('Ctrl Pts',(-0.149640798445545,0.796094342111123,
-1.05191558742875));
#58146=CARTESIAN_POINT('Ctrl Pts',(-0.511402698585466,0.628192542158727,
-1.04133117172218));
#58147=CARTESIAN_POINT('Ctrl Pts',(-0.749192454903401,0.308008147304111,
-1.0307467560156));
#58148=CARTESIAN_POINT('Ctrl Pts',(-0.805367637396107,-0.0868419751117828,
-1.02016234030903));
#58149=CARTESIAN_POINT('Ctrl Pts',(-0.666309959555275,-0.460640287244008,
-1.00957792460246));
#58150=CARTESIAN_POINT('Ctrl Pts',(-0.365729308830476,-0.722772831593447,
-0.998993508895893));
#58151=CARTESIAN_POINT('Ctrl Pts',(0.0235094193238699,-0.809694869478828,
-0.988409093189323));
#58152=CARTESIAN_POINT('Ctrl Pts',(0.407049099987939,-0.700335281747471,
-0.977824677482751));
#58153=CARTESIAN_POINT('Ctrl Pts',(0.691914261919856,-0.421204384778777,
-0.96724026177618));
#58154=CARTESIAN_POINT('Ctrl Pts',(0.809049488131863,-0.0399675137301213,
-0.95665584606961));
#58155=CARTESIAN_POINT('Ctrl Pts',(0.730059532600632,0.350958056416475,
-0.94607143036304));
#58156=CARTESIAN_POINT('Ctrl Pts',(0.474092686589821,0.65680636566214,-0.935487014656467));
#58157=CARTESIAN_POINT('Ctrl Pts',(0.103198983021999,0.803435403596176,
-0.924902598949898));
#58158=CARTESIAN_POINT('Ctrl Pts',(-0.292711632809765,0.755300190510067,
-0.914318183243327));
#58159=CARTESIAN_POINT('Ctrl Pts',(-0.61766475557937,0.524069391829271,
-0.903733767536755));
#58160=CARTESIAN_POINT('Ctrl Pts',(-0.792887093817242,0.165796665355037,
-0.893149351830184));
#58161=CARTESIAN_POINT('Ctrl Pts',(-0.775902242528539,-0.232667547778068,
-0.882564936123614));
#58162=CARTESIAN_POINT('Ctrl Pts',(-0.570827573064836,-0.574729814432577,
-0.871980520417042));
#58163=CARTESIAN_POINT('Ctrl Pts',(-0.227376122902374,-0.777469341192823,
-0.861396104710473));
#58164=CARTESIAN_POINT('Ctrl Pts',(0.171194556553094,-0.791739162584277,
-0.850811689003901));
#58165=CARTESIAN_POINT('Ctrl Pts',(0.528265223182337,-0.614080069485487,
-0.840227273297331));
#58166=CARTESIAN_POINT('Ctrl Pts',(0.757276832434234,-0.287559170990757,
-0.829642857590759));
#58167=CARTESIAN_POINT('Ctrl Pts',(0.80271368969163,0.108670189770389,-0.819058441884189));
#58168=CARTESIAN_POINT('Ctrl Pts',(0.65356124988132,0.478556339855944,-0.808474026177618));
#58169=CARTESIAN_POINT('Ctrl Pts',(0.345976200987988,0.732433577952855,
-0.797889610471048));
#58170=CARTESIAN_POINT('Ctrl Pts',(-0.0454784350531522,0.808758424814215,
-0.787305194764476));
#58171=CARTESIAN_POINT('Ctrl Pts',(-0.425908446969388,0.689028644225319,
-0.776720779057906));
#58172=CARTESIAN_POINT('Ctrl Pts',(-0.703092150301373,0.402268450101991,
-0.766136363351335));
#58173=CARTESIAN_POINT('Ctrl Pts',(-0.809836244769647,0.0179926212724646,
-0.755551947644764));
#58174=CARTESIAN_POINT('Ctrl Pts',(-0.720264432790935,-0.370644876693602,
-0.744967531938193));
#58175=CARTESIAN_POINT('Ctrl Pts',(-0.456090204684125,-0.669432747147952,
-0.734383116231623));
#58176=CARTESIAN_POINT('Ctrl Pts',(-0.0813531775763558,-0.805940530226078,
-0.723798700525051));
#58177=CARTESIAN_POINT('Ctrl Pts',(0.313105025141168,-0.747076783867769,
-0.713214284818481));
#58178=CARTESIAN_POINT('Ctrl Pts',(0.631662084608203,-0.507110923399684,
-0.702629869111909));
#58179=CARTESIAN_POINT('Ctrl Pts',(0.797095206354558,-0.144214110854122,
-0.69204545340534));
#58180=CARTESIAN_POINT('Ctrl Pts',(0.769301031878133,0.253642267995895,
-0.681461037698768));
#58181=CARTESIAN_POINT('Ctrl Pts',(0.55501726721706,0.59001212771753,-0.670876621992198));
#58182=CARTESIAN_POINT('Ctrl Pts',(0.206189366490007,0.783354595894676,
-0.660292206285626));
#58183=CARTESIAN_POINT('Ctrl Pts',(-0.192621790288684,0.786800688655547,
-0.649707790579056));
#58184=CARTESIAN_POINT('Ctrl Pts',(-0.544738665839294,0.599515023750437,
-0.639123374872485));
#58185=CARTESIAN_POINT('Ctrl Pts',(-0.764803085536455,0.266898329175697,
-0.628538959165915));
#58186=CARTESIAN_POINT('Ctrl Pts',(-0.799468281674222,-0.130418343647384,
-0.617954543459343));
#58187=CARTESIAN_POINT('Ctrl Pts',(-0.640330914137974,-0.496119741758062,
-0.607370127752773));
#58188=CARTESIAN_POINT('Ctrl Pts',(-0.325968160424073,-0.741554607667304,
-0.596785712046202));
#58189=CARTESIAN_POINT('Ctrl Pts',(0.0674139447942975,-0.807226014081639,
-0.586201296339631));
#58190=CARTESIAN_POINT('Ctrl Pts',(0.444453944105535,-0.677214271358701,
-0.57561688063306));
#58191=CARTESIAN_POINT('Ctrl Pts',(0.713751940666774,-0.383036088322335,
-0.565032464926489));
#58192=CARTESIAN_POINT('Ctrl Pts',(0.810026242480741,0.00399552942575872,
-0.554448049219919));
#58193=CARTESIAN_POINT('Ctrl Pts',(0.709938579680872,0.390058573606024,
-0.543863633513348));
#58194=CARTESIAN_POINT('Ctrl Pts',(0.43775163546222,0.681565832046335,-0.533279217806777));
#58195=CARTESIAN_POINT('Ctrl Pts',(0.0594474241177121,0.807851769527448,
-0.522694802100205));
#58196=CARTESIAN_POINT('Ctrl Pts',(-0.333267694403378,0.73830286578742,
-0.512110386393635));
#58197=CARTESIAN_POINT('Ctrl Pts',(-0.645193949819299,0.489778771364616,
-0.501525970687064));
#58198=CARTESIAN_POINT('Ctrl Pts',(-0.800715949546566,0.122525286796658,
-0.490941554980494));
#58199=CARTESIAN_POINT('Ctrl Pts',(-0.762132933035005,-0.274430082436889,
-0.480357139273922));
#58200=CARTESIAN_POINT('Ctrl Pts',(-0.538797976179722,-0.604859668540979,
-0.469772723567353));
#58201=CARTESIAN_POINT('Ctrl Pts',(-0.184850671743438,-0.788662606517423,
-0.459188307860781));
#58202=CARTESIAN_POINT('Ctrl Pts',(0.21390708346606,-0.78128243126663,-0.44860389215421));
#58203=CARTESIAN_POINT('Ctrl Pts',(0.560810697474516,-0.584508202988675,
-0.438019476447639));
#58204=CARTESIAN_POINT('Ctrl Pts',(0.771765764932894,-0.246040813362938,
-0.427435060741069));
#58205=CARTESIAN_POINT('Ctrl Pts',(0.795633755607728,0.152070393899087,
-0.416850645034498));
#58206=CARTESIAN_POINT('Ctrl Pts',(0.626628726655166,0.513317559307146,
-0.406266229327927));
#58207=CARTESIAN_POINT('Ctrl Pts',(0.305719918052573,0.750129195185145,
-0.395681813621356));
#58208=CARTESIAN_POINT('Ctrl Pts',(-0.0892997780545805,0.805098768724972,
-0.385097397914785));
#58209=CARTESIAN_POINT('Ctrl Pts',(-0.462671928758388,0.664900867874235,
-0.374512982208215));
#58210=CARTESIAN_POINT('Ctrl Pts',(-0.723885776272768,0.363521472101399,
-0.363928566501644));
#58211=CARTESIAN_POINT('Ctrl Pts',(-0.80961934210688,-0.0259807358690237,
-0.353344150795073));
#58212=CARTESIAN_POINT('Ctrl Pts',(-0.699089581840477,-0.409184841296579,
-0.342759735088502));
#58213=CARTESIAN_POINT('Ctrl Pts',(-0.419090492574482,-0.693196679717168,
-0.332175319381931));
#58214=CARTESIAN_POINT('Ctrl Pts',(-0.0374978646661122,-0.809167713093017,
-0.321590903675361));
#58215=CARTESIAN_POINT('Ctrl Pts',(0.353184783042783,-0.72898490167873,
-0.31100648796879));
#58216=CARTESIAN_POINT('Ctrl Pts',(0.658250379547188,-0.472085707555573,
-0.300422072262219));
#58217=CARTESIAN_POINT('Ctrl Pts',(0.803746655759619,-0.100746175410839,
-0.289837656555648));
#58218=CARTESIAN_POINT('Ctrl Pts',(0.754403227182254,0.295015672833151,
-0.279253240849077));
#58219=CARTESIAN_POINT('Ctrl Pts',(0.522181653518331,0.619261495923837,
-0.268668825142507));
#58220=CARTESIAN_POINT('Ctrl Pts',(0.163375759383157,0.793389461681513,
-0.258084409435936));
#58221=CARTESIAN_POINT('Ctrl Pts',(-0.235034744356846,0.775188456700942,
-0.247499993729365));
#58222=CARTESIAN_POINT('Ctrl Pts',(-0.576469488299967,0.569070665635123,
-0.236915578022794));
#58223=CARTESIAN_POINT('Ctrl Pts',(-0.778159713414795,0.225001992997835,
-0.226331162316223));
#58224=CARTESIAN_POINT('Ctrl Pts',(-0.79121298916181,-0.173610385023293,
-0.215746746609652));
#58225=CARTESIAN_POINT('Ctrl Pts',(-0.612464682138529,-0.530137120397022,
-0.205162330903082));
#58226=CARTESIAN_POINT('Ctrl Pts',(-0.285246595439281,-0.758151020532611,
-0.194577915196511));
#58227=CARTESIAN_POINT('Ctrl Pts',(0.11112020208874,-0.802378259169899,
-0.18399349948994));
#58228=CARTESIAN_POINT('Ctrl Pts',(0.480548201048789,-0.652097501693999,
-0.173409083783369));
#58229=CARTESIAN_POINT('Ctrl Pts',(0.733487712653825,-0.343738992654043,
-0.162824668076799));
#58230=CARTESIAN_POINT('Ctrl Pts',(0.808612851326351,0.0479468193779454,
-0.152240252370227));
#58231=CARTESIAN_POINT('Ctrl Pts',(0.687731314139993,0.42800954215717,-0.141655836663657));
#58232=CARTESIAN_POINT('Ctrl Pts',(0.400108948943141,0.704316812114868,
-0.131071420957086));
#58233=CARTESIAN_POINT('Ctrl Pts',(0.0155437137054643,0.809887134152576,
-0.120487005250515));
#58234=CARTESIAN_POINT('Ctrl Pts',(-0.372890155274564,0.719131092953015,
-0.109902589543944));
#58235=CARTESIAN_POINT('Ctrl Pts',(-0.571421157135923,0.542397737891296,
-0.10284631240623));
#58236=CARTESIAN_POINT('Ctrl Pts',(-0.643664247046212,0.435663249423613,
-0.0993181738373734));
#58237=CARTESIAN_POINT('Ctrl Pts',(-0.45977880844899,-0.601851132366384,
-1.12625));
#58238=CARTESIAN_POINT('Ctrl Pts',(-0.359977905972875,-0.678093142316892,
-1.12272186143114));
#58239=CARTESIAN_POINT('Ctrl Pts',(-0.12181923537489,-0.77989951689062,
-1.11566558429343));
#58240=CARTESIAN_POINT('Ctrl Pts',(0.265169376314336,-0.743459799348474,
-1.10508116858686));
#58241=CARTESIAN_POINT('Ctrl Pts',(0.587784754341776,-0.526827671798997,
-1.09449675288029));
#58242=CARTESIAN_POINT('Ctrl Pts',(0.767958066793961,-0.182469283416555,
-1.08391233717372));
#58243=CARTESIAN_POINT('Ctrl Pts',(0.761944391177619,0.206114383395603,
-1.07332792146715));
#58244=CARTESIAN_POINT('Ctrl Pts',(0.571236150706841,0.544736978791852,
-1.06274350576058));
#58245=CARTESIAN_POINT('Ctrl Pts',(0.242046145015635,0.751305487993935,
-1.052159090054));
#58246=CARTESIAN_POINT('Ctrl Pts',(-0.145816290148113,0.775747822655397,
-1.04157467434743));
#58247=CARTESIAN_POINT('Ctrl Pts',(-0.49833230679134,0.612137244306616,
-1.03099025864086));
#58248=CARTESIAN_POINT('Ctrl Pts',(-0.730044650361351,0.300136098188643,
-1.02040584293429));
#58249=CARTESIAN_POINT('Ctrl Pts',(-0.784784111755368,-0.0846224744286107,
-1.00982142722772));
#58250=CARTESIAN_POINT('Ctrl Pts',(-0.649280459609723,-0.44886727734967,
-0.999237011521151));
#58251=CARTESIAN_POINT('Ctrl Pts',(-0.356382026600188,-0.704300257801391,
-0.988652595814579));
#58252=CARTESIAN_POINT('Ctrl Pts',(0.0229085673489686,-0.789000748765239,
-0.978068180108009));
#58253=CARTESIAN_POINT('Ctrl Pts',(0.396645769635938,-0.682436165170636,
-0.967483764401438));
#58254=CARTESIAN_POINT('Ctrl Pts',(0.674230369135851,-0.410439274720323,
-0.956899348694867));
#58255=CARTESIAN_POINT('Ctrl Pts',(0.788371862026309,-0.0389460270134203,
-0.946314932988296));
#58256=CARTESIAN_POINT('Ctrl Pts',(0.711400725851038,0.34198829674693,-0.935730517281726));
#58257=CARTESIAN_POINT('Ctrl Pts',(0.461975861282486,0.640019757856148,
-0.925146101575154));
#58258=CARTESIAN_POINT('Ctrl Pts',(0.100561431158108,0.782901261841898,
-0.914561685868584));
#58259=CARTESIAN_POINT('Ctrl Pts',(-0.285230530863874,0.735996284919716,
-0.903977270162013));
#58260=CARTESIAN_POINT('Ctrl Pts',(-0.601878526106636,0.510675265639743,
-0.893392854455441));
#58261=CARTESIAN_POINT('Ctrl Pts',(-0.772622544972735,0.161559246623488,
-0.882808438748872));
#58262=CARTESIAN_POINT('Ctrl Pts',(-0.756071791238703,-0.226721048051631,
-0.8722240230423));
#58263=CARTESIAN_POINT('Ctrl Pts',(-0.556238404788085,-0.56004091296378,
-0.86163960733573));
#58264=CARTESIAN_POINT('Ctrl Pts',(-0.221564861015834,-0.757598838112922,
-0.851055191629159));
#58265=CARTESIAN_POINT('Ctrl Pts',(0.166819178923372,-0.77150395248008,
-0.840470775922587));
#58266=CARTESIAN_POINT('Ctrl Pts',(0.514763860249949,-0.598385457150939,
-0.829886360216018));
#58267=CARTESIAN_POINT('Ctrl Pts',(0.737922407977915,-0.280209755277388,
-0.819301944509446));
#58268=CARTESIAN_POINT('Ctrl Pts',(0.782197993447165,0.10589280521499,-0.808717528802876));
#58269=CARTESIAN_POINT('Ctrl Pts',(0.636857580500936,0.466325432833393,
-0.798133113096305));
#58270=CARTESIAN_POINT('Ctrl Pts',(0.337133767205639,0.7137140955303,-0.787548697389734));
#58271=CARTESIAN_POINT('Ctrl Pts',(-0.0443161006228249,0.788088237683092,
-0.776964281683163));
#58272=CARTESIAN_POINT('Ctrl Pts',(-0.415023110842465,0.67141850184181,
-0.766379865976593));
#58273=CARTESIAN_POINT('Ctrl Pts',(-0.685122573884916,0.391987303241029,
-0.755795450270022));
#58274=CARTESIAN_POINT('Ctrl Pts',(-0.789138510796985,0.017532767208172,
-0.745211034563451));
#58275=CARTESIAN_POINT('Ctrl Pts',(-0.70185596846724,-0.361171962748739,
-0.73462661885688));
#58276=CARTESIAN_POINT('Ctrl Pts',(-0.444433485458407,-0.652323435231446,
-0.724042203150309));
#58277=CARTESIAN_POINT('Ctrl Pts',(-0.0792739591687064,-0.78534236263338,
-0.713457787443738));
#58278=CARTESIAN_POINT('Ctrl Pts',(0.305102710404417,-0.727983051487286,
-0.702873371737167));
#58279=CARTESIAN_POINT('Ctrl Pts',(0.615518112450528,-0.494150220473694,
-0.692288956030597));
#58280=CARTESIAN_POINT('Ctrl Pts',(0.776723106885605,-0.140528297430926,
-0.681704540324026));
#58281=CARTESIAN_POINT('Ctrl Pts',(0.749639293834737,0.2471596979441,-0.671120124617455));
#58282=CARTESIAN_POINT('Ctrl Pts',(0.540832177550741,0.5749326420326,-0.660535708910885));
#58283=CARTESIAN_POINT('Ctrl Pts',(0.200919594133972,0.763333677916743,
-0.649951293204313));
#58284=CARTESIAN_POINT('Ctrl Pts',(-0.187698777027075,0.76669169569743,
-0.639366877497742));
#58285=CARTESIAN_POINT('Ctrl Pts',(-0.530816275895669,0.584192663761806,
-0.628782461791172));
#58286=CARTESIAN_POINT('Ctrl Pts',(-0.74525630566813,0.26007696170702,-0.618198046084601));
#58287=CARTESIAN_POINT('Ctrl Pts',(-0.779035531324326,-0.127085121407205,
-0.60761363037803));
#58288=CARTESIAN_POINT('Ctrl Pts',(-0.623965384685697,-0.483439950627679,
-0.59702921467146));
#58289=CARTESIAN_POINT('Ctrl Pts',(-0.317637090641027,-0.72260201065176,
-0.586444798964888));
#58290=CARTESIAN_POINT('Ctrl Pts',(0.0656909842520751,-0.786594992189027,
-0.575860383258318));
#58291=CARTESIAN_POINT('Ctrl Pts',(0.433094623554485,-0.65990607983035,
-0.565275967551747));
#58292=CARTESIAN_POINT('Ctrl Pts',(0.695509922128082,-0.373246480720517,
-0.554691551845176));
#58293=CARTESIAN_POINT('Ctrl Pts',(0.789323652560837,0.00389341198452537,
-0.544107136138605));
#58294=CARTESIAN_POINT('Ctrl Pts',(0.691794022736099,0.380089485852302,
-0.533522720432034));
#58295=CARTESIAN_POINT('Ctrl Pts',(0.426563612012526,0.664146423656478,
-0.522938304725464));
#58296=CARTESIAN_POINT('Ctrl Pts',(0.0579280713131231,0.787204754624109,
-0.512353889018892));
#58297=CARTESIAN_POINT('Ctrl Pts',(-0.324750063678657,0.719433376546828,
-0.501769473312322));
#58298=CARTESIAN_POINT('Ctrl Pts',(-0.628704131266007,0.477261042279711,
-0.491185057605751));
#58299=CARTESIAN_POINT('Ctrl Pts',(-0.780251311394817,0.119393794711166,
-0.480600641899181));
#58300=CARTESIAN_POINT('Ctrl Pts',(-0.742654396723938,-0.267416218983557,
-0.470016226192609));
#58301=CARTESIAN_POINT('Ctrl Pts',(-0.525027417936618,-0.589400710521861,
-0.45943181048604));
#58302=CARTESIAN_POINT('Ctrl Pts',(-0.180126272146453,-0.768506026802316,
-0.448847394779467));
#58303=CARTESIAN_POINT('Ctrl Pts',(0.2084400622787,-0.761314473516762,-0.438262979072897));
#58304=CARTESIAN_POINT('Ctrl Pts',(0.546477539752423,-0.569569386198943,
-0.427678563366326));
#58305=CARTESIAN_POINT('Ctrl Pts',(0.752041033427042,-0.239752520718229,
-0.417094147659756));
#58306=CARTESIAN_POINT('Ctrl Pts',(0.775299007787293,0.148183790183373,
-0.406509731953185));
#58307=CARTESIAN_POINT('Ctrl Pts',(0.610613396682344,0.500198227646389,
-0.395925316246614));
#58308=CARTESIAN_POINT('Ctrl Pts',(0.297906351328603,0.730957449505269,
-0.385340900540043));
#58309=CARTESIAN_POINT('Ctrl Pts',(-0.0870174610282331,0.784522114809553,
-0.374756484833472));
#58310=CARTESIAN_POINT('Ctrl Pts',(-0.450846994322682,0.647907381388128,
-0.364172069126901));
#58311=CARTESIAN_POINT('Ctrl Pts',(-0.705384757924115,0.354230617596552,
-0.353587653420331));
#58312=CARTESIAN_POINT('Ctrl Pts',(-0.788927151716196,-0.0253167221713116,
-0.34300323771376));
#58313=CARTESIAN_POINT('Ctrl Pts',(-0.681222302768386,-0.398726925828482,
-0.332418822007189));
#58314=CARTESIAN_POINT('Ctrl Pts',(-0.408379409214356,-0.675480010995333,
-0.321834406300618));
#58315=CARTESIAN_POINT('Ctrl Pts',(-0.0365394970548637,-0.78848706540278,
-0.311249990594048));
#58316=CARTESIAN_POINT('Ctrl Pts',(0.34415811286122,-0.710353560265595,
-0.300665574887476));
#58317=CARTESIAN_POINT('Ctrl Pts',(0.641426865742682,-0.46002017646779,
-0.290081159180906));
#58318=CARTESIAN_POINT('Ctrl Pts',(0.783204559045905,-0.0981713122198112,
-0.279496743474335));
#58319=CARTESIAN_POINT('Ctrl Pts',(0.735122246113324,0.28747568440524,-0.268912327767764));
#58320=CARTESIAN_POINT('Ctrl Pts',(0.508835774002897,0.603434457081201,
-0.258327912061193));
#58321=CARTESIAN_POINT('Ctrl Pts',(0.15920021398477,0.773112073356828,-0.247743496354623));
#58322=CARTESIAN_POINT('Ctrl Pts',(-0.229027743997885,0.755376248295727,
-0.237159080648052));
#58323=CARTESIAN_POINT('Ctrl Pts',(-0.561736124377014,0.554526400266618,
-0.226574664941481));
#58324=CARTESIAN_POINT('Ctrl Pts',(-0.758271565853453,0.219251408945238,
-0.21599024923491));
#58325=CARTESIAN_POINT('Ctrl Pts',(-0.77099122695846,-0.169173263830817,
-0.205405833528339));
#58326=CARTESIAN_POINT('Ctrl Pts',(-0.596811355752575,-0.516587915656091,
-0.194821417821768));
#58327=CARTESIAN_POINT('Ctrl Pts',(-0.277956284358317,-0.738774253642473,
-0.184237002115198));
#58328=CARTESIAN_POINT('Ctrl Pts',(0.10828020030236,-0.781871135833539,
-0.173652586408627));
#58329=CARTESIAN_POINT('Ctrl Pts',(0.468266386187344,-0.635431242679944,
-0.163068170702056));
#58330=CARTESIAN_POINT('Ctrl Pts',(0.714741288735686,-0.33495373727441,
-0.152483754995485));
#58331=CARTESIAN_POINT('Ctrl Pts',(0.787946384751507,0.0467213981662761,
-0.141899339288914));
#58332=CARTESIAN_POINT('Ctrl Pts',(0.670154328821452,0.417070506397107,
-0.131314923582344));
#58333=CARTESIAN_POINT('Ctrl Pts',(0.389882994450745,0.686315935883682,
-0.120730507875773));
#58334=CARTESIAN_POINT('Ctrl Pts',(0.0151464486370003,0.789188099552884,
-0.110146092169202));
#58335=CARTESIAN_POINT('Ctrl Pts',(-0.363359856668217,0.70075159444385,
-0.0995616764626311));
#58336=CARTESIAN_POINT('Ctrl Pts',(-0.556816818082027,0.528535177208499,
-0.0925053993249171));
#58337=CARTESIAN_POINT('Ctrl Pts',(-0.627213524521604,0.424528600787578,
-0.0889772607560602));
#58338=CARTESIAN_POINT('',(-0.676565692095432,0.457932546695678,-0.12));
#58339=CARTESIAN_POINT('Ctrl Pts',(0.351315334519652,0.671030718912572,
-0.12));
#58340=CARTESIAN_POINT('Ctrl Pts',(0.320499669985717,0.689321131271763,
-0.12));
#58341=CARTESIAN_POINT('Ctrl Pts',(0.288470314380493,0.705335580148948,
-0.12));
#58342=CARTESIAN_POINT('Ctrl Pts',(0.255512129576956,0.71904543011569,-0.12));
#58343=CARTESIAN_POINT('Ctrl Pts',(0.222147796814793,0.732924228330349,
-0.12));
#58344=CARTESIAN_POINT('Ctrl Pts',(0.187830516461056,0.744441808855746,
-0.12));
#58345=CARTESIAN_POINT('Ctrl Pts',(0.152824268659072,0.753525280825666,
-0.12));
#58346=CARTESIAN_POINT('Ctrl Pts',(0.126989719984155,0.760228866998956,
-0.12));
#58347=CARTESIAN_POINT('Ctrl Pts',(0.100779187651715,0.765605880524341,
-0.12));
#58348=CARTESIAN_POINT('Ctrl Pts',(0.0742933277386271,0.769609591773371,
-0.12));
#58349=CARTESIAN_POINT('Ctrl Pts',(0.0666757152808372,0.770761101325565,
-0.12));
#58350=CARTESIAN_POINT('Ctrl Pts',(0.05904330606438,0.771797653690265,-0.12));
#58351=CARTESIAN_POINT('Ctrl Pts',(0.0514033585107013,0.772718183814432,
-0.12));
#58352=CARTESIAN_POINT('Ctrl Pts',(0.0392486607748846,0.774182691958939,
-0.12));
#58353=CARTESIAN_POINT('Ctrl Pts',(0.0270711318452966,0.77535414067244,
-0.12));
#58354=CARTESIAN_POINT('Ctrl Pts',(0.0148810082990253,0.776230637396705,
-0.12));
#58355=CARTESIAN_POINT('Ctrl Pts',(-0.0215690645836386,0.77885147789595,
-0.12));
#58356=CARTESIAN_POINT('Ctrl Pts',(-0.0581308241831653,0.778839173851118,
-0.12));
#58357=CARTESIAN_POINT('Ctrl Pts',(-0.0945366085253862,0.77628931721492,
-0.12));
#58358=CARTESIAN_POINT('Ctrl Pts',(-0.121214846926866,0.774420776694254,
-0.12));
#58359=CARTESIAN_POINT('Ctrl Pts',(-0.147809835066177,0.771188449071339,
-0.12));
#58360=CARTESIAN_POINT('Ctrl Pts',(-0.174217694473098,0.766612275855449,
-0.12));
#58361=CARTESIAN_POINT('Ctrl Pts',(-0.190197279887772,0.76384320057188,
-0.12));
#58362=CARTESIAN_POINT('Ctrl Pts',(-0.206108346384988,0.760581783987262,
-0.12));
#58363=CARTESIAN_POINT('Ctrl Pts',(-0.221927418748357,0.75682985953972,
-0.12));
#58364=CARTESIAN_POINT('Ctrl Pts',(-0.229467360157552,0.755041556796273,
-0.12));
#58365=CARTESIAN_POINT('Ctrl Pts',(-0.236985877665914,0.753141777077181,
-0.12));
#58366=CARTESIAN_POINT('Ctrl Pts',(-0.244467321365349,0.751134526253216,
-0.12));
#58367=CARTESIAN_POINT('Ctrl Pts',(-0.28053587885935,0.741457431208775,
-0.12));
#58368=CARTESIAN_POINT('Ctrl Pts',(-0.315822129989096,0.729268499602105,
-0.12));
#58369=CARTESIAN_POINT('Ctrl Pts',(-0.350052129478668,0.714644278113597,
-0.12));
#58370=CARTESIAN_POINT('Ctrl Pts',(-0.355634194410513,0.712259429876851,
-0.12));
#58371=CARTESIAN_POINT('Ctrl Pts',(-0.361188160013049,0.709809706700498,
-0.12));
#58372=CARTESIAN_POINT('Ctrl Pts',(-0.366712818974203,0.707295310693252,
-0.12));
#58373=CARTESIAN_POINT('Ctrl Pts',(-0.397138122868592,0.693448073575234,
-0.12));
#58374=CARTESIAN_POINT('Ctrl Pts',(-0.426675742611679,0.677641907045331,
-0.12));
#58375=CARTESIAN_POINT('Ctrl Pts',(-0.455180005223254,0.660007879054353,
-0.12));
#58376=CARTESIAN_POINT('Ctrl Pts',(-0.46186601449095,0.655871610869445,
-0.12));
#58377=CARTESIAN_POINT('Ctrl Pts',(-0.468495101204548,0.651634643117698,
-0.12));
#58378=CARTESIAN_POINT('Ctrl Pts',(-0.47506524617052,0.647298434033082,
-0.12));
#58379=CARTESIAN_POINT('Ctrl Pts',(-0.481997163210447,0.642723460147725,
-0.12));
#58380=CARTESIAN_POINT('Ctrl Pts',(-0.488856348608865,0.638042668269532,
-0.12));
#58381=CARTESIAN_POINT('Ctrl Pts',(-0.49563768528437,0.633260662340094,
-0.12));
#58382=CARTESIAN_POINT('Ctrl Pts',(-0.526421712148936,0.611552641334433,
-0.12));
#58383=CARTESIAN_POINT('Ctrl Pts',(-0.55562415886581,0.587748863931158,
-0.12));
#58384=CARTESIAN_POINT('Ctrl Pts',(-0.583051806458648,0.562054023958938,
-0.12));
#58385=CARTESIAN_POINT('Ctrl Pts',(-0.610463295427848,0.536374321750432,
-0.12));
#58386=CARTESIAN_POINT('Ctrl Pts',(-0.636103059525297,0.508805062795953,
-0.12));
#58387=CARTESIAN_POINT('Ctrl Pts',(-0.659749387735623,0.479508356571552,
-0.12));
#58388=CARTESIAN_POINT('Ctrl Pts',(-0.665472951291048,0.472417126231326,
-0.12));
#58389=CARTESIAN_POINT('Ctrl Pts',(-0.67107955278444,0.465224522951303,
-0.12));
#58390=CARTESIAN_POINT('Ctrl Pts',(-0.676565692095429,0.457932546695683,
-0.12));
#58391=CARTESIAN_POINT('Ctrl Pts',(0.589349009255739,-0.565869316348666,
-1.12625));
#58392=CARTESIAN_POINT('Ctrl Pts',(0.595826955511013,-0.559130415243387,
-1.12600649737474));
#58393=CARTESIAN_POINT('Ctrl Pts',(0.694346705276111,-0.453008535243734,
-1.12223485618063));
#58394=CARTESIAN_POINT('Ctrl Pts',(0.828384689818385,-0.196826841568892,
-1.11493507641766));
#58395=CARTESIAN_POINT('Ctrl Pts',(0.821897829369208,0.222332451391623,
-1.10435066071109));
#58396=CARTESIAN_POINT('Ctrl Pts',(0.616183750099592,0.587599496275829,
-1.09376624500452));
#58397=CARTESIAN_POINT('Ctrl Pts',(0.261091496307321,0.810421806269904,
-1.08318182929794));
#58398=CARTESIAN_POINT('Ctrl Pts',(-0.157289815040408,0.836787381022574,
-1.07259741359137));
#58399=CARTESIAN_POINT('Ctrl Pts',(-0.537543482173718,0.66030313786295,
-1.0620129978848));
#58400=CARTESIAN_POINT('Ctrl Pts',(-0.787488063987499,0.323752245535049,
-1.05142858217823));
#58401=CARTESIAN_POINT('Ctrl Pts',(-0.846534688677586,-0.0912809764781274,
-1.04084416647166));
#58402=CARTESIAN_POINT('Ctrl Pts',(-0.700368959446378,-0.484186307032685,
-1.03025975076509));
#58403=CARTESIAN_POINT('Ctrl Pts',(-0.384423873291054,-0.759717979177559,
-1.01967533505852));
#58404=CARTESIAN_POINT('Ctrl Pts',(0.0247111232736737,-0.851083110906004,
-1.00909091935195));
#58405=CARTESIAN_POINT('Ctrl Pts',(0.427855760691938,-0.736133514901143,
-0.998506503645379));
#58406=CARTESIAN_POINT('Ctrl Pts',(0.727282047487867,-0.442734604895684,
-0.987922087938806));
#58407=CARTESIAN_POINT('Ctrl Pts',(0.850404740342968,-0.0420104871635237,
-0.977337672232236));
#58408=CARTESIAN_POINT('Ctrl Pts',(0.767377146099822,0.368897575755565,
-0.966753256525666));
#58409=CARTESIAN_POINT('Ctrl Pts',(0.498326337204488,0.690379581274125,
-0.956168840819094));
#58410=CARTESIAN_POINT('Ctrl Pts',(0.108474086749782,0.844503687104732,
-0.945584425112523));
#58411=CARTESIAN_POINT('Ctrl Pts',(-0.307673836701549,0.793908001690771,
-0.935000009405954));
#58412=CARTESIAN_POINT('Ctrl Pts',(-0.649237214524838,0.550857644208326,
-0.92441559369938));
#58413=CARTESIAN_POINT('Ctrl Pts',(-0.833416191506256,0.174271502818133,
-0.913831177992813));
#58414=CARTESIAN_POINT('Ctrl Pts',(-0.815563145108209,-0.244560547230943,
-0.90324676228624));
#58415=CARTESIAN_POINT('Ctrl Pts',(-0.600005909618339,-0.604107617370173,
-0.892662346579669));
#58416=CARTESIAN_POINT('Ctrl Pts',(-0.238998646675456,-0.817210347352623,
-0.882077930873099));
#58417=CARTESIAN_POINT('Ctrl Pts',(0.179945311812538,-0.832209582792671,
-0.871493515166528));
#58418=CARTESIAN_POINT('Ctrl Pts',(0.555267949047112,-0.645469294154581,
-0.860909099459957));
#58419=CARTESIAN_POINT('Ctrl Pts',(0.795985681346874,-0.302258002417496,
-0.850324683753386));
#58420=CARTESIAN_POINT('Ctrl Pts',(0.843745082180559,0.114224958881187,
-0.839740268046816));
#58421=CARTESIAN_POINT('Ctrl Pts',(0.686968588642089,0.503018153901045,
-0.829155852340245));
#58422=CARTESIAN_POINT('Ctrl Pts',(0.363661068552688,0.769872542797965,
-0.818571436633674));
#58423=CARTESIAN_POINT('Ctrl Pts',(-0.0478031039138072,0.850098799076459,
-0.807987020927103));
#58424=CARTESIAN_POINT('Ctrl Pts',(-0.447679119223231,0.724248928992339,
-0.797402605220533));
#58425=CARTESIAN_POINT('Ctrl Pts',(-0.739031303134287,0.422830743823914,
-0.786818189513961));
#58426=CARTESIAN_POINT('Ctrl Pts',(-0.851231712714971,0.0189123294010497,
-0.776233773807391));
#58427=CARTESIAN_POINT('Ctrl Pts',(-0.757081361438326,-0.389590704583328,
-0.76564935810082));
#58428=CARTESIAN_POINT('Ctrl Pts',(-0.47940364313556,-0.703651370980966,
-0.755064942394249));
#58429=CARTESIAN_POINT('Ctrl Pts',(-0.0855116143916544,-0.847136865411472,
-0.744480526687677));
#58430=CARTESIAN_POINT('Ctrl Pts',(0.32910965461467,-0.785264248628736,
-0.733896110981108));
#58431=CARTESIAN_POINT('Ctrl Pts',(0.663950028923554,-0.533032329251662,
-0.723311695274536));
#58432=CARTESIAN_POINT('Ctrl Pts',(0.837839405292465,-0.151585737700515,
-0.712727279567966));
#58433=CARTESIAN_POINT('Ctrl Pts',(0.808624507964924,0.266607408099483,
-0.702142863861395));
#58434=CARTESIAN_POINT('Ctrl Pts',(0.583387446549701,0.620171099087391,
-0.691558448154824));
#58435=CARTESIAN_POINT('Ctrl Pts',(0.216728911202076,0.823396431850541,
-0.680974032448253));
#58436=CARTESIAN_POINT('Ctrl Pts',(-0.202467816811901,0.82701867457178,
-0.670389616741682));
#58437=CARTESIAN_POINT('Ctrl Pts',(-0.572583445726546,0.630159743727697,
-0.659805201035112));
#58438=CARTESIAN_POINT('Ctrl Pts',(-0.803896645273109,0.28054106411305,
-0.64922078532854));
#58439=CARTESIAN_POINT('Ctrl Pts',(-0.840333782374011,-0.13708478812774,
-0.63863636962197));
#58440=CARTESIAN_POINT('Ctrl Pts',(-0.67306197304253,-0.521479324018831,
-0.628051953915399));
#58441=CARTESIAN_POINT('Ctrl Pts',(-0.342630299990165,-0.779459801698389,
-0.617467538208829));
#58442=CARTESIAN_POINT('Ctrl Pts',(0.0708598658787425,-0.848488057866866,
-0.606883122502257));
#58443=CARTESIAN_POINT('Ctrl Pts',(0.467172585207633,-0.711830654415401,
-0.596298706795688));
#58444=CARTESIAN_POINT('Ctrl Pts',(0.750235977744157,-0.402615303525972,
-0.585714291089115));
#58445=CARTESIAN_POINT('Ctrl Pts',(0.851431422320549,0.00419976430822538,
-0.575129875382545));
#58446=CARTESIAN_POINT('Ctrl Pts',(0.746227693570421,0.409996749113468,
-0.564545459675974));
#58447=CARTESIAN_POINT('Ctrl Pts',(0.460127682361608,0.71640464882605,-0.553961043969404));
#58448=CARTESIAN_POINT('Ctrl Pts',(0.0624861297268915,0.849145799334127,
-0.543376628262832));
#58449=CARTESIAN_POINT('Ctrl Pts',(-0.350302955852823,0.776041844268604,
-0.532792212556262));
#58450=CARTESIAN_POINT('Ctrl Pts',(-0.678173586925882,0.514814229534424,
-0.522207796849691));
#58451=CARTESIAN_POINT('Ctrl Pts',(-0.841645225850066,0.128788270967645,
-0.51162338114312));
#58452=CARTESIAN_POINT('Ctrl Pts',(-0.801090005657138,-0.288457809343555,
-0.501038965436549));
#58453=CARTESIAN_POINT('Ctrl Pts',(-0.56633909266593,-0.635777584579214,
-0.490454549729979));
#58454=CARTESIAN_POINT('Ctrl Pts',(-0.19429947093741,-0.828975765947642,
-0.479870134023407));
#58455=CARTESIAN_POINT('Ctrl Pts',(0.224841125840782,-0.821218346766365,
-0.469285718316837));
#58456=CARTESIAN_POINT('Ctrl Pts',(0.5894770129187,-0.61438583656814,-0.458701302610266));
#58457=CARTESIAN_POINT('Ctrl Pts',(0.811215227944599,-0.258617398652356,
-0.448116886903695));
#58458=CARTESIAN_POINT('Ctrl Pts',(0.836303251248599,0.159843601330512,
-0.437532471197125));
#58459=CARTESIAN_POINT('Ctrl Pts',(0.65865938660081,0.539556222628661,-0.426948055490553));
#58460=CARTESIAN_POINT('Ctrl Pts',(0.321347051500512,0.788472686544896,
-0.416363639783983));
#58461=CARTESIAN_POINT('Ctrl Pts',(-0.0938644121072754,0.84625207655581,
-0.405779224077412));
#58462=CARTESIAN_POINT('Ctrl Pts',(-0.486321797629799,0.698887840846451,
-0.395194808370841));
#58463=CARTESIAN_POINT('Ctrl Pts',(-0.760887812970074,0.382103181111091,
-0.38461039266427));
#58464=CARTESIAN_POINT('Ctrl Pts',(-0.851003722888248,-0.0273087632644477,
-0.374025976957699));
#58465=CARTESIAN_POINT('Ctrl Pts',(-0.734824139984661,-0.430100672232773,
-0.363441561251129));
#58466=CARTESIAN_POINT('Ctrl Pts',(-0.440512659294734,-0.728630017160838,
-0.352857145544558));
#58467=CARTESIAN_POINT('Ctrl Pts',(-0.0394145998886097,-0.850529008473493,
-0.342272729837987));
#58468=CARTESIAN_POINT('Ctrl Pts',(0.37123812340591,-0.766247584504999,
-0.331688314131417));
#58469=CARTESIAN_POINT('Ctrl Pts',(0.691897407156199,-0.496216769731138,
-0.321103898424845));
#58470=CARTESIAN_POINT('Ctrl Pts',(0.844830849187049,-0.105895901792893,
-0.310519482718275));
#58471=CARTESIAN_POINT('Ctrl Pts',(0.792965189320112,0.310095649688973,
-0.299935067011704));
#58472=CARTESIAN_POINT('Ctrl Pts',(0.5488734125492,0.650915573609111,-0.289350651305133));
#58473=CARTESIAN_POINT('Ctrl Pts',(0.17172685017993,0.833944238330878,-0.278766235598562));
#58474=CARTESIAN_POINT('Ctrl Pts',(-0.247048745074766,0.814812873511378,
-0.268181819891991));
#58475=CARTESIAN_POINT('Ctrl Pts',(-0.605936216145875,0.598159196372129,
-0.257597404185421));
#58476=CARTESIAN_POINT('Ctrl Pts',(-0.81793600853748,0.236503161103032,
-0.24701298847885));
#58477=CARTESIAN_POINT('Ctrl Pts',(-0.831656513568511,-0.182484627408247,
-0.236428572772279));
#58478=CARTESIAN_POINT('Ctrl Pts',(-0.643771334910437,-0.557235529878883,
-0.225844157065708));
#58479=CARTESIAN_POINT('Ctrl Pts',(-0.299827217601208,-0.796904554312887,
-0.215259741359137));
#58480=CARTESIAN_POINT('Ctrl Pts',(0.116800205661499,-0.843392505842621,
-0.204675325652566));
#58481=CARTESIAN_POINT('Ctrl Pts',(0.50511183077168,-0.685430019722108,
-0.194090909945995));
#58482=CARTESIAN_POINT('Ctrl Pts',(0.770980560490101,-0.361309503413311,
-0.183506494239425));
#58483=CARTESIAN_POINT('Ctrl Pts',(0.849945784476039,0.0503976618012852,
-0.172922078532854));
#58484=CARTESIAN_POINT('Ctrl Pts',(0.722885284777076,0.449887613677294,
-0.162337662826283));
#58485=CARTESIAN_POINT('Ctrl Pts',(0.420560857927933,0.74031856457724,-0.151753247119713));
#58486=CARTESIAN_POINT('Ctrl Pts',(0.0163382438423926,0.851285203351961,
-0.141168831413141));
#58487=CARTESIAN_POINT('Ctrl Pts',(-0.391950752487257,0.755890089971345,
-0.130584415706571));
#58488=CARTESIAN_POINT('Ctrl Pts',(-0.600629835243716,0.570122859256891,
-0.123528138568857));
#58489=CARTESIAN_POINT('Ctrl Pts',(-0.676565692095429,0.457932546695683,
-0.12));
#58490=CARTESIAN_POINT('Ctrl Pts',(0.589301091561365,-0.565833523687263,
-1.12625));
#58491=CARTESIAN_POINT('Ctrl Pts',(0.681795706363583,-0.469502756447991,
-1.12277201246584));
#58492=CARTESIAN_POINT('Ctrl Pts',(0.818575647567586,-0.230726286157603,
-1.11581603739752));
#58493=CARTESIAN_POINT('Ctrl Pts',(0.830732477917423,0.18205408312639,-1.10538207479504));
#58494=CARTESIAN_POINT('Ctrl Pts',(0.647100797261757,0.551826151980974,
-1.09494811219256));
#58495=CARTESIAN_POINT('Ctrl Pts',(0.310930583933843,0.791574909217227,
-1.08451414959008));
#58496=CARTESIAN_POINT('Ctrl Pts',(-0.0985234799625261,0.844718114599206,
-1.0740801869876));
#58497=CARTESIAN_POINT('Ctrl Pts',(-0.484757379072011,0.698765466281204,
-1.06364622438512));
#58498=CARTESIAN_POINT('Ctrl Pts',(-0.756728010910764,0.388101050966172,
-1.05321226178264));
#58499=CARTESIAN_POINT('Ctrl Pts',(-0.850331447180054,-0.0140392876955686,
-1.04277829918015));
#58500=CARTESIAN_POINT('Ctrl Pts',(-0.743503406614725,-0.412872032986837,
-1.03234433657768));
#58501=CARTESIAN_POINT('Ctrl Pts',(-0.461424807647823,-0.714386145646098,
-1.02191037397519));
#58502=CARTESIAN_POINT('Ctrl Pts',(-0.070583950441432,-0.847513141979658,
-1.01147641137271));
#58503=CARTESIAN_POINT('Ctrl Pts',(0.336894159842268,-0.780873113300912,
-1.00104244877023));
#58504=CARTESIAN_POINT('Ctrl Pts',(0.664963173900127,-0.530174058353579,
-0.990608486167752));
#58505=CARTESIAN_POINT('Ctrl Pts',(0.836294104630411,-0.154507939527322,
-0.980174523565272));
#58506=CARTESIAN_POINT('Ctrl Pts',(0.810502659647238,0.25757712537611,-0.969740560962791));
#58507=CARTESIAN_POINT('Ctrl Pts',(0.593668115536935,0.608948854591682,
-0.959306598360311));
#58508=CARTESIAN_POINT('Ctrl Pts',(0.236900417487047,0.816785607236095,
-0.948872635757829));
#58509=CARTESIAN_POINT('Ctrl Pts',(-0.175706936751575,0.832098317777406,
-0.93843867315535));
#58510=CARTESIAN_POINT('Ctrl Pts',(-0.546898513860023,0.651277630891637,
-0.928004710552868));
#58511=CARTESIAN_POINT('Ctrl Pts',(-0.789180970390852,0.316944685067363,
-0.917570747950388));
#58512=CARTESIAN_POINT('Ctrl Pts',(-0.845446053461758,-0.0920951029197594,
-0.907136785347908));
#58513=CARTESIAN_POINT('Ctrl Pts',(-0.702431554241408,-0.479427209172013,
-0.896702822745426));
#58514=CARTESIAN_POINT('Ctrl Pts',(-0.393847334508687,-0.753753815530975,
-0.886268860142947));
#58515=CARTESIAN_POINT('Ctrl Pts',(0.0075704042826582,-0.850413561905815,
-0.875834897540465));
#58516=CARTESIAN_POINT('Ctrl Pts',(0.40720372762689,-0.746622837529438,
-0.865400934937985));
#58517=CARTESIAN_POINT('Ctrl Pts',(0.710855304480888,-0.46684609176493,
-0.854966972335505));
#58518=CARTESIAN_POINT('Ctrl Pts',(0.84695160373427,-0.0770293336317737,
-0.844533009733024));
#58519=CARTESIAN_POINT('Ctrl Pts',(0.783413448288198,0.330943962550491,
-0.834099047130544));
#58520=CARTESIAN_POINT('Ctrl Pts',(0.53521737866792,0.660910655746168,-0.823665084528062));
#58521=CARTESIAN_POINT('Ctrl Pts',(0.160865541628774,0.835094494547749,
-0.813231121925583));
#58522=CARTESIAN_POINT('Ctrl Pts',(-0.251403815775333,0.812438710747313,
-0.802797159323102));
#58523=CARTESIAN_POINT('Ctrl Pts',(-0.604414930500534,0.59828348556128,
-0.792363196720621));
#58524=CARTESIAN_POINT('Ctrl Pts',(-0.814959764354287,0.243107218714007,
-0.781929234118141));
#58525=CARTESIAN_POINT('Ctrl Pts',(-0.833410920788056,-0.169371704893337,
-0.771495271515659));
#58526=CARTESIAN_POINT('Ctrl Pts',(-0.65541928878181,-0.541928125492689,
-0.76106130891318));
#58527=CARTESIAN_POINT('Ctrl Pts',(-0.322939169195014,-0.786746992562985,
-0.750627346310698));
#58528=CARTESIAN_POINT('Ctrl Pts',(0.0856607483339347,-0.846122197736321,
-0.740193383708218));
#58529=CARTESIAN_POINT('Ctrl Pts',(0.474069622233808,-0.706058447001636,
-0.729759421105737));
#58530=CARTESIAN_POINT('Ctrl Pts',(0.750735829720999,-0.399570083064779,
-0.719325458503258));
#58531=CARTESIAN_POINT('Ctrl Pts',(0.850446544913026,0.00110070557588335,
-0.708891495900775));
#58532=CARTESIAN_POINT('Ctrl Pts',(0.749699014916824,0.401512047565219,
-0.698457533298296));
#58533=CARTESIAN_POINT('Ctrl Pts',(0.472240379621293,0.707283225562721,
-0.688023570695814));
#58534=CARTESIAN_POINT('Ctrl Pts',(0.0834702475924911,0.84634109853777,
-0.677589608093335));
#58535=CARTESIAN_POINT('Ctrl Pts',(-0.324974606449005,0.78590841862814,
-0.667155645490853));
#58536=CARTESIAN_POINT('Ctrl Pts',(-0.656819890853624,0.540229736580931,
-0.656721682888373));
#58537=CARTESIAN_POINT('Ctrl Pts',(-0.833846552603121,0.167213827236748,
-0.646287720285892));
#58538=CARTESIAN_POINT('Ctrl Pts',(-0.814327743398679,-0.245215953066854,
-0.635853757683411));
#58539=CARTESIAN_POINT('Ctrl Pts',(-0.602864230054735,-0.599846028100363,
-0.625419795080931));
#58540=CARTESIAN_POINT('Ctrl Pts',(-0.249299950511681,-0.813086755507764,
-0.61498583247845));
#58541=CARTESIAN_POINT('Ctrl Pts',(0.163026670890489,-0.834675291287356,
-0.604551869875971));
#58542=CARTESIAN_POINT('Ctrl Pts',(0.536926373445071,-0.659523014614649,
-0.594117907273488));
#58543=CARTESIAN_POINT('Ctrl Pts',(0.784267482446793,-0.328914963605851,
-0.58368394467101));
#58544=CARTESIAN_POINT('Ctrl Pts',(0.846749373394363,0.07922143626269,-0.573249982068528));
#58545=CARTESIAN_POINT('Ctrl Pts',(0.709644477235602,0.468684598889571,
-0.562816019466048));
#58546=CARTESIAN_POINT('Ctrl Pts',(0.405269706838339,0.74767439572747,-0.552382056863567));
#58547=CARTESIAN_POINT('Ctrl Pts',(0.00536905683500304,0.850430309041236,
-0.541948094261086));
#58548=CARTESIAN_POINT('Ctrl Pts',(-0.395797130335716,0.752731804114374,
-0.531514131658606));
#58549=CARTESIAN_POINT('Ctrl Pts',(-0.703670213228199,0.477607336964844,
-0.521080169056125));
#58550=CARTESIAN_POINT('Ctrl Pts',(-0.845681612069302,0.0899063307845272,
-0.510646206453645));
#58551=CARTESIAN_POINT('Ctrl Pts',(-0.788357905185793,-0.318986442718711,
-0.500212243851163));
#58552=CARTESIAN_POINT('Ctrl Pts',(-0.54521082915687,-0.652691113067544,
-0.489778281248684));
#58553=CARTESIAN_POINT('Ctrl Pts',(-0.173552435486475,-0.832550352497661,
-0.479344318646203));
#58554=CARTESIAN_POINT('Ctrl Pts',(0.239013898693356,-0.816169647523525,
-0.468910356043722));
#58555=CARTESIAN_POINT('Ctrl Pts',(0.595242410120839,-0.60741008429298,
-0.458476393441241));
#58556=CARTESIAN_POINT('Ctrl Pts',(0.811166689955888,-0.25547825428647,
-0.448042430838761));
#58557=CARTESIAN_POINT('Ctrl Pts',(0.835891355663177,0.15667220185756,-0.43760846823628));
#58558=CARTESIAN_POINT('Ctrl Pts',(0.663588571113163,0.531893547239619,
-0.4271745056338));
#58559=CARTESIAN_POINT('Ctrl Pts',(0.334871722342646,0.781742583516306,
-0.416740543031319));
#58560=CARTESIAN_POINT('Ctrl Pts',(-0.0727775393183082,0.84732754415147,
-0.406306580428839));
#58561=CARTESIAN_POINT('Ctrl Pts',(-0.463272450821895,0.713189437398579,
-0.395872617826358));
#58562=CARTESIAN_POINT('Ctrl Pts',(-0.74456969071411,0.410945875971156,
-0.385438655223877));
#58563=CARTESIAN_POINT('Ctrl Pts',(-0.8503648552362,0.0118385085176673,
-0.375004692621397));
#58564=CARTESIAN_POINT('Ctrl Pts',(-0.755721029601023,-0.390059306686192,
-0.364570730018916));
#58565=CARTESIAN_POINT('Ctrl Pts',(-0.482946653183773,-0.700016476572467,
-0.354136767416436));
#58566=CARTESIAN_POINT('Ctrl Pts',(-0.0963372107351823,-0.844973182506324,
-0.343702804813954));
#58567=CARTESIAN_POINT('Ctrl Pts',(0.312979817940922,-0.790761766178747,
-0.333268842211475));
#58568=CARTESIAN_POINT('Ctrl Pts',(0.648524561294601,-0.550160368159601,
-0.322834879608993));
#58569=CARTESIAN_POINT('Ctrl Pts',(0.831205969332432,-0.17988099945694,
-0.312400917006513));
#58570=CARTESIAN_POINT('Ctrl Pts',(0.817964316356759,0.232798011437269,
-0.301966954404032));
#58571=CARTESIAN_POINT('Ctrl Pts',(0.611920785515868,0.590604343299518,
-0.291532991801552));
#58572=CARTESIAN_POINT('Ctrl Pts',(0.261641771830845,0.809199678217181,
-0.281099029199071));
#58573=CARTESIAN_POINT('Ctrl Pts',(-0.150308664289158,0.837059044723433,
-0.270665066596591));
#58574=CARTESIAN_POINT('Ctrl Pts',(-0.526829940633299,0.667615720654165,
-0.26023110399411));
#58575=CARTESIAN_POINT('Ctrl Pts',(-0.779172437010211,0.340809105248274,
-0.249797141391629));
#58576=CARTESIAN_POINT('Ctrl Pts',(-0.847856686154441,-0.0663294394492073,
-0.239363178789149));
#58577=CARTESIAN_POINT('Ctrl Pts',(-0.716693103442289,-0.457833473536335,
-0.228929216186668));
#58578=CARTESIAN_POINT('Ctrl Pts',(-0.416598299086144,-0.741421929191927,
-0.218495253584188));
#58579=CARTESIAN_POINT('Ctrl Pts',(-0.0183072020772284,-0.850250118821529,
-0.208061290981707));
#58580=CARTESIAN_POINT('Ctrl Pts',(0.384298765226859,-0.758666652961295,
-0.197627328379227));
#58581=CARTESIAN_POINT('Ctrl Pts',(0.696322509060594,-0.488257754713517,
-0.187193365776746));
#58582=CARTESIAN_POINT('Ctrl Pts',(0.844215296492181,-0.102763035312441,
-0.176759403174265));
#58583=CARTESIAN_POINT('Ctrl Pts',(0.793120952222842,0.306956102035922,
-0.166325440571785));
#58584=CARTESIAN_POINT('Ctrl Pts',(0.555075924815356,0.644318467007069,
-0.155891477969304));
#58585=CARTESIAN_POINT('Ctrl Pts',(0.186203366191301,0.829817432539671,
-0.145457515366824));
#58586=CARTESIAN_POINT('Ctrl Pts',(-0.226576956355173,0.81970386523168,
-0.135023552764342));
#58587=CARTESIAN_POINT('Ctrl Pts',(-0.585915510641066,0.616411513065771,
-0.124589590161862));
#58588=CARTESIAN_POINT('Ctrl Pts',(-0.807221329288043,0.267758165995395,
-0.114155627559382));
#58589=CARTESIAN_POINT('Ctrl Pts',(-0.827788619517399,-0.00665018237018827,
-0.107199652491061));
#58590=CARTESIAN_POINT('Ctrl Pts',(-0.805186023504941,-0.13827082337233,
-0.103721664956901));
#58591=CARTESIAN_POINT('Ctrl Pts',(0.59113087362967,-0.567590438870545,
-1.12757052310293));
#58592=CARTESIAN_POINT('Ctrl Pts',(0.683912652131218,-0.470960598009107,
-1.12409253556877));
#58593=CARTESIAN_POINT('Ctrl Pts',(0.82111734424875,-0.231442668990131,
-1.11713656050045));
#58594=CARTESIAN_POINT('Ctrl Pts',(0.833311893543815,0.182619350617622,
-1.10670259789796));
#58595=CARTESIAN_POINT('Ctrl Pts',(0.649110049900926,0.553539577591918,
-1.09626863529548));
#58596=CARTESIAN_POINT('Ctrl Pts',(0.311896021207629,0.794032746862487,
-1.085834672693));
#58597=CARTESIAN_POINT('Ctrl Pts',(-0.0988293942380879,0.847340965934938,
-1.07540071009052));
#58598=CARTESIAN_POINT('Ctrl Pts',(-0.486262551456734,0.700935132557606,
-1.06496674748804));
#58599=CARTESIAN_POINT('Ctrl Pts',(-0.759077651294704,0.389306105187754,
-1.05453278488556));
#58600=CARTESIAN_POINT('Ctrl Pts',(-0.852971726711211,-0.014082879866262,
-1.04409882228308));
#58601=CARTESIAN_POINT('Ctrl Pts',(-0.745811984820576,-0.414154000672726,
-1.0336648596806));
#58602=CARTESIAN_POINT('Ctrl Pts',(-0.4628575318427,-0.716604314872258,
-1.02323089707812));
#58603=CARTESIAN_POINT('Ctrl Pts',(-0.0708031136070384,-0.850144670496582,
-1.01279693447564));
#58604=CARTESIAN_POINT('Ctrl Pts',(0.337940216291625,-0.7832977245458,-1.00236297187316));
#58605=CARTESIAN_POINT('Ctrl Pts',(0.667027884744328,-0.531820248945429,
-0.991929009270678));
#58606=CARTESIAN_POINT('Ctrl Pts',(0.838890798054124,-0.154987686725414,
-0.981495046668197));
#58607=CARTESIAN_POINT('Ctrl Pts',(0.813019270631118,0.258376902423271,
-0.971061084065717));
#58608=CARTESIAN_POINT('Ctrl Pts',(0.595511455199314,0.610839640952936,
-0.960627121463234));
#58609=CARTESIAN_POINT('Ctrl Pts',(0.237635993349262,0.819321726773045,
-0.950193158860757));
#58610=CARTESIAN_POINT('Ctrl Pts',(-0.176252506838998,0.83468198328421,
-0.939759196258273));
#58611=CARTESIAN_POINT('Ctrl Pts',(-0.548596633896843,0.653299848115927,
-0.929325233655794));
#58612=CARTESIAN_POINT('Ctrl Pts',(-0.791631377522395,0.317928798402169,
-0.918891271053314));
#58613=CARTESIAN_POINT('Ctrl Pts',(-0.848071163691741,-0.092381058239788,
-0.908457308450832));
#58614=CARTESIAN_POINT('Ctrl Pts',(-0.704612604411761,-0.480915830789204,
-0.898023345848353));
#58615=CARTESIAN_POINT('Ctrl Pts',(-0.395070230591342,-0.756094221336819,
-0.887589383245871));
#58616=CARTESIAN_POINT('Ctrl Pts',(0.00759391039004866,-0.853054096250918,
-0.877155420643392));
#58617=CARTESIAN_POINT('Ctrl Pts',(0.408468095313881,-0.748941101646619,
-0.86672145804091));
#58618=CARTESIAN_POINT('Ctrl Pts',(0.713062510398055,-0.468295649009077,
-0.856287495438431));
#58619=CARTESIAN_POINT('Ctrl Pts',(0.849581388698288,-0.0772685097340202,
-0.845853532835948));
#58620=CARTESIAN_POINT('Ctrl Pts',(0.785845947261971,0.331971543645811,
-0.835419570233469));
#58621=CARTESIAN_POINT('Ctrl Pts',(0.536879228776823,0.662962783515191,
-0.824985607630987));
#58622=CARTESIAN_POINT('Ctrl Pts',(0.161365029180057,0.837687463184462,
-0.814551645028508));
#58623=CARTESIAN_POINT('Ctrl Pts',(-0.252184424692901,0.814961333169054,
-0.804117682426026));
#58624=CARTESIAN_POINT('Ctrl Pts',(-0.606291639027032,0.600141155949544,
-0.793683719823546));
#58625=CARTESIAN_POINT('Ctrl Pts',(-0.817490214648176,0.243862066695402,
-0.783249757221066));
#58626=CARTESIAN_POINT('Ctrl Pts',(-0.835998661927778,-0.16989760408391,
-0.772815794618584));
#58627=CARTESIAN_POINT('Ctrl Pts',(-0.657454365854888,-0.543610812472342,
-0.762381832016105));
#58628=CARTESIAN_POINT('Ctrl Pts',(-0.323941895404749,-0.789189842192652,
-0.751947869413623));
#58629=CARTESIAN_POINT('Ctrl Pts',(0.0859267249812208,-0.848749407394488,
-0.741513906811143));
#58630=CARTESIAN_POINT('Ctrl Pts',(0.47554160854206,-0.708250758675002,
-0.731079944208662));
#58631=CARTESIAN_POINT('Ctrl Pts',(0.753066864680074,-0.400810748283291,
-0.720645981606182));
#58632=CARTESIAN_POINT('Ctrl Pts',(0.853087181670372,0.00110412326700143,
-0.710212019003701));
#58633=CARTESIAN_POINT('Ctrl Pts',(0.752026830565646,0.402758742584041,
-0.699778056401221));
#58634=CARTESIAN_POINT('Ctrl Pts',(0.473706686130727,0.709479340173859,
-0.68934409379874));
#58635=CARTESIAN_POINT('Ctrl Pts',(0.0837294227343689,0.848968987882985,
-0.678910131196259));
#58636=CARTESIAN_POINT('Ctrl Pts',(-0.325983652691977,0.788348664485508,
-0.668476168593779));
#58637=CARTESIAN_POINT('Ctrl Pts',(-0.658859316796523,0.541907150062543,
-0.658042205991297));
#58638=CARTESIAN_POINT('Ctrl Pts',(-0.83643564637975,0.167733026216601,
-0.647608243388819));
#58639=CARTESIAN_POINT('Ctrl Pts',(-0.816856231267325,-0.245977348668999,
-0.637174280786336));
#58640=CARTESIAN_POINT('Ctrl Pts',(-0.604736123655918,-0.601708550183643,
-0.626740318183857));
#58641=CARTESIAN_POINT('Ctrl Pts',(-0.250074026927023,-0.815611390108666,
-0.616306355581375));
#58642=CARTESIAN_POINT('Ctrl Pts',(0.163532868748728,-0.837266958297831,
-0.605872392978896));
#58643=CARTESIAN_POINT('Ctrl Pts',(0.538593529983231,-0.661570833757573,
-0.595438430376415));
#58644=CARTESIAN_POINT('Ctrl Pts',(0.786702633196865,-0.329936244658886,
-0.585004467773934));
#58645=CARTESIAN_POINT('Ctrl Pts',(0.849378530433119,0.0794674188442131,
-0.574570505171454));
#58646=CARTESIAN_POINT('Ctrl Pts',(0.711847923533838,0.470139864698849,
-0.564136542568972));
#58647=CARTESIAN_POINT('Ctrl Pts',(0.406528069390245,0.749995924933148,
-0.553702579966493));
#58648=CARTESIAN_POINT('Ctrl Pts',(0.0053857277579616,0.853070895386196,
-0.543268617364011));
#58649=CARTESIAN_POINT('Ctrl Pts',(-0.397026080534959,0.755069036574495,
-0.532834654761531));
#58650=CARTESIAN_POINT('Ctrl Pts',(-0.705855109435038,0.479090307878314,
-0.52240069215905));
#58651=CARTESIAN_POINT('Ctrl Pts',(-0.84830745370885,0.0901854899664981,
-0.511966729556569));
#58652=CARTESIAN_POINT('Ctrl Pts',(-0.7908057566996,-0.319976895711644,
-0.50153276695409));
#58653=CARTESIAN_POINT('Ctrl Pts',(-0.546903708932309,-0.654717719154274,
-0.491098804351608));
#58654=CARTESIAN_POINT('Ctrl Pts',(-0.174091315846697,-0.835135421572604,
-0.480664841749129));
#58655=CARTESIAN_POINT('Ctrl Pts',(0.239756036914954,-0.818703854504989,
-0.470230879146647));
#58656=CARTESIAN_POINT('Ctrl Pts',(0.597090637969018,-0.609296092772832,
-0.459796916544167));
#58657=CARTESIAN_POINT('Ctrl Pts',(0.813685362752721,-0.256271514336742,
-0.449362953941686));
#58658=CARTESIAN_POINT('Ctrl Pts',(0.838486798553873,0.157158669087693,
-0.438928991339206));
#58659=CARTESIAN_POINT('Ctrl Pts',(0.665649013810141,0.533545076851018,
-0.428495028736725));
#58660=CARTESIAN_POINT('Ctrl Pts',(0.335911499133207,0.784169894454499,
-0.418061066134244));
#58661=CARTESIAN_POINT('Ctrl Pts',(-0.0730035135980353,0.849958496410589,
-0.407627103531764));
#58662=CARTESIAN_POINT('Ctrl Pts',(-0.464710911909924,0.715403890799101,
-0.397193140929283));
#58663=CARTESIAN_POINT('Ctrl Pts',(-0.746881579809863,0.412221863029791,
-0.386759178326802));
#58664=CARTESIAN_POINT('Ctrl Pts',(-0.853005238347077,0.01187526708989,
-0.376325215724322));
#58665=CARTESIAN_POINT('Ctrl Pts',(-0.758067543607107,-0.391270440941413,
-0.365891253121841));
#58666=CARTESIAN_POINT('Ctrl Pts',(-0.484446202675581,-0.702190027925983,
-0.355457290519361));
#58667=CARTESIAN_POINT('Ctrl Pts',(-0.0966363378011808,-0.847596824471873,
-0.34502332791688));
#58668=CARTESIAN_POINT('Ctrl Pts',(0.313951620362259,-0.793217081681621,
-0.3345893653144));
#58669=CARTESIAN_POINT('Ctrl Pts',(0.650538230236919,-0.551868616254977,
-0.324155402711919));
#58670=CARTESIAN_POINT('Ctrl Pts',(0.833786864097282,-0.180439530010112,
-0.313721440109438));
#58671=CARTESIAN_POINT('Ctrl Pts',(0.820504095785433,0.233520849327355,
-0.303287477506958));
#58672=CARTESIAN_POINT('Ctrl Pts',(0.613820799724295,0.592438169948661,
-0.292853514904477));
#58673=CARTESIAN_POINT('Ctrl Pts',(0.262454169604739,0.811712243442553,
-0.282419552301996));
#58674=CARTESIAN_POINT('Ctrl Pts',(-0.150775372733263,0.839658113287937,
-0.271985589699516));
#58675=CARTESIAN_POINT('Ctrl Pts',(-0.528465747745014,0.66968866765364,
-0.261551627097035));
#58676=CARTESIAN_POINT('Ctrl Pts',(-0.78159176764234,0.341867317610358,
-0.251117664494555));
#58677=CARTESIAN_POINT('Ctrl Pts',(-0.850489281400512,-0.0665353923691108,
-0.240683701892074));
#58678=CARTESIAN_POINT('Ctrl Pts',(-0.718918435725102,-0.459255046614004,
-0.230249739289594));
#58679=CARTESIAN_POINT('Ctrl Pts',(-0.417891836923547,-0.743724044456582,
-0.219815776687113));
#58680=CARTESIAN_POINT('Ctrl Pts',(-0.0183640459379991,-0.852890145736156,
-0.209381814084632));
#58681=CARTESIAN_POINT('Ctrl Pts',(0.385492012985996,-0.761022313010095,
-0.198947851482152));
#58682=CARTESIAN_POINT('Ctrl Pts',(0.698484590670027,-0.489773795410247,
-0.188513888879671));
#58683=CARTESIAN_POINT('Ctrl Pts',(0.846836585170214,-0.103082114107112,
-0.17807992627719));
#58684=CARTESIAN_POINT('Ctrl Pts',(0.795583593099748,0.307909199916563,
-0.16764596367471));
#58685=CARTESIAN_POINT('Ctrl Pts',(0.556799435517521,0.646319077797019,
-0.157212001072229));
#58686=CARTESIAN_POINT('Ctrl Pts',(0.186781528084307,0.83239401241337,-0.146778038469749));
#58687=CARTESIAN_POINT('Ctrl Pts',(-0.227280478634921,0.822249052826759,
-0.136344075867268));
#58688=CARTESIAN_POINT('Ctrl Pts',(-0.587734776932399,0.618325457284273,
-0.125910113264787));
#58689=CARTESIAN_POINT('Ctrl Pts',(-0.809727755002957,0.268589584372264,
-0.115476150662307));
#58690=CARTESIAN_POINT('Ctrl Pts',(-0.830358898319076,-0.00667087734731289,
-0.108520175593986));
#58691=CARTESIAN_POINT('Ctrl Pts',(-0.807686129085189,-0.138700154790173,
-0.105042188059826));
#58692=CARTESIAN_POINT('Ctrl Pts',(0.594875448103835,-0.571185894232442,
-1.13205842314276));
#58693=CARTESIAN_POINT('Ctrl Pts',(0.688244416305429,-0.473944510369919,
-1.1285804356086));
#58694=CARTESIAN_POINT('Ctrl Pts',(0.826319063393535,-0.23290837533709,
-1.12162446054028));
#58695=CARTESIAN_POINT('Ctrl Pts',(0.83859038834421,0.183775983334779,-1.1111904979378));
#58696=CARTESIAN_POINT('Ctrl Pts',(0.653221937147493,0.557046083095294,
-1.10075653533532));
#58697=CARTESIAN_POINT('Ctrl Pts',(0.313871699922475,0.799062532067006,
-1.09032257273284));
#58698=CARTESIAN_POINT('Ctrl Pts',(-0.0994554132647858,0.852708501700447,
-1.07988861013036));
#58699=CARTESIAN_POINT('Ctrl Pts',(-0.489342809626878,0.705375220702394,
-1.06945464752788));
#58700=CARTESIAN_POINT('Ctrl Pts',(-0.763886051959433,0.391772185135788,
-1.0590206849254));
#58701=CARTESIAN_POINT('Ctrl Pts',(-0.858374910495865,-0.0141720913963219,
-1.04858672232292));
#58702=CARTESIAN_POINT('Ctrl Pts',(-0.75053635735818,-0.416777473112896,
-1.03815275972044));
#58703=CARTESIAN_POINT('Ctrl Pts',(-0.465789520808082,-0.721143672414923,
-1.02771879711796));
#58704=CARTESIAN_POINT('Ctrl Pts',(-0.0712516182343091,-0.855529943231548,
-1.01728483451548));
#58705=CARTESIAN_POINT('Ctrl Pts',(0.340080911027159,-0.788259553404192,
-1.006850871913));
#58706=CARTESIAN_POINT('Ctrl Pts',(0.671253197851214,-0.53518908404983,
-0.996416909310516));
#58707=CARTESIAN_POINT('Ctrl Pts',(0.844204783065116,-0.155969462060879,
-0.985982946708035));
#58708=CARTESIAN_POINT('Ctrl Pts',(0.818169371553483,0.260013600576981,
-0.975548984105555));
#58709=CARTESIAN_POINT('Ctrl Pts',(0.599283744716546,0.614709027432673,
-0.965115021503073));
#58710=CARTESIAN_POINT('Ctrl Pts',(0.239141307420071,0.82451175082322,-0.954681058900594));
#58711=CARTESIAN_POINT('Ctrl Pts',(-0.177368984921704,0.839969307441941,
-0.944247096298111));
#58712=CARTESIAN_POINT('Ctrl Pts',(-0.552071739738338,0.657438200377167,
-0.933813133695633));
#58713=CARTESIAN_POINT('Ctrl Pts',(-0.796645996016163,0.31994273023519,
-0.923379171093151));
#58714=CARTESIAN_POINT('Ctrl Pts',(-0.853443302115344,-0.092966249499057,
-0.912945208490671));
#58715=CARTESIAN_POINT('Ctrl Pts',(-0.709075999240425,-0.483962210060304,
-0.90251124588819));
#58716=CARTESIAN_POINT('Ctrl Pts',(-0.397572817705153,-0.760883728388117,
-0.89207728328571));
#58717=CARTESIAN_POINT('Ctrl Pts',(0.00764201429865589,-0.858457799247159,
-0.881643320683229));
#58718=CARTESIAN_POINT('Ctrl Pts',(0.411055551701718,-0.753685296994478,
-0.871209358080748));
#58719=CARTESIAN_POINT('Ctrl Pts',(0.717579431471203,-0.471262085267673,
-0.860775395478267));
#58720=CARTESIAN_POINT('Ctrl Pts',(0.854963093698934,-0.077757969991451,
-0.850341432875787));
#58721=CARTESIAN_POINT('Ctrl Pts',(0.790823917731154,0.334074429773344,
-0.839907470273306));
#58722=CARTESIAN_POINT('Ctrl Pts',(0.540280110279979,0.667162345999428,
-0.829473507670825));
#58723=CARTESIAN_POINT('Ctrl Pts',(0.162387201977175,0.842993825670224,
-0.819039545068346));
#58724=CARTESIAN_POINT('Ctrl Pts',(-0.253781896338945,0.82012373613643,
-0.808605582465865));
#58725=CARTESIAN_POINT('Ctrl Pts',(-0.610132216032369,0.60394277249038,
-0.798171619863384));
#58726=CARTESIAN_POINT('Ctrl Pts',(-0.822668636909621,0.245406820054244,
-0.787737657260904));
#58727=CARTESIAN_POINT('Ctrl Pts',(-0.841294326638981,-0.170973826795068,
-0.777303694658423));
#58728=CARTESIAN_POINT('Ctrl Pts',(-0.661619035061959,-0.547054335443539,
-0.766869732055942));
#58729=CARTESIAN_POINT('Ctrl Pts',(-0.325993917425955,-0.794188994689023,
-0.756435769453461));
#58730=CARTESIAN_POINT('Ctrl Pts',(0.0864710310261406,-0.854125842178519,
-0.746001806850981));
#58731=CARTESIAN_POINT('Ctrl Pts',(0.478553944601615,-0.71273719952737,
-0.735567844248499));
#58732=CARTESIAN_POINT('Ctrl Pts',(0.757837194827812,-0.403349698920676,
-0.725133881646021));
#58733=CARTESIAN_POINT('Ctrl Pts',(0.858491094247377,0.00111111737702571,
-0.714699919043538));
#58734=CARTESIAN_POINT('Ctrl Pts',(0.756790572578487,0.405310032863995,
-0.704265956441059));
#58735=CARTESIAN_POINT('Ctrl Pts',(0.476707398805814,0.713973563521563,
-0.693831993838578));
#58736=CARTESIAN_POINT('Ctrl Pts',(0.084259809886235,0.854346813607812,
-0.683398031236097));
#58737=CARTESIAN_POINT('Ctrl Pts',(-0.328048608300887,0.793342488510314,
-0.672964068633617));
#58738=CARTESIAN_POINT('Ctrl Pts',(-0.663032885717748,0.545339881120648,
-0.662530106031136));
#58739=CARTESIAN_POINT('Ctrl Pts',(-0.841734079185264,0.168795537328509,
-0.652096143428656));
#58740=CARTESIAN_POINT('Ctrl Pts',(-0.822030637537395,-0.247535501360414,
-0.641662180826174));
#58741=CARTESIAN_POINT('Ctrl Pts',(-0.608566847191108,-0.605520095441727,
-0.631228218223695));
#58742=CARTESIAN_POINT('Ctrl Pts',(-0.251658130179691,-0.820777910885976,
-0.620794255621213));
#58743=CARTESIAN_POINT('Ctrl Pts',(0.164568773806467,-0.842570657079702,
-0.610360293018733));
#58744=CARTESIAN_POINT('Ctrl Pts',(0.542005270791329,-0.665761578884141,
-0.599926330416252));
#58745=CARTESIAN_POINT('Ctrl Pts',(0.791686030375065,-0.332026238109064,
-0.589492367813772));
#58746=CARTESIAN_POINT('Ctrl Pts',(0.85475895042051,0.0799708081734412,
-0.57905840521129));
#58747=CARTESIAN_POINT('Ctrl Pts',(0.716357150761197,0.473117983210515,
-0.568624442608811));
#58748=CARTESIAN_POINT('Ctrl Pts',(0.409103236611469,0.754746802098496,
-0.558190480006329));
#58749=CARTESIAN_POINT('Ctrl Pts',(0.00541984385136075,0.858474704797127,
-0.54775651740385));
#58750=CARTESIAN_POINT('Ctrl Pts',(-0.399541057053304,0.759852049554789,
-0.537322554801368));
#58751=CARTESIAN_POINT('Ctrl Pts',(-0.710326374957925,0.482125123306199,
-0.526888592198889));
#58752=CARTESIAN_POINT('Ctrl Pts',(-0.853681088920773,0.090756773317092,
-0.516454629596408));
#58753=CARTESIAN_POINT('Ctrl Pts',(-0.795815145266697,-0.322003801294379,
-0.506020666993927));
#58754=CARTESIAN_POINT('Ctrl Pts',(-0.550368090878974,-0.658865052970729,
-0.495586704391446));
#58755=CARTESIAN_POINT('Ctrl Pts',(-0.175194103781465,-0.840425618055573,
-0.485152741788965));
#58756=CARTESIAN_POINT('Ctrl Pts',(0.241274780474974,-0.823889964613383,
-0.474718779186485));
#58757=CARTESIAN_POINT('Ctrl Pts',(0.600872930889906,-0.613155701602504,
-0.464284816584005));
#58758=CARTESIAN_POINT('Ctrl Pts',(0.818839683037894,-0.257894875804606,
-0.453850853981524));
#58759=CARTESIAN_POINT('Ctrl Pts',(0.843798224459354,0.158154196539887,
-0.443416891379044));
#58760=CARTESIAN_POINT('Ctrl Pts',(0.669865592320389,0.536924838044416,
-0.432982928776562));
#58761=CARTESIAN_POINT('Ctrl Pts',(0.338039343055762,0.78913724790465,-0.422548966174082));
#58762=CARTESIAN_POINT('Ctrl Pts',(-0.0734659570783441,0.855342590214102,
-0.412115003571602));
#58763=CARTESIAN_POINT('Ctrl Pts',(-0.467654640517619,0.719935643433754,
-0.401681040969121));
#58764=CARTESIAN_POINT('Ctrl Pts',(-0.751612729039848,0.414833097799243,
-0.391247078366641));
#58765=CARTESIAN_POINT('Ctrl Pts',(-0.85840863185104,0.0119504914122616,
-0.380813115764159));
#58766=CARTESIAN_POINT('Ctrl Pts',(-0.762869550742065,-0.393748958145996,
-0.370379153161679));
#58767=CARTESIAN_POINT('Ctrl Pts',(-0.487514945218854,-0.706638076853403,
-0.359945190559198));
#58768=CARTESIAN_POINT('Ctrl Pts',(-0.0972484842880521,-0.852965958176228,
-0.349511227956718));
#58769=CARTESIAN_POINT('Ctrl Pts',(0.315940358613552,-0.798241744877078,
-0.339077265354237));
#58770=CARTESIAN_POINT('Ctrl Pts',(0.654659088924843,-0.555364448591695,
-0.328643302751756));
#58771=CARTESIAN_POINT('Ctrl Pts',(0.839068518092748,-0.181582530945499,
-0.318209340149276));
#58772=CARTESIAN_POINT('Ctrl Pts',(0.825701609589117,0.23500009586131,-0.307775377546795));
#58773=CARTESIAN_POINT('Ctrl Pts',(0.617709070479456,0.596190991632762,
-0.297341414944315));
#58774=CARTESIAN_POINT('Ctrl Pts',(0.264116695332044,0.816854064938795,
-0.286907452341834));
#58775=CARTESIAN_POINT('Ctrl Pts',(-0.151730464954603,0.844976958912708,
-0.276473489739354));
#58776=CARTESIAN_POINT('Ctrl Pts',(-0.531813333742569,0.673930835536438,
-0.266039527136873));
#58777=CARTESIAN_POINT('Ctrl Pts',(-0.786542789844424,0.344032888819267,
-0.255605564534393));
#58778=CARTESIAN_POINT('Ctrl Pts',(-0.855876737496279,-0.0669568631605798,
-0.245171601931911));
#58779=CARTESIAN_POINT('Ctrl Pts',(-0.723472451346344,-0.462164215102111,
-0.234737639329432));
#58780=CARTESIAN_POINT('Ctrl Pts',(-0.420538988411855,-0.748435191644752,
-0.22430367672695));
#58781=CARTESIAN_POINT('Ctrl Pts',(-0.0184803735586183,-0.858292811196645,
-0.21386971412447));
#58782=CARTESIAN_POINT('Ctrl Pts',(0.387933926300151,-0.765843035246912,
-0.203435751521989));
#58783=CARTESIAN_POINT('Ctrl Pts',(0.702909167805231,-0.492876289710399,
-0.193001788919509));
#58784=CARTESIAN_POINT('Ctrl Pts',(0.852200902248736,-0.103735083894892,
-0.182567826317028));
#58785=CARTESIAN_POINT('Ctrl Pts',(0.800623248743806,0.309859647074913,
-0.172133863714547));
#58786=CARTESIAN_POINT('Ctrl Pts',(0.560326498983083,0.650413239900031,
-0.161699901112067));
#58787=CARTESIAN_POINT('Ctrl Pts',(0.187964709191458,0.837666784744464,
-0.151265938509586));
#58788=CARTESIAN_POINT('Ctrl Pts',(-0.228720208214099,0.827457735607706,
-0.140831975907105));
#58789=CARTESIAN_POINT('Ctrl Pts',(-0.591457779048179,0.622242032554339,
-0.130398013304625));
#58790=CARTESIAN_POINT('Ctrl Pts',(-0.814857060568085,0.270291466147323,
-0.119964050702144));
#58791=CARTESIAN_POINT('Ctrl Pts',(-0.83561875211749,-0.00671391055875398,
-0.113008075633824));
#58792=CARTESIAN_POINT('Ctrl Pts',(-0.812802493323685,-0.139578764049745,
-0.109530088099664));
#58793=CARTESIAN_POINT('Ctrl Pts',(0.596426278379627,-0.572674966240212,
-1.13871522674109));
#58794=CARTESIAN_POINT('Ctrl Pts',(0.690040836764286,-0.475177806505636,
-1.13523723920693));
#58795=CARTESIAN_POINT('Ctrl Pts',(0.828472169960176,-0.233517118585343,
-1.12828126413861));
#58796=CARTESIAN_POINT('Ctrl Pts',(0.840777371648049,0.1842558308649,-1.11784730153613));
#58797=CARTESIAN_POINT('Ctrl Pts',(0.654924723121757,0.558498066470774,
-1.10741333893365));
#58798=CARTESIAN_POINT('Ctrl Pts',(0.314690182553946,0.801146035838714,
-1.09697937633117));
#58799=CARTESIAN_POINT('Ctrl Pts',(-0.0997147922563187,0.854931601464747,
-1.08654541372869));
#58800=CARTESIAN_POINT('Ctrl Pts',(-0.490618589981848,0.707214329023195,
-1.07611145112621));
#58801=CARTESIAN_POINT('Ctrl Pts',(-0.765877684119502,0.392793594264132,
-1.06567748852373));
#58802=CARTESIAN_POINT('Ctrl Pts',(-0.860612864682261,-0.0142090290307373,
-1.05524352592125));
#58803=CARTESIAN_POINT('Ctrl Pts',(-0.752493169135759,-0.417864105985997,
-1.04480956331877));
#58804=CARTESIAN_POINT('Ctrl Pts',(-0.467003929674391,-0.723023842952482,
-1.03437560071629));
#58805=CARTESIAN_POINT('Ctrl Pts',(-0.0714373875773983,-0.857760491803007,
-1.02394163811381));
#58806=CARTESIAN_POINT('Ctrl Pts',(0.340967574370286,-0.790314711499322,
-1.01350767551132));
#58807=CARTESIAN_POINT('Ctrl Pts',(0.673003296155669,-0.536584435271311,
-1.00307371290884));
#58808=CARTESIAN_POINT('Ctrl Pts',(0.846405803153587,-0.156376107134292,
-0.992639750306363));
#58809=CARTESIAN_POINT('Ctrl Pts',(0.820302511565669,0.260691510764421,
-0.982205787703882));
#58810=CARTESIAN_POINT('Ctrl Pts',(0.600846203873045,0.616311703562283,
-0.971771825101402));
#58811=CARTESIAN_POINT('Ctrl Pts',(0.239764799219732,0.826661426818634,
-0.961337862498921));
#58812=CARTESIAN_POINT('Ctrl Pts',(-0.177831423260388,0.842159284588734,
-0.950903899896442));
#58813=CARTESIAN_POINT('Ctrl Pts',(-0.553511107201048,0.659152280411276,
-0.940469937293959));
#58814=CARTESIAN_POINT('Ctrl Pts',(-0.798723020136244,0.320776888411997,
-0.930035974691481));
#58815=CARTESIAN_POINT('Ctrl Pts',(-0.855668408795538,-0.0932086321197877,
-0.919602012088999));
#58816=CARTESIAN_POINT('Ctrl Pts',(-0.710924709912798,-0.485224001607961,
-0.909168049486517));
#58817=CARTESIAN_POINT('Ctrl Pts',(-0.398609373888874,-0.762867512737827,
-0.89873408688404));
#58818=CARTESIAN_POINT('Ctrl Pts',(0.00766193864182875,-0.860695979777121,
-0.888300124281556));
#58819=CARTESIAN_POINT('Ctrl Pts',(0.412127260215948,-0.755650313515053,
-0.877866161679077));
#58820=CARTESIAN_POINT('Ctrl Pts',(0.719450312385613,-0.472490764912427,
-0.867432199076596));
#58821=CARTESIAN_POINT('Ctrl Pts',(0.857192162794717,-0.0779607014182988,
-0.856998236474115));
#58822=CARTESIAN_POINT('Ctrl Pts',(0.792885762468365,0.334945432267616,
-0.846564273871635));
#58823=CARTESIAN_POINT('Ctrl Pts',(0.541688734471801,0.668901778939057,
-0.836130311269154));
#58824=CARTESIAN_POINT('Ctrl Pts',(0.162810579659971,0.845191688359986,
-0.825696348666674));
#58825=CARTESIAN_POINT('Ctrl Pts',(-0.254443559264954,0.822261971679499,
-0.815262386064192));
#58826=CARTESIAN_POINT('Ctrl Pts',(-0.611722959395606,0.605517378668961,
-0.804828423461713));
#58827=CARTESIAN_POINT('Ctrl Pts',(-0.824813507545726,0.246046647390084,
-0.794394460859231));
#58828=CARTESIAN_POINT('Ctrl Pts',(-0.84348775837634,-0.171419591619667,
-0.783960498256752));
#58829=CARTESIAN_POINT('Ctrl Pts',(-0.663344015420907,-0.548480621469044,
-0.77352653565427));
#58830=CARTESIAN_POINT('Ctrl Pts',(-0.326843852320352,-0.79625961289154,
-0.76309257305179));
#58831=CARTESIAN_POINT('Ctrl Pts',(0.0866964792406474,-0.856352728383039,
-0.752658610449309));
#58832=CARTESIAN_POINT('Ctrl Pts',(0.479801635661557,-0.71459545572183,
-0.742224647846828));
#58833=CARTESIAN_POINT('Ctrl Pts',(0.759813036221547,-0.404401316651656,
-0.731790685244349));
#58834=CARTESIAN_POINT('Ctrl Pts',(0.860729361584666,0.00111401429436048,
-0.721356722641867));
#58835=CARTESIAN_POINT('Ctrl Pts',(0.758763685207286,0.406366761598998,
-0.710922760039387));
#58836=CARTESIAN_POINT('Ctrl Pts',(0.477950275531433,0.715835043177703,
-0.700488797436906));
#58837=CARTESIAN_POINT('Ctrl Pts',(0.0844794929808862,0.856574275931451,
-0.690054834834426));
#58838=CARTESIAN_POINT('Ctrl Pts',(-0.328903900207727,0.795410899692695,
-0.679620872231945));
#58839=CARTESIAN_POINT('Ctrl Pts',(-0.664761552283533,0.546761697202158,
-0.669186909629465));
#58840=CARTESIAN_POINT('Ctrl Pts',(-0.843928657450257,0.16923562289307,
-0.658752947026984));
#58841=CARTESIAN_POINT('Ctrl Pts',(-0.82417384477458,-0.248180878617356,
-0.648318984424504));
#58842=CARTESIAN_POINT('Ctrl Pts',(-0.610153509307644,-0.607098814033897,
-0.637885021822023));
#58843=CARTESIAN_POINT('Ctrl Pts',(-0.252314255999422,-0.822917852000584,
-0.627451059219542));
#58844=CARTESIAN_POINT('Ctrl Pts',(0.164997839307108,-0.844767416479698,
-0.617017096617061));
#58845=CARTESIAN_POINT('Ctrl Pts',(0.543418392840445,-0.667497359728489,
-0.606583134014581));
#58846=CARTESIAN_POINT('Ctrl Pts',(0.793750122821745,-0.33289190053569,
-0.596149171412101));
#58847=CARTESIAN_POINT('Ctrl Pts',(0.856987487271739,0.0801793089360829,
-0.58571520880962));
#58848=CARTESIAN_POINT('Ctrl Pts',(0.718224844931966,0.474351501572674,
-0.575281246207139));
#58849=CARTESIAN_POINT('Ctrl Pts',(0.410169855028622,0.756714586186626,
-0.564847283604659));
#58850=CARTESIAN_POINT('Ctrl Pts',(0.0054339745273192,0.860712929403662,
-0.554413321002177));
#58851=CARTESIAN_POINT('Ctrl Pts',(-0.4005827448517,0.761833144099726,-0.543979358399698));
#58852=CARTESIAN_POINT('Ctrl Pts',(-0.712178345624292,0.483382125182182,
-0.533545395797216));
#58853=CARTESIAN_POINT('Ctrl Pts',(-0.855906815559752,0.0909933953656075,
-0.523111433194736));
#58854=CARTESIAN_POINT('Ctrl Pts',(-0.797890003186724,-0.32284333311451,
-0.512677470592255));
#58855=CARTESIAN_POINT('Ctrl Pts',(-0.551803016563766,-0.660582853117555,
-0.502243507989775));
#58856=CARTESIAN_POINT('Ctrl Pts',(-0.175650871758218,-0.842616784886446,
-0.491809545387294));
#58857=CARTESIAN_POINT('Ctrl Pts',(0.24190383471219,-0.826038019508388,
-0.481375582784813));
#58858=CARTESIAN_POINT('Ctrl Pts',(0.602439533344009,-0.614754327830273,
-0.470941620182333));
#58859=CARTESIAN_POINT('Ctrl Pts',(0.820974570783732,-0.258567262135502,
-0.460507657579852));
#58860=CARTESIAN_POINT('Ctrl Pts',(0.845998184386402,0.15856653788477,-0.450073694977372));
#58861=CARTESIAN_POINT('Ctrl Pts',(0.671612073193297,0.538324714333902,
-0.439639732374891));
#58862=CARTESIAN_POINT('Ctrl Pts',(0.338920682915139,0.791194695137899,
-0.429205769772411));
#58863=CARTESIAN_POINT('Ctrl Pts',(-0.0736574983223148,0.85757264873735,
-0.41877180716993));
#58864=CARTESIAN_POINT('Ctrl Pts',(-0.468873914793169,0.72181266748964,
-0.40833784456745));
#58865=CARTESIAN_POINT('Ctrl Pts',(-0.753572341938536,0.415914655172892,
-0.397903881964969));
#58866=CARTESIAN_POINT('Ctrl Pts',(-0.860646684191481,0.0119816488637972,
-0.387469919362488));
#58867=CARTESIAN_POINT('Ctrl Pts',(-0.764858512548966,-0.394775544721155,
-0.377035956760008));
#58868=CARTESIAN_POINT('Ctrl Pts',(-0.488785999497304,-0.708480431348439,
-0.366601994157527));
#58869=CARTESIAN_POINT('Ctrl Pts',(-0.097502031596093,-0.855189820319157,
-0.356168031555046));
#58870=CARTESIAN_POINT('Ctrl Pts',(0.316764081759707,-0.800322929452836,
-0.345734068952566));
#58871=CARTESIAN_POINT('Ctrl Pts',(0.656365923236636,-0.556812400837165,
-0.335300106350085));
#58872=CARTESIAN_POINT('Ctrl Pts',(0.841256146677281,-0.182055954894471,
-0.324866143747605));
#58873=CARTESIAN_POINT('Ctrl Pts',(0.82785438782568,0.235612790663162,-0.314432181145124));
#58874=CARTESIAN_POINT('Ctrl Pts',(0.619319568298153,0.597745387301998,
-0.303998218542643));
#58875=CARTESIAN_POINT('Ctrl Pts',(0.264805303262618,0.818983775723725,
-0.293564255940163));
#58876=CARTESIAN_POINT('Ctrl Pts',(-0.152126058284342,0.847179992119361,
-0.283130293337682));
#58877=CARTESIAN_POINT('Ctrl Pts',(-0.533199883246888,0.675687915217586,
-0.272696330735201));
#58878=CARTESIAN_POINT('Ctrl Pts',(-0.788593472808699,0.344929855388104,
-0.262262368132721));
#58879=CARTESIAN_POINT('Ctrl Pts',(-0.85810818859447,-0.0671314343578934,
-0.25182840553024));
#58880=CARTESIAN_POINT('Ctrl Pts',(-0.725358696723669,-0.463369173631081,
-0.24139444292776));
#58881=CARTESIAN_POINT('Ctrl Pts',(-0.421635422015108,-0.750386522096553,
-0.230960480325279));
#58882=CARTESIAN_POINT('Ctrl Pts',(-0.0185285562433264,-0.86053055751242,
-0.220526517722799));
#58883=CARTESIAN_POINT('Ctrl Pts',(0.388945352751925,-0.767839757527659,
-0.210092555120318));
#58884=CARTESIAN_POINT('Ctrl Pts',(0.704741798496444,-0.494161306472494,
-0.199658592517837));
#58885=CARTESIAN_POINT('Ctrl Pts',(0.85442277317254,-0.104005573943575,
-0.189224629915356));
#58886=CARTESIAN_POINT('Ctrl Pts',(0.802710635634205,0.310667577083989,
-0.178790667312876));
#58887=CARTESIAN_POINT('Ctrl Pts',(0.561787401645997,0.65210888533253,-0.168356704710395));
#58888=CARTESIAN_POINT('Ctrl Pts',(0.188454746657775,0.839850992854137,
-0.157922742107915));
#58889=CARTESIAN_POINT('Ctrl Pts',(-0.229316478451303,0.82961463096934,
-0.147488779505434));
#58890=CARTESIAN_POINT('Ctrl Pts',(-0.592999937130298,0.623865269466558,
-0.137054816902954));
#58891=CARTESIAN_POINT('Ctrl Pts',(-0.816981345420961,0.270994210833144,
-0.126620854300473));
#58892=CARTESIAN_POINT('Ctrl Pts',(-0.837797728572329,-0.00672831308055416,
-0.119664879232153));
#58893=CARTESIAN_POINT('Ctrl Pts',(-0.814921455736579,-0.139942643537184,
-0.116186891697993));
#58894=CARTESIAN_POINT('Ctrl Pts',(0.596426278379627,-0.572674966240212,
-1.1425283350431));
#58895=CARTESIAN_POINT('Ctrl Pts',(0.690039237300982,-0.475179472305614,
-1.13905034750894));
#58896=CARTESIAN_POINT('Ctrl Pts',(0.828472972546818,-0.233515977058058,
-1.13209437244062));
#58897=CARTESIAN_POINT('Ctrl Pts',(0.840776790045671,0.184255282770983,
-1.12166040983814));
#58898=CARTESIAN_POINT('Ctrl Pts',(0.654924835154713,0.558498232654793,
-1.11122644723566));
#58899=CARTESIAN_POINT('Ctrl Pts',(0.31469001782895,0.801145770682762,-1.10079248463318));
#58900=CARTESIAN_POINT('Ctrl Pts',(-0.0997147185513737,0.854931525810344,
-1.0903585220307));
#58901=CARTESIAN_POINT('Ctrl Pts',(-0.490618537208114,0.707214177068778,
-1.07992455942821));
#58902=CARTESIAN_POINT('Ctrl Pts',(-0.765877541643967,0.392793546079614,
-1.06949059682574));
#58903=CARTESIAN_POINT('Ctrl Pts',(-0.860612728693632,-0.0142090354680717,
-1.05905663422325));
#58904=CARTESIAN_POINT('Ctrl Pts',(-0.752493039839581,-0.417864031829521,
-1.04862267162078));
#58905=CARTESIAN_POINT('Ctrl Pts',(-0.467003853748621,-0.723023724671482,
-1.03818870901829));
#58906=CARTESIAN_POINT('Ctrl Pts',(-0.0714373746764586,-0.857760347616996,
-1.02775474641581));
#58907=CARTESIAN_POINT('Ctrl Pts',(0.340967517012704,-0.790314580308694,
-1.01732078381333));
#58908=CARTESIAN_POINT('Ctrl Pts',(0.673003184192233,-0.53658434549891,
-1.00688682121085));
#58909=CARTESIAN_POINT('Ctrl Pts',(0.846405661890071,-0.15637608121211,
-0.99645285860837));
#58910=CARTESIAN_POINT('Ctrl Pts',(0.820302374851198,0.26069146737326,-0.986018896005891));
#58911=CARTESIAN_POINT('Ctrl Pts',(0.600846103651701,0.616311600756356,
-0.975584933403409));
#58912=CARTESIAN_POINT('Ctrl Pts',(0.239764759257477,0.826661288997697,
-0.96515097080093));
#58913=CARTESIAN_POINT('Ctrl Pts',(-0.177831393616744,0.842159144153302,
-0.954717008198447));
#58914=CARTESIAN_POINT('Ctrl Pts',(-0.553511014901823,0.65915217050663,
-0.944283045595968));
#58915=CARTESIAN_POINT('Ctrl Pts',(-0.798722886956037,0.320776834921653,
-0.933849082993487));
#58916=CARTESIAN_POINT('Ctrl Pts',(-0.855668266116612,-0.0932086165764395,
-0.923415120391007));
#58917=CARTESIAN_POINT('Ctrl Pts',(-0.710924591370782,-0.485223920700338,
-0.912981157788526));
#58918=CARTESIAN_POINT('Ctrl Pts',(-0.39860930742276,-0.762867385533715,
-0.902547195186045));
#58919=CARTESIAN_POINT('Ctrl Pts',(0.0076619373640938,-0.860695836261201,
-0.892113232583565));
#58920=CARTESIAN_POINT('Ctrl Pts',(0.412127191496178,-0.755650187514626,
-0.881679269981083));
#58921=CARTESIAN_POINT('Ctrl Pts',(0.719450192421379,-0.472490686127359,
-0.871245307378604));
#58922=CARTESIAN_POINT('Ctrl Pts',(0.857192019862881,-0.0779606884187777,
-0.860811344776123));
#58923=CARTESIAN_POINT('Ctrl Pts',(0.792885630259222,0.334945376417383,
-0.850377382173642));
#58924=CARTESIAN_POINT('Ctrl Pts',(0.54168864414833,0.668901667403545,-0.839943419571162));
#58925=CARTESIAN_POINT('Ctrl Pts',(0.162810552512241,0.845191547429137,
-0.829509456968682));
#58926=CARTESIAN_POINT('Ctrl Pts',(-0.254443516837955,0.822261834572054,
-0.8190754943662));
#58927=CARTESIAN_POINT('Ctrl Pts',(-0.611722857394327,0.605517277702424,
-0.80864153176372));
#58928=CARTESIAN_POINT('Ctrl Pts',(-0.824813370012824,0.246046606363224,
-0.798207569161239));
#58929=CARTESIAN_POINT('Ctrl Pts',(-0.843487617729615,-0.171419563036438,
-0.787773606558758));
#58930=CARTESIAN_POINT('Ctrl Pts',(-0.663343904812114,-0.54848053001306,
-0.777339643956279));
#58931=CARTESIAN_POINT('Ctrl Pts',(-0.326843797821022,-0.796259480119837,
-0.766905681353797));
#58932=CARTESIAN_POINT('Ctrl Pts',(0.0866964647845083,-0.856352585591155,
-0.756471718751317));
#58933=CARTESIAN_POINT('Ctrl Pts',(0.479801555657399,-0.714595336567154,
-0.746037756148836));
#58934=CARTESIAN_POINT('Ctrl Pts',(0.7598129095271,-0.404401249220066,-0.735603793546356));
#58935=CARTESIAN_POINT('Ctrl Pts',(0.860729218063003,0.00111401410860473,
-0.725169830943875));
#58936=CARTESIAN_POINT('Ctrl Pts',(0.758763558687812,0.406366693839682,
-0.714735868341394));
#58937=CARTESIAN_POINT('Ctrl Pts',(0.477950195835978,0.715834923816333,
-0.704301905738914));
#58938=CARTESIAN_POINT('Ctrl Pts',(0.0844794788944169,0.856574133102626,
-0.693867943136433));
#58939=CARTESIAN_POINT('Ctrl Pts',(-0.328903845364895,0.795410767062509,
-0.683433980533953));
#58940=CARTESIAN_POINT('Ctrl Pts',(-0.664761441438374,0.546761606032795,
-0.673000017931472));
#58941=CARTESIAN_POINT('Ctrl Pts',(-0.843928516730014,0.169235594674005,
-0.662566055328992));
#58942=CARTESIAN_POINT('Ctrl Pts',(-0.82417370734834,-0.248180837234624,
-0.652132092726511));
#58943=CARTESIAN_POINT('Ctrl Pts',(-0.61015340756806,-0.607098712803667,
-0.64169813012403));
#58944=CARTESIAN_POINT('Ctrl Pts',(-0.252314213927473,-0.822917714783772,
-0.63126416752155));
#58945=CARTESIAN_POINT('Ctrl Pts',(0.164997811794668,-0.844767275619598,
-0.620830204919069));
#58946=CARTESIAN_POINT('Ctrl Pts',(0.543418302228559,-0.667497248427149,
-0.610396242316589));
#58947=CARTESIAN_POINT('Ctrl Pts',(0.793749990468483,-0.332891845027883,
-0.599962279714107));
#58948=CARTESIAN_POINT('Ctrl Pts',(0.856987344374013,0.0801792955666448,
-0.589528317111628));
#58949=CARTESIAN_POINT('Ctrl Pts',(0.71822472517211,0.474351422477294,-0.579094354509146));
#58950=CARTESIAN_POINT('Ctrl Pts',(0.410169786635162,0.756714460008828,
-0.568660391906666));
#58951=CARTESIAN_POINT('Ctrl Pts',(0.00543397362123488,0.860712785884739,
-0.558226429304186));
#58952=CARTESIAN_POINT('Ctrl Pts',(-0.400582678056834,0.761833017068439,
-0.547792466701704));
#58953=CARTESIAN_POINT('Ctrl Pts',(-0.712178226872656,0.483382044580997,
-0.537358504099225));
#58954=CARTESIAN_POINT('Ctrl Pts',(-0.855906672842221,0.0909933801929833,
-0.526924541496744));
#58955=CARTESIAN_POINT('Ctrl Pts',(-0.797889870143162,-0.322843279282244,
-0.516490578894263));
#58956=CARTESIAN_POINT('Ctrl Pts',(-0.551802924553791,-0.660582742969169,
-0.506056616291783));
#58957=CARTESIAN_POINT('Ctrl Pts',(-0.175650842469447,-0.842616644384952,
-0.495622653689301));
#58958=CARTESIAN_POINT('Ctrl Pts',(0.241903794376119,-0.826037881771305,
-0.485188691086821));
#58959=CARTESIAN_POINT('Ctrl Pts',(0.602439432890687,-0.61475422532353,
-0.47475472848434));
#58960=CARTESIAN_POINT('Ctrl Pts',(0.820974433890951,-0.2585672190209,-0.46432076588186));
#58961=CARTESIAN_POINT('Ctrl Pts',(0.845998043321078,0.158566511444712,
-0.453886803279379));
#58962=CARTESIAN_POINT('Ctrl Pts',(0.671611961205852,0.53832462457136,-0.443452840676899));
#58963=CARTESIAN_POINT('Ctrl Pts',(0.338920626402068,0.791194563210737,
-0.433018878074418));
#58964=CARTESIAN_POINT('Ctrl Pts',(-0.0736574860403522,0.85757250574206,
-0.422584915471938));
#58965=CARTESIAN_POINT('Ctrl Pts',(-0.468873836611143,0.72181254713152,
-0.412150952869457));
#58966=CARTESIAN_POINT('Ctrl Pts',(-0.753572216284693,0.41591458582155,
-0.401716990266977));
#58967=CARTESIAN_POINT('Ctrl Pts',(-0.860646540683597,0.0119816468658661,
-0.391283027664496));
#58968=CARTESIAN_POINT('Ctrl Pts',(-0.764858385013229,-0.394775478894489,
-0.380849065062015));
#58969=CARTESIAN_POINT('Ctrl Pts',(-0.488785917995028,-0.70848031321364,
-0.370415102459535));
#58970=CARTESIAN_POINT('Ctrl Pts',(-0.0975020153382415,-0.855189677720726,
-0.359981139857054));
#58971=CARTESIAN_POINT('Ctrl Pts',(0.316764028941221,-0.800322796004492,
-0.349547177254573));
#58972=CARTESIAN_POINT('Ctrl Pts',(0.656365813791203,-0.556812307990146,
-0.339113214652093));
#58973=CARTESIAN_POINT('Ctrl Pts',(0.841256006403051,-0.182055924541145,
-0.328679252049612));
#58974=CARTESIAN_POINT('Ctrl Pts',(0.827854249784971,0.23561275138288,-0.318245289447132));
#58975=CARTESIAN_POINT('Ctrl Pts',(0.619319465031675,0.597745287618043,
-0.307811326844651));
#58976=CARTESIAN_POINT('Ctrl Pts',(0.264805259104926,0.818983639189149,
-0.297377364242171));
#58977=CARTESIAN_POINT('Ctrl Pts',(-0.152126032912431,0.847179850805376,
-0.286943401639689));
#58978=CARTESIAN_POINT('Ctrl Pts',(-0.533199794350217,0.675687802651953,
-0.276509439037209));
#58979=CARTESIAN_POINT('Ctrl Pts',(-0.788593341292993,0.344929797673643,
-0.266075476434728));
#58980=CARTESIAN_POINT('Ctrl Pts',(-0.858108045553684,-0.0671314227721541,
-0.255641513832248));
#58981=CARTESIAN_POINT('Ctrl Pts',(-0.72535857568816,-0.463369097137432,
-0.245207551229767));
#58982=CARTESIAN_POINT('Ctrl Pts',(-0.421635351879131,-0.750386395459336,
-0.234773588627287));
#58983=CARTESIAN_POINT('Ctrl Pts',(-0.0185285528209956,-0.860530417001193,
-0.224339626024806));
#58984=CARTESIAN_POINT('Ctrl Pts',(0.388945287243328,-0.76783962364223,
-0.213905663422326));
#58985=CARTESIAN_POINT('Ctrl Pts',(0.704741682270798,-0.494161235578589,
-0.203471700819845));
#58986=CARTESIAN_POINT('Ctrl Pts',(0.854422628174538,-0.104005533986035,
-0.193037738217364));
#58987=CARTESIAN_POINT('Ctrl Pts',(0.802710506756149,0.310667480825697,
-0.182603775614884));
#58988=CARTESIAN_POINT('Ctrl Pts',(0.561787298202008,0.652108863993638,
-0.172169813012403));
#58989=CARTESIAN_POINT('Ctrl Pts',(0.188454734446511,0.839850680936056,
-0.161735850409922));
#58990=CARTESIAN_POINT('Ctrl Pts',(-0.22931647807991,0.829614831389831,
-0.151301887807442));
#58991=CARTESIAN_POINT('Ctrl Pts',(-0.59299976270307,0.623864489566942,
-0.140867925204961));
#58992=CARTESIAN_POINT('Ctrl Pts',(-0.81698137021996,0.270995606044551,
-0.130433962602481));
#58993=CARTESIAN_POINT('Ctrl Pts',(-0.837797337716894,-0.00673058913074182,
-0.12347798753416));
#58994=CARTESIAN_POINT('Ctrl Pts',(-0.814921455736579,-0.139942643537184,
-0.12));
#58995=CARTESIAN_POINT('Ctrl Pts',(-0.676565692095429,0.457932546695683,
-0.12));
#58996=CARTESIAN_POINT('Ctrl Pts',(-0.715290549838907,0.406460878340116,
-0.12));
#58997=CARTESIAN_POINT('Ctrl Pts',(-0.761722039381193,0.328281076047502,
-0.12));
#58998=CARTESIAN_POINT('Ctrl Pts',(-0.809780868705113,0.169044693082709,
-0.12));
#58999=CARTESIAN_POINT('Ctrl Pts',(-0.820456584566055,0.110526708837243,
-0.12));
#59000=CARTESIAN_POINT('Ctrl Pts',(-0.829018965506486,-0.0125105404198994,
-0.12));
#59001=CARTESIAN_POINT('Ctrl Pts',(-0.82576831737714,-0.0767786210857246,
-0.12));
#59002=CARTESIAN_POINT('Ctrl Pts',(-0.814921455736578,-0.139942643537185,
-0.12));
#59003=CARTESIAN_POINT('Origin',(0.,0.,0.0794349077448279));
#59004=CARTESIAN_POINT('',(-1.045,-1.27975590510898E-16,-6.93889390390723E-17));
#59005=CARTESIAN_POINT('Origin',(0.,0.,0.));
#59006=CARTESIAN_POINT('',(-1.1,-9.25861368525747E-17,0.0317542648054295));
#59007=CARTESIAN_POINT('',(-1.18258529610859,-1.44824929759811E-16,0.0794349077448279));
#59008=CARTESIAN_POINT('',(-1.1,0.635085296108588,0.130002302030174));
#59009=CARTESIAN_POINT('Ctrl Pts',(-1.1,0.635085296108588,0.130002302030174));
#59010=CARTESIAN_POINT('Ctrl Pts',(-1.1,0.294744111674235,0.0317542648054296));
#59011=CARTESIAN_POINT('Ctrl Pts',(-1.1,-5.04611257989404E-17,0.0317542648054295));
#59012=CARTESIAN_POINT('',(7.77755175064932E-17,1.27017059221718,0.130002302030174));
#59013=CARTESIAN_POINT('Ctrl Pts',(7.77755175064932E-17,1.27017059221718,
0.130002302030174));
#59014=CARTESIAN_POINT('Ctrl Pts',(-0.55,0.952627944162882,-0.0533310313031589));
#59015=CARTESIAN_POINT('Ctrl Pts',(-1.1,0.635085296108588,0.130002302030174));
#59016=CARTESIAN_POINT('',(1.1,0.635085296108588,0.130002302030174));
#59017=CARTESIAN_POINT('Ctrl Pts',(1.1,0.635085296108588,0.130002302030174));
#59018=CARTESIAN_POINT('Ctrl Pts',(0.55,0.952627944162882,-0.0533310313031591));
#59019=CARTESIAN_POINT('Ctrl Pts',(7.77755175064932E-17,1.27017059221718,
0.130002302030174));
#59020=CARTESIAN_POINT('',(1.1,-0.635085296108589,0.130002302030174));
#59021=CARTESIAN_POINT('Ctrl Pts',(1.1,-0.635085296108589,0.130002302030174));
#59022=CARTESIAN_POINT('Ctrl Pts',(1.1,-3.33066907387547E-16,-0.0533310313031591));
#59023=CARTESIAN_POINT('Ctrl Pts',(1.1,0.635085296108588,0.130002302030174));
#59024=CARTESIAN_POINT('',(-2.3332655251948E-16,-1.27017059221718,0.130002302030174));
#59025=CARTESIAN_POINT('Ctrl Pts',(-2.3332655251948E-16,-1.27017059221718,
0.130002302030174));
#59026=CARTESIAN_POINT('Ctrl Pts',(0.55,-0.952627944162883,-0.0533310313031587));
#59027=CARTESIAN_POINT('Ctrl Pts',(1.1,-0.635085296108589,0.130002302030174));
#59028=CARTESIAN_POINT('',(-1.1,-0.635085296108588,0.130002302030174));
#59029=CARTESIAN_POINT('Ctrl Pts',(-1.1,-0.635085296108588,0.130002302030174));
#59030=CARTESIAN_POINT('Ctrl Pts',(-0.55,-0.952627944162882,-0.0533310313031589));
#59031=CARTESIAN_POINT('Ctrl Pts',(-2.3332655251948E-16,-1.27017059221718,
0.130002302030174));
#59032=CARTESIAN_POINT('Ctrl Pts',(-1.1,-5.04611257989404E-17,0.0317542648054295));
#59033=CARTESIAN_POINT('Ctrl Pts',(-1.1,-0.294744111674235,0.0317542648054295));
#59034=CARTESIAN_POINT('Ctrl Pts',(-1.1,-0.635085296108588,0.130002302030174));
#59035=CARTESIAN_POINT('Origin',(-2.3332655251948E-16,-1.27017059221718,
0.));
#59036=CARTESIAN_POINT('',(1.1,-0.635085296108589,0.669997697969826));
#59037=CARTESIAN_POINT('',(1.1,-0.635085296108589,0.));
#59038=CARTESIAN_POINT('',(-2.3332655251948E-16,-1.27017059221718,0.669997697969826));
#59039=CARTESIAN_POINT('Ctrl Pts',(1.1,-0.635085296108589,0.669997697969826));
#59040=CARTESIAN_POINT('Ctrl Pts',(0.55,-0.952627944162883,0.853331031303159));
#59041=CARTESIAN_POINT('Ctrl Pts',(-2.3332655251948E-16,-1.27017059221718,
0.669997697969826));
#59042=CARTESIAN_POINT('',(-2.3332655251948E-16,-1.27017059221718,0.));
#59043=CARTESIAN_POINT('Origin',(1.1,-0.635085296108589,0.));
#59044=CARTESIAN_POINT('',(1.1,0.635085296108588,0.669997697969826));
#59045=CARTESIAN_POINT('',(1.1,0.635085296108588,0.));
#59046=CARTESIAN_POINT('Ctrl Pts',(1.1,0.635085296108588,0.669997697969826));
#59047=CARTESIAN_POINT('Ctrl Pts',(1.1,-3.33066907387547E-16,0.853331031303159));
#59048=CARTESIAN_POINT('Ctrl Pts',(1.1,-0.635085296108589,0.669997697969826));
#59049=CARTESIAN_POINT('Origin',(1.1,0.635085296108588,0.));
#59050=CARTESIAN_POINT('',(7.77755175064932E-17,1.27017059221718,0.669997697969826));
#59051=CARTESIAN_POINT('',(7.77755175064932E-17,1.27017059221718,0.));
#59052=CARTESIAN_POINT('Ctrl Pts',(7.77755175064932E-17,1.27017059221718,
0.669997697969826));
#59053=CARTESIAN_POINT('Ctrl Pts',(0.55,0.952627944162882,0.853331031303159));
#59054=CARTESIAN_POINT('Ctrl Pts',(1.1,0.635085296108588,0.669997697969826));
#59055=CARTESIAN_POINT('Origin',(0.,0.,0.720565092255172));
#59056=CARTESIAN_POINT('',(-1.1,0.635085296108588,0.669997697969826));
#59057=CARTESIAN_POINT('Ctrl Pts',(-1.1,0.635085296108588,0.669997697969826));
#59058=CARTESIAN_POINT('Ctrl Pts',(-0.55,0.952627944162882,0.853331031303159));
#59059=CARTESIAN_POINT('Ctrl Pts',(7.77755175064932E-17,1.27017059221718,
0.669997697969826));
#59060=CARTESIAN_POINT('',(-1.1,-1.43047262651515E-16,0.768245735194571));
#59061=CARTESIAN_POINT('Ctrl Pts',(-1.1,-1.51383377396821E-16,0.768245735194571));
#59062=CARTESIAN_POINT('Ctrl Pts',(-1.1,0.294744111674235,0.768245735194571));
#59063=CARTESIAN_POINT('Ctrl Pts',(-1.1,0.635085296108588,0.669997697969826));
#59064=CARTESIAN_POINT('',(-1.045,-1.27975590510898E-16,0.8));
#59065=CARTESIAN_POINT('',(-1.18258529610859,-1.44824929759811E-16,0.720565092255172));
#59066=CARTESIAN_POINT('Origin',(0.,0.,0.8));
#59067=CARTESIAN_POINT('',(-1.1,-0.635085296108588,0.669997697969826));
#59068=CARTESIAN_POINT('Ctrl Pts',(-1.1,-0.635085296108588,0.669997697969826));
#59069=CARTESIAN_POINT('Ctrl Pts',(-1.1,-0.294744111674235,0.76824573519457));
#59070=CARTESIAN_POINT('Ctrl Pts',(-1.1,-1.51383377396821E-16,0.768245735194571));
#59071=CARTESIAN_POINT('Ctrl Pts',(-2.3332655251948E-16,-1.27017059221718,
0.669997697969826));
#59072=CARTESIAN_POINT('Ctrl Pts',(-0.55,-0.952627944162883,0.853331031303159));
#59073=CARTESIAN_POINT('Ctrl Pts',(-1.1,-0.635085296108588,0.669997697969826));
#59074=CARTESIAN_POINT('Origin',(7.77755175064932E-17,1.27017059221718,
0.));
#59075=CARTESIAN_POINT('',(-1.1,0.635085296108588,0.));
#59076=CARTESIAN_POINT('Origin',(0.,0.,0.8));
#59077=CARTESIAN_POINT('Origin',(0.,0.,0.8));
#59078=CARTESIAN_POINT('',(-0.4,4.89858719658941E-17,0.8));
#59079=CARTESIAN_POINT('Origin',(0.,0.,0.8));
#59080=CARTESIAN_POINT('Origin',(0.,0.,0.));
#59081=CARTESIAN_POINT('',(-0.7431,9.10035036446398E-17,0.));
#59082=CARTESIAN_POINT('Origin',(0.,0.,0.));
#59083=CARTESIAN_POINT('Origin',(0.,0.,0.));
#59084=CARTESIAN_POINT('',(-0.4,-4.89858719658941E-17,0.));
#59085=CARTESIAN_POINT('Origin',(0.,0.,0.));
#59086=CARTESIAN_POINT('Origin',(-1.1,-0.635085296108589,0.));
#59087=CARTESIAN_POINT('',(-1.1,-0.635085296108589,0.));
#59088=CARTESIAN_POINT('Origin',(-1.1,0.635085296108588,0.));
#59089=CARTESIAN_POINT('Origin',(0.,0.,0.0765832901469392));
#59090=CARTESIAN_POINT('',(-0.4,-4.89858719658941E-17,-1.2));
#59091=CARTESIAN_POINT('',(-0.4,-4.89858719658941E-17,0.0765832901469392));
#59092=CARTESIAN_POINT('Origin',(0.,0.,-1.2));
#59093=CARTESIAN_POINT('Origin',(0.,0.,0.0765832901469392));
#59094=CARTESIAN_POINT('',(-0.4,-4.89858719658941E-17,1.35316658029388));
#59095=CARTESIAN_POINT('Origin',(0.,0.,1.35316658029388));
#59096=CARTESIAN_POINT('',(-0.4,-4.89858719658941E-17,0.0765832901469392));
#59097=CARTESIAN_POINT('Origin',(0.7531,0.,-1.2));
#59098=CARTESIAN_POINT('',(-0.7531,-9.22281504437872E-17,-1.2));
#59099=CARTESIAN_POINT('Origin',(0.,0.,-1.2));
#59100=CARTESIAN_POINT('Origin',(0.,0.,-1.16));
#59101=CARTESIAN_POINT('',(-0.7931,-9.71267376403766E-17,-1.16));
#59102=CARTESIAN_POINT('Origin',(0.7431,0.,-0.12));
#59103=CARTESIAN_POINT('',(-0.7431,-9.10035036446398E-17,-0.12));
#59104=CARTESIAN_POINT('Origin',(0.,0.,-0.12));
#59105=CARTESIAN_POINT('Origin',(0.,0.,-0.0349999999999999));
#59106=CARTESIAN_POINT('',(-0.7431,-9.10035036446398E-17,-0.0349999999999999));
#59107=CARTESIAN_POINT('Origin',(0.,0.,2.17));
#59108=CARTESIAN_POINT('',(-0.74,-9.06238631369041E-17,2.2));
#59109=CARTESIAN_POINT('Origin',(0.,0.,2.2));
#59110=CARTESIAN_POINT('',(-0.77,-9.42978035343462E-17,2.17));
#59111=CARTESIAN_POINT('Origin',(0.58,0.,2.2));
#59112=CARTESIAN_POINT('',(-0.58,-7.10295143505465E-17,2.2));
#59113=CARTESIAN_POINT('Origin',(0.,0.,2.2));
#59114=CARTESIAN_POINT('Origin',(0.,0.,1.77658329014694));
#59115=CARTESIAN_POINT('',(-0.49,-6.00076931582203E-17,1.77658329014694));
#59116=CARTESIAN_POINT('',(7.34666790032092,0.,2.6));
#59117=CARTESIAN_POINT('',(7.34666790032092,0.,2.6));
#59118=CARTESIAN_POINT('',(6.65,0.,1.44918799183103E-15));
#59119=CARTESIAN_POINT('',(0.,0.,0.));
#59120=CARTESIAN_POINT('',(0.,0.,0.));
#59121=CARTESIAN_POINT('',(0.,0.,0.));
#59122=CARTESIAN_POINT('',(0.,0.,0.));
#59123=CARTESIAN_POINT('',(11.36,-3.10130032290503E-266,2.52242671194836E-15));
#59124=CARTESIAN_POINT('',(12.35,0.,2.74225087082414E-15));
#59125=CARTESIAN_POINT('',(11.225,0.,2.49245069028348E-15));
#59126=CARTESIAN_POINT('',(11.225,0.,2.49245069028348E-15));
#59127=CARTESIAN_POINT('',(0.539999999999999,0.,6.));
#59128=CARTESIAN_POINT('',(-3.9,6.8,-8.65973959207622E-16));
#59129=CARTESIAN_POINT('',(4.,0.,5.2));
#59130=CARTESIAN_POINT('',(-1.2,6.8,-2.66453525910038E-16));
#59131=CARTESIAN_POINT('',(0.,0.,0.));
#59132=CARTESIAN_POINT('',(0.,0.,0.));
#59133=CARTESIAN_POINT('',(0.,0.,0.));
#59134=CARTESIAN_POINT('',(0.,0.,0.));
#59135=CARTESIAN_POINT('',(0.,0.,0.));
#59136=CARTESIAN_POINT('',(7.18367857374021,1.671247785185,1.99171555210934));
#59137=CARTESIAN_POINT('',(6.77097511132978,2.56050015783174,0.451485261934021));
#59138=CARTESIAN_POINT('',(6.30166604983954,2.25166604983954,-1.3));
#59139=CARTESIAN_POINT('',(5.99534631493002,0.889252372646739,-2.44320081404336));
#59140=CARTESIAN_POINT('',(5.99534631493002,-0.889252372646738,-2.44320081404336));
#59141=CARTESIAN_POINT('',(6.30166604983954,-2.25166604983954,-1.3));
#59142=CARTESIAN_POINT('',(6.77097511132977,-2.56050015783174,0.45148526193402));
#59143=CARTESIAN_POINT('',(7.18367857374021,-1.671247785185,1.99171555210934));
#59144=CARTESIAN_POINT('',(7.18367857374021,1.671247785185,1.99171555210934));
#59145=CARTESIAN_POINT('',(6.77097511132977,2.56050015783174,0.451485261934021));
#59146=CARTESIAN_POINT('',(6.30166604983954,2.25166604983954,-1.3));
#59147=CARTESIAN_POINT('',(5.99534631493002,0.889252372646739,-2.44320081404336));
#59148=CARTESIAN_POINT('',(5.99534631493002,-0.889252372646739,-2.44320081404336));
#59149=CARTESIAN_POINT('',(6.30166604983954,-2.25166604983954,-1.3));
#59150=CARTESIAN_POINT('',(6.77097511132977,-2.56050015783174,0.451485261934019));
#59151=CARTESIAN_POINT('',(7.18367857374021,-1.671247785185,1.99171555210935));
#59152=CARTESIAN_POINT('',(-4.125,-3.08148791101945E-33,-9.15933995315754E-16));
#59153=CARTESIAN_POINT('',(-4.125,0.,-9.15933995315754E-16));
#59154=CARTESIAN_POINT('',(-4.135,-6.88627004953319E-282,-9.18154441365004E-16));
#59155=CARTESIAN_POINT('',(0.539999999999999,5.19615242270663,3.));
#59156=CARTESIAN_POINT('',(0.540000000000001,5.19615242270663,-3.));
#59157=CARTESIAN_POINT('',(0.540000000000001,7.34788079488412E-16,-6.));
#59158=CARTESIAN_POINT('',(0.540000000000001,-5.19615242270663,-3.));
#59159=CARTESIAN_POINT('',(0.539999999999999,-5.19615242270663,3.));
#59160=CARTESIAN_POINT('',(-1.2,-6.8,-2.66453525910038E-16));
#59161=UNCERTAINTY_MEASURE_WITH_UNIT(LENGTH_MEASURE(0.001),#59205,
'DISTANCE_ACCURACY_VALUE',
'Maximum model space distance between geometric entities at asserted c
onnectivities');
#59162=UNCERTAINTY_MEASURE_WITH_UNIT(LENGTH_MEASURE(0.001),#59205,
'DISTANCE_ACCURACY_VALUE',
'Maximum model space distance between geometric entities at asserted c
onnectivities');
#59163=UNCERTAINTY_MEASURE_WITH_UNIT(LENGTH_MEASURE(0.001),#59205,
'DISTANCE_ACCURACY_VALUE',
'Maximum model space distance between geometric entities at asserted c
onnectivities');
#59164=UNCERTAINTY_MEASURE_WITH_UNIT(LENGTH_MEASURE(0.001),#59205,
'DISTANCE_ACCURACY_VALUE',
'Maximum model space distance between geometric entities at asserted c
onnectivities');
#59165=UNCERTAINTY_MEASURE_WITH_UNIT(LENGTH_MEASURE(0.001),#59205,
'DISTANCE_ACCURACY_VALUE',
'Maximum model space distance between geometric entities at asserted c
onnectivities');
#59166=UNCERTAINTY_MEASURE_WITH_UNIT(LENGTH_MEASURE(0.001),#59205,
'DISTANCE_ACCURACY_VALUE',
'Maximum model space distance between geometric entities at asserted c
onnectivities');
#59167=UNCERTAINTY_MEASURE_WITH_UNIT(LENGTH_MEASURE(0.001),#59205,
'DISTANCE_ACCURACY_VALUE',
'Maximum model space distance between geometric entities at asserted c
onnectivities');
#59168=UNCERTAINTY_MEASURE_WITH_UNIT(LENGTH_MEASURE(0.001),#59205,
'DISTANCE_ACCURACY_VALUE',
'Maximum model space distance between geometric entities at asserted c
onnectivities');
#59169=UNCERTAINTY_MEASURE_WITH_UNIT(LENGTH_MEASURE(0.001),#59205,
'DISTANCE_ACCURACY_VALUE',
'Maximum model space distance between geometric entities at asserted c
onnectivities');
#59170=UNCERTAINTY_MEASURE_WITH_UNIT(LENGTH_MEASURE(0.001),#59205,
'DISTANCE_ACCURACY_VALUE',
'Maximum model space distance between geometric entities at asserted c
onnectivities');
#59171=UNCERTAINTY_MEASURE_WITH_UNIT(LENGTH_MEASURE(0.001),#59205,
'DISTANCE_ACCURACY_VALUE',
'Maximum model space distance between geometric entities at asserted c
onnectivities');
#59172=UNCERTAINTY_MEASURE_WITH_UNIT(LENGTH_MEASURE(0.001),#59205,
'DISTANCE_ACCURACY_VALUE',
'Maximum model space distance between geometric entities at asserted c
onnectivities');
#59173=UNCERTAINTY_MEASURE_WITH_UNIT(LENGTH_MEASURE(0.001),#59205,
'DISTANCE_ACCURACY_VALUE',
'Maximum model space distance between geometric entities at asserted c
onnectivities');
#59174=UNCERTAINTY_MEASURE_WITH_UNIT(LENGTH_MEASURE(0.001),#59205,
'DISTANCE_ACCURACY_VALUE',
'Maximum model space distance between geometric entities at asserted c
onnectivities');
#59175=UNCERTAINTY_MEASURE_WITH_UNIT(LENGTH_MEASURE(0.001),#59205,
'DISTANCE_ACCURACY_VALUE',
'Maximum model space distance between geometric entities at asserted c
onnectivities');
#59176=UNCERTAINTY_MEASURE_WITH_UNIT(LENGTH_MEASURE(0.001),#59205,
'DISTANCE_ACCURACY_VALUE',
'Maximum model space distance between geometric entities at asserted c
onnectivities');
#59177=UNCERTAINTY_MEASURE_WITH_UNIT(LENGTH_MEASURE(0.001),#59205,
'DISTANCE_ACCURACY_VALUE',
'Maximum model space distance between geometric entities at asserted c
onnectivities');
#59178=UNCERTAINTY_MEASURE_WITH_UNIT(LENGTH_MEASURE(0.001),#59205,
'DISTANCE_ACCURACY_VALUE',
'Maximum model space distance between geometric entities at asserted c
onnectivities');
#59179=UNCERTAINTY_MEASURE_WITH_UNIT(LENGTH_MEASURE(0.001),#59205,
'DISTANCE_ACCURACY_VALUE',
'Maximum model space distance between geometric entities at asserted c
onnectivities');
#59180=UNCERTAINTY_MEASURE_WITH_UNIT(LENGTH_MEASURE(0.001),#59205,
'DISTANCE_ACCURACY_VALUE',
'Maximum model space distance between geometric entities at asserted c
onnectivities');
#59181=UNCERTAINTY_MEASURE_WITH_UNIT(LENGTH_MEASURE(0.001),#59205,
'DISTANCE_ACCURACY_VALUE',
'Maximum model space distance between geometric entities at asserted c
onnectivities');
#59182=UNCERTAINTY_MEASURE_WITH_UNIT(LENGTH_MEASURE(0.001),#59205,
'DISTANCE_ACCURACY_VALUE',
'Maximum model space distance between geometric entities at asserted c
onnectivities');
#59183=(
GEOMETRIC_REPRESENTATION_CONTEXT(3)
GLOBAL_UNCERTAINTY_ASSIGNED_CONTEXT((#59161))
GLOBAL_UNIT_ASSIGNED_CONTEXT((#59205,#59207,#59208))
REPRESENTATION_CONTEXT('','3D')
);
#59184=(
GEOMETRIC_REPRESENTATION_CONTEXT(3)
GLOBAL_UNCERTAINTY_ASSIGNED_CONTEXT((#59162))
GLOBAL_UNIT_ASSIGNED_CONTEXT((#59205,#59207,#59208))
REPRESENTATION_CONTEXT('','3D')
);
#59185=(
GEOMETRIC_REPRESENTATION_CONTEXT(3)
GLOBAL_UNCERTAINTY_ASSIGNED_CONTEXT((#59163))
GLOBAL_UNIT_ASSIGNED_CONTEXT((#59205,#59207,#59208))
REPRESENTATION_CONTEXT('','3D')
);
#59186=(
GEOMETRIC_REPRESENTATION_CONTEXT(3)
GLOBAL_UNCERTAINTY_ASSIGNED_CONTEXT((#59164))
GLOBAL_UNIT_ASSIGNED_CONTEXT((#59205,#59207,#59208))
REPRESENTATION_CONTEXT('','3D')
);
#59187=(
GEOMETRIC_REPRESENTATION_CONTEXT(3)
GLOBAL_UNCERTAINTY_ASSIGNED_CONTEXT((#59165))
GLOBAL_UNIT_ASSIGNED_CONTEXT((#59205,#59207,#59208))
REPRESENTATION_CONTEXT('','3D')
);
#59188=(
GEOMETRIC_REPRESENTATION_CONTEXT(3)
GLOBAL_UNCERTAINTY_ASSIGNED_CONTEXT((#59166))
GLOBAL_UNIT_ASSIGNED_CONTEXT((#59205,#59207,#59208))
REPRESENTATION_CONTEXT('','3D')
);
#59189=(
GEOMETRIC_REPRESENTATION_CONTEXT(3)
GLOBAL_UNCERTAINTY_ASSIGNED_CONTEXT((#59167))
GLOBAL_UNIT_ASSIGNED_CONTEXT((#59205,#59207,#59208))
REPRESENTATION_CONTEXT('','3D')
);
#59190=(
GEOMETRIC_REPRESENTATION_CONTEXT(3)
GLOBAL_UNCERTAINTY_ASSIGNED_CONTEXT((#59168))
GLOBAL_UNIT_ASSIGNED_CONTEXT((#59205,#59207,#59208))
REPRESENTATION_CONTEXT('','3D')
);
#59191=(
GEOMETRIC_REPRESENTATION_CONTEXT(3)
GLOBAL_UNCERTAINTY_ASSIGNED_CONTEXT((#59169))
GLOBAL_UNIT_ASSIGNED_CONTEXT((#59205,#59207,#59208))
REPRESENTATION_CONTEXT('','3D')
);
#59192=(
GEOMETRIC_REPRESENTATION_CONTEXT(3)
GLOBAL_UNCERTAINTY_ASSIGNED_CONTEXT((#59170))
GLOBAL_UNIT_ASSIGNED_CONTEXT((#59205,#59207,#59208))
REPRESENTATION_CONTEXT('','3D')
);
#59193=(
GEOMETRIC_REPRESENTATION_CONTEXT(3)
GLOBAL_UNCERTAINTY_ASSIGNED_CONTEXT((#59171))
GLOBAL_UNIT_ASSIGNED_CONTEXT((#59205,#59207,#59208))
REPRESENTATION_CONTEXT('','3D')
);
#59194=(
GEOMETRIC_REPRESENTATION_CONTEXT(3)
GLOBAL_UNCERTAINTY_ASSIGNED_CONTEXT((#59172))
GLOBAL_UNIT_ASSIGNED_CONTEXT((#59205,#59207,#59208))
REPRESENTATION_CONTEXT('','3D')
);
#59195=(
GEOMETRIC_REPRESENTATION_CONTEXT(3)
GLOBAL_UNCERTAINTY_ASSIGNED_CONTEXT((#59173))
GLOBAL_UNIT_ASSIGNED_CONTEXT((#59205,#59207,#59208))
REPRESENTATION_CONTEXT('','3D')
);
#59196=(
GEOMETRIC_REPRESENTATION_CONTEXT(3)
GLOBAL_UNCERTAINTY_ASSIGNED_CONTEXT((#59174))
GLOBAL_UNIT_ASSIGNED_CONTEXT((#59205,#59207,#59208))
REPRESENTATION_CONTEXT('','3D')
);
#59197=(
GEOMETRIC_REPRESENTATION_CONTEXT(3)
GLOBAL_UNCERTAINTY_ASSIGNED_CONTEXT((#59175))
GLOBAL_UNIT_ASSIGNED_CONTEXT((#59205,#59207,#59208))
REPRESENTATION_CONTEXT('','3D')
);
#59198=(
GEOMETRIC_REPRESENTATION_CONTEXT(3)
GLOBAL_UNCERTAINTY_ASSIGNED_CONTEXT((#59176))
GLOBAL_UNIT_ASSIGNED_CONTEXT((#59205,#59207,#59208))
REPRESENTATION_CONTEXT('','3D')
);
#59199=(
GEOMETRIC_REPRESENTATION_CONTEXT(3)
GLOBAL_UNCERTAINTY_ASSIGNED_CONTEXT((#59177))
GLOBAL_UNIT_ASSIGNED_CONTEXT((#59205,#59207,#59208))
REPRESENTATION_CONTEXT('','3D')
);
#59200=(
GEOMETRIC_REPRESENTATION_CONTEXT(3)
GLOBAL_UNCERTAINTY_ASSIGNED_CONTEXT((#59178))
GLOBAL_UNIT_ASSIGNED_CONTEXT((#59205,#59207,#59208))
REPRESENTATION_CONTEXT('','3D')
);
#59201=(
GEOMETRIC_REPRESENTATION_CONTEXT(3)
GLOBAL_UNCERTAINTY_ASSIGNED_CONTEXT((#59179))
GLOBAL_UNIT_ASSIGNED_CONTEXT((#59205,#59207,#59208))
REPRESENTATION_CONTEXT('','3D')
);
#59202=(
GEOMETRIC_REPRESENTATION_CONTEXT(3)
GLOBAL_UNCERTAINTY_ASSIGNED_CONTEXT((#59180))
GLOBAL_UNIT_ASSIGNED_CONTEXT((#59205,#59207,#59208))
REPRESENTATION_CONTEXT('','3D')
);
#59203=(
GEOMETRIC_REPRESENTATION_CONTEXT(3)
GLOBAL_UNCERTAINTY_ASSIGNED_CONTEXT((#59181))
GLOBAL_UNIT_ASSIGNED_CONTEXT((#59205,#59207,#59208))
REPRESENTATION_CONTEXT('','3D')
);
#59204=(
GEOMETRIC_REPRESENTATION_CONTEXT(3)
GLOBAL_UNCERTAINTY_ASSIGNED_CONTEXT((#59182))
GLOBAL_UNIT_ASSIGNED_CONTEXT((#59205,#59207,#59208))
REPRESENTATION_CONTEXT('','3D')
);
#59205=(
LENGTH_UNIT()
NAMED_UNIT(*)
SI_UNIT(.CENTI.,.METRE.)
);
#59206=(
LENGTH_UNIT()
NAMED_UNIT(*)
SI_UNIT($,.METRE.)
);
#59207=(
NAMED_UNIT(*)
PLANE_ANGLE_UNIT()
SI_UNIT($,.RADIAN.)
);
#59208=(
NAMED_UNIT(*)
SI_UNIT($,.STERADIAN.)
SOLID_ANGLE_UNIT()
);
#59209=SHAPE_DEFINITION_REPRESENTATION(#59230,#59296);
#59210=SHAPE_DEFINITION_REPRESENTATION(#59231,#59297);
#59211=SHAPE_DEFINITION_REPRESENTATION(#59232,#59298);
#59212=SHAPE_DEFINITION_REPRESENTATION(#59233,#59299);
#59213=SHAPE_DEFINITION_REPRESENTATION(#59234,#59300);
#59214=SHAPE_DEFINITION_REPRESENTATION(#59235,#59301);
#59215=SHAPE_DEFINITION_REPRESENTATION(#59236,#59302);
#59216=SHAPE_DEFINITION_REPRESENTATION(#59237,#59303);
#59217=SHAPE_DEFINITION_REPRESENTATION(#59238,#59304);
#59218=SHAPE_DEFINITION_REPRESENTATION(#59239,#59305);
#59219=SHAPE_DEFINITION_REPRESENTATION(#59240,#59306);
#59220=SHAPE_DEFINITION_REPRESENTATION(#59241,#59307);
#59221=SHAPE_DEFINITION_REPRESENTATION(#59242,#59308);
#59222=SHAPE_DEFINITION_REPRESENTATION(#59243,#59309);
#59223=SHAPE_DEFINITION_REPRESENTATION(#59244,#59310);
#59224=SHAPE_DEFINITION_REPRESENTATION(#59245,#59311);
#59225=SHAPE_DEFINITION_REPRESENTATION(#59246,#59312);
#59226=SHAPE_DEFINITION_REPRESENTATION(#59247,#59313);
#59227=SHAPE_DEFINITION_REPRESENTATION(#59248,#59314);
#59228=SHAPE_DEFINITION_REPRESENTATION(#59249,#59315);
#59229=SHAPE_DEFINITION_REPRESENTATION(#59250,#59316);
#59230=PRODUCT_DEFINITION_SHAPE('',$,#59318);
#59231=PRODUCT_DEFINITION_SHAPE('',$,#59319);
#59232=PRODUCT_DEFINITION_SHAPE('',$,#59320);
#59233=PRODUCT_DEFINITION_SHAPE('',$,#59321);
#59234=PRODUCT_DEFINITION_SHAPE('',$,#59322);
#59235=PRODUCT_DEFINITION_SHAPE('',$,#59323);
#59236=PRODUCT_DEFINITION_SHAPE('',$,#59324);
#59237=PRODUCT_DEFINITION_SHAPE('',$,#59325);
#59238=PRODUCT_DEFINITION_SHAPE('',$,#59326);
#59239=PRODUCT_DEFINITION_SHAPE('',$,#59327);
#59240=PRODUCT_DEFINITION_SHAPE('',$,#59328);
#59241=PRODUCT_DEFINITION_SHAPE('',$,#59329);
#59242=PRODUCT_DEFINITION_SHAPE('',$,#59330);
#59243=PRODUCT_DEFINITION_SHAPE('',$,#59331);
#59244=PRODUCT_DEFINITION_SHAPE('',$,#59332);
#59245=PRODUCT_DEFINITION_SHAPE('',$,#59333);
#59246=PRODUCT_DEFINITION_SHAPE('',$,#59334);
#59247=PRODUCT_DEFINITION_SHAPE('',$,#59335);
#59248=PRODUCT_DEFINITION_SHAPE('',$,#59336);
#59249=PRODUCT_DEFINITION_SHAPE('',$,#59337);
#59250=PRODUCT_DEFINITION_SHAPE('',$,#59338);
#59251=PRODUCT_DEFINITION_SHAPE($,$,#146);
#59252=PRODUCT_DEFINITION_SHAPE($,$,#147);
#59253=PRODUCT_DEFINITION_SHAPE($,$,#148);
#59254=PRODUCT_DEFINITION_SHAPE($,$,#149);
#59255=PRODUCT_DEFINITION_SHAPE($,$,#150);
#59256=PRODUCT_DEFINITION_SHAPE($,$,#151);
#59257=PRODUCT_DEFINITION_SHAPE($,$,#152);
#59258=PRODUCT_DEFINITION_SHAPE($,$,#153);
#59259=PRODUCT_DEFINITION_SHAPE($,$,#154);
#59260=PRODUCT_DEFINITION_SHAPE($,$,#155);
#59261=PRODUCT_DEFINITION_SHAPE($,$,#156);
#59262=PRODUCT_DEFINITION_SHAPE($,$,#157);
#59263=PRODUCT_DEFINITION_SHAPE($,$,#158);
#59264=PRODUCT_DEFINITION_SHAPE($,$,#159);
#59265=PRODUCT_DEFINITION_SHAPE($,$,#160);
#59266=PRODUCT_DEFINITION_SHAPE($,$,#161);
#59267=PRODUCT_DEFINITION_SHAPE($,$,#162);
#59268=PRODUCT_DEFINITION_SHAPE($,$,#163);
#59269=PRODUCT_DEFINITION_SHAPE($,$,#164);
#59270=PRODUCT_DEFINITION_SHAPE($,$,#165);
#59271=PRODUCT_DEFINITION_SHAPE($,$,#166);
#59272=PRODUCT_DEFINITION_SHAPE($,$,#167);
#59273=PRODUCT_DEFINITION_SHAPE($,$,#168);
#59274=PRODUCT_DEFINITION_SHAPE($,$,#169);
#59275=PRODUCT_DEFINITION_SHAPE($,$,#170);
#59276=PRODUCT_DEFINITION_SHAPE($,$,#171);
#59277=PRODUCT_DEFINITION_SHAPE($,$,#172);
#59278=PRODUCT_DEFINITION_SHAPE($,$,#173);
#59279=PRODUCT_DEFINITION_SHAPE($,$,#174);
#59280=PRODUCT_DEFINITION_SHAPE($,$,#175);
#59281=PRODUCT_DEFINITION_SHAPE($,$,#176);
#59282=PRODUCT_DEFINITION_SHAPE($,$,#177);
#59283=PRODUCT_DEFINITION_SHAPE($,$,#178);
#59284=PRODUCT_DEFINITION_SHAPE($,$,#179);
#59285=PRODUCT_DEFINITION_SHAPE($,$,#180);
#59286=PRODUCT_DEFINITION_SHAPE($,$,#181);
#59287=PRODUCT_DEFINITION_SHAPE($,$,#182);
#59288=PRODUCT_DEFINITION_SHAPE($,$,#183);
#59289=PRODUCT_DEFINITION_SHAPE($,$,#184);
#59290=PRODUCT_DEFINITION_SHAPE($,$,#185);
#59291=PRODUCT_DEFINITION_SHAPE($,$,#186);
#59292=PRODUCT_DEFINITION_SHAPE($,$,#187);
#59293=PRODUCT_DEFINITION_SHAPE($,$,#188);
#59294=PRODUCT_DEFINITION_SHAPE($,$,#189);
#59295=PRODUCT_DEFINITION_SHAPE($,$,#190);
#59296=SHAPE_REPRESENTATION('',(#23045,#25071,#25072,#25073,#25074,#25075,
#25076,#25077,#25078,#25079,#25080,#25081,#25082,#25083,#25084,#25085,#25086,
#25087,#25088,#25089,#25090,#25091,#25092,#25093,#25094,#25095,#25096,#25097,
#25098,#25099,#25100,#25101,#25102,#25103,#25104,#25105,#25106,#25107,#25108,
#25109,#25110,#25111,#25112,#25113,#25114,#25115),#59183);
#59297=SHAPE_REPRESENTATION('',(#23046),#59184);
#59298=SHAPE_REPRESENTATION('',(#23123),#59185);
#59299=SHAPE_REPRESENTATION('',(#23145),#59186);
#59300=SHAPE_REPRESENTATION('',(#23166),#59187);
#59301=SHAPE_REPRESENTATION('',(#23174),#59188);
#59302=SHAPE_REPRESENTATION('',(#23191),#59189);
#59303=SHAPE_REPRESENTATION('',(#23228),#59190);
#59304=SHAPE_REPRESENTATION('',(#23491),#59191);
#59305=SHAPE_REPRESENTATION('',(#23559),#59192);
#59306=SHAPE_REPRESENTATION('',(#23609),#59193);
#59307=SHAPE_REPRESENTATION('',(#23720),#59194);
#59308=SHAPE_REPRESENTATION('',(#23866),#59195);
#59309=SHAPE_REPRESENTATION('',(#23996),#59196);
#59310=SHAPE_REPRESENTATION('',(#24159),#59197);
#59311=SHAPE_REPRESENTATION('',(#24197),#59198);
#59312=SHAPE_REPRESENTATION('',(#24231),#59199);
#59313=SHAPE_REPRESENTATION('',(#24619),#59200);
#59314=SHAPE_REPRESENTATION('',(#24636),#59201);
#59315=SHAPE_REPRESENTATION('',(#24661),#59202);
#59316=SHAPE_REPRESENTATION('',(#24996),#59203);
#59317=PRODUCT_DEFINITION_CONTEXT('part definition',#59382,'design');
#59318=PRODUCT_DEFINITION('2026-10-23-00-46-48-583','MAS-332',#59339,
#59317);
#59319=PRODUCT_DEFINITION('2026-10-23-00-47-18-389',
'08_Slipper_Retainer_Plate',#59340,#59317);
#59320=PRODUCT_DEFINITION('2026-10-23-00-47-19-123',
'09_Spherical_Ball_Guide_SR16',#59341,#59317);
#59321=PRODUCT_DEFINITION('2026-10-23-00-47-19-372',
'10_Swashplate_15deg',#59342,#59317);
#59322=PRODUCT_DEFINITION('2026-10-23-00-47-20-071',
'11_Block_Hold-Down_Spring_3x33x24.5',#59343,#59317);
#59323=PRODUCT_DEFINITION('2026-10-23-00-47-21-965',
'16_DIN_6885_A_8x7x16_Parallel_Key',#59344,#59317);
#59324=PRODUCT_DEFINITION('2026-10-23-00-47-22-996',
'14_DIN_3760_A_25x40x7_NBR_Lip_Seal',#59345,#59317);
#59325=PRODUCT_DEFINITION('2026-10-23-00-47-37-044',
'18_Pressure_Relief_Valve_Plug_G3-8_AF22',#59346,#59317);
#59326=PRODUCT_DEFINITION('2026-10-23-00-47-48-451',
'19_Case_Drain_Fitting_DIN_2353_GE08-LR_G1-4',#59347,#59317);
#59327=PRODUCT_DEFINITION('2026-10-23-00-47-53-406',
'04_Drive_Shaft_D25_Keyed_42CrMo4',#59348,#59317);
#59328=PRODUCT_DEFINITION('2026-10-23-00-47-55-837',
'05_Rotary_Cylinder_Block_9xD12',#59349,#59317);
#59329=PRODUCT_DEFINITION('2026-10-23-00-48-09-036',
'01_Front_Housing_Pump_Casing_D100_Flange_D140',#59350,#59317);
#59330=PRODUCT_DEFINITION('2026-10-23-00-48-16-141',
'02_Valve_Port_Plate_D140x24_Kidney_Ports',#59351,#59317);
#59331=PRODUCT_DEFINITION('2026-10-23-00-48-24-882',
'03_Rear_End_Cover_D140_Bearing_Housing',#59352,#59317);
#59332=PRODUCT_DEFINITION('2026-10-23-00-47-08-320',
'06_Axial_Piston_D12_Ball_End_SR4.5',#59353,#59317);
#59333=PRODUCT_DEFINITION('2026-10-23-00-47-18-058',
'07_Slipper_Shoe_D16_Bronze',#59354,#59317);
#59334=PRODUCT_DEFINITION('2026-10-23-00-47-28-876',
'12_Taper_Roller_Bearing_30205_Cone_Assembly',#59355,#59317);
#59335=PRODUCT_DEFINITION('2026-10-23-00-47-30-002',
'13_Taper_Roller_Bearing_30205_Cup',#59356,#59317);
#59336=PRODUCT_DEFINITION('2026-10-23-00-47-22-382',
'15_DIN_471_25x1.2_Retaining_Ring',#59357,#59317);
#59337=PRODUCT_DEFINITION('2026-10-23-00-47-30-365',
'17_ISO_4762_M8x45-12.9_Socket_Head_Screw',#59358,#59317);
#59338=PRODUCT_DEFINITION('2026-10-23-00-47-50-726',
'20_Port_Connector_DIN_2353_GE10-LR_G3-8',#59359,#59317);
#59339=PRODUCT_DEFINITION_FORMATION('',$,#59384);
#59340=PRODUCT_DEFINITION_FORMATION('',$,#59385);
#59341=PRODUCT_DEFINITION_FORMATION('',$,#59386);
#59342=PRODUCT_DEFINITION_FORMATION('',$,#59387);
#59343=PRODUCT_DEFINITION_FORMATION('',$,#59388);
#59344=PRODUCT_DEFINITION_FORMATION('',$,#59389);
#59345=PRODUCT_DEFINITION_FORMATION('',$,#59390);
#59346=PRODUCT_DEFINITION_FORMATION('',$,#59391);
#59347=PRODUCT_DEFINITION_FORMATION('',$,#59392);
#59348=PRODUCT_DEFINITION_FORMATION('',$,#59393);
#59349=PRODUCT_DEFINITION_FORMATION('',$,#59394);
#59350=PRODUCT_DEFINITION_FORMATION('',$,#59395);
#59351=PRODUCT_DEFINITION_FORMATION('',$,#59396);
#59352=PRODUCT_DEFINITION_FORMATION('',$,#59397);
#59353=PRODUCT_DEFINITION_FORMATION('',$,#59398);
#59354=PRODUCT_DEFINITION_FORMATION('',$,#59399);
#59355=PRODUCT_DEFINITION_FORMATION('',$,#59400);
#59356=PRODUCT_DEFINITION_FORMATION('',$,#59401);
#59357=PRODUCT_DEFINITION_FORMATION('',$,#59402);
#59358=PRODUCT_DEFINITION_FORMATION('',$,#59403);
#59359=PRODUCT_DEFINITION_FORMATION('',$,#59404);
#59360=PRODUCT_RELATED_PRODUCT_CATEGORY('MAS-332','MAS-332',(#59384));
#59361=PRODUCT_RELATED_PRODUCT_CATEGORY('08_Slipper_Retainer_Plate',
'08_Slipper_Retainer_Plate',(#59385));
#59362=PRODUCT_RELATED_PRODUCT_CATEGORY('09_Spherical_Ball_Guide_SR16',
'09_Spherical_Ball_Guide_SR16',(#59386));
#59363=PRODUCT_RELATED_PRODUCT_CATEGORY('10_Swashplate_15deg',
'10_Swashplate_15deg',(#59387));
#59364=PRODUCT_RELATED_PRODUCT_CATEGORY(
'11_Block_Hold-Down_Spring_3x33x24.5',
'11_Block_Hold-Down_Spring_3x33x24.5',(#59388));
#59365=PRODUCT_RELATED_PRODUCT_CATEGORY(
'16_DIN_6885_A_8x7x16_Parallel_Key','16_DIN_6885_A_8x7x16_Parallel_Key',
(#59389));
#59366=PRODUCT_RELATED_PRODUCT_CATEGORY(
'14_DIN_3760_A_25x40x7_NBR_Lip_Seal',
'14_DIN_3760_A_25x40x7_NBR_Lip_Seal',(#59390));
#59367=PRODUCT_RELATED_PRODUCT_CATEGORY(
'18_Pressure_Relief_Valve_Plug_G3-8_AF22',
'18_Pressure_Relief_Valve_Plug_G3-8_AF22',(#59391));
#59368=PRODUCT_RELATED_PRODUCT_CATEGORY(
'19_Case_Drain_Fitting_DIN_2353_GE08-LR_G1-4',
'19_Case_Drain_Fitting_DIN_2353_GE08-LR_G1-4',(#59392));
#59369=PRODUCT_RELATED_PRODUCT_CATEGORY(
'04_Drive_Shaft_D25_Keyed_42CrMo4','04_Drive_Shaft_D25_Keyed_42CrMo4',(#59393));
#59370=PRODUCT_RELATED_PRODUCT_CATEGORY(
'05_Rotary_Cylinder_Block_9xD12','05_Rotary_Cylinder_Block_9xD12',(#59394));
#59371=PRODUCT_RELATED_PRODUCT_CATEGORY(
'01_Front_Housing_Pump_Casing_D100_Flange_D140',
'01_Front_Housing_Pump_Casing_D100_Flange_D140',(#59395));
#59372=PRODUCT_RELATED_PRODUCT_CATEGORY(
'02_Valve_Port_Plate_D140x24_Kidney_Ports',
'02_Valve_Port_Plate_D140x24_Kidney_Ports',(#59396));
#59373=PRODUCT_RELATED_PRODUCT_CATEGORY(
'03_Rear_End_Cover_D140_Bearing_Housing',
'03_Rear_End_Cover_D140_Bearing_Housing',(#59397));
#59374=PRODUCT_RELATED_PRODUCT_CATEGORY(
'06_Axial_Piston_D12_Ball_End_SR4.5',
'06_Axial_Piston_D12_Ball_End_SR4.5',(#59398));
#59375=PRODUCT_RELATED_PRODUCT_CATEGORY('07_Slipper_Shoe_D16_Bronze',
'07_Slipper_Shoe_D16_Bronze',(#59399));
#59376=PRODUCT_RELATED_PRODUCT_CATEGORY(
'12_Taper_Roller_Bearing_30205_Cone_Assembly',
'12_Taper_Roller_Bearing_30205_Cone_Assembly',(#59400));
#59377=PRODUCT_RELATED_PRODUCT_CATEGORY(
'13_Taper_Roller_Bearing_30205_Cup','13_Taper_Roller_Bearing_30205_Cup',
(#59401));
#59378=PRODUCT_RELATED_PRODUCT_CATEGORY(
'15_DIN_471_25x1.2_Retaining_Ring','15_DIN_471_25x1.2_Retaining_Ring',(#59402));
#59379=PRODUCT_RELATED_PRODUCT_CATEGORY(
'17_ISO_4762_M8x45-12.9_Socket_Head_Screw',
'17_ISO_4762_M8x45-12.9_Socket_Head_Screw',(#59403));
#59380=PRODUCT_RELATED_PRODUCT_CATEGORY(
'20_Port_Connector_DIN_2353_GE10-LR_G3-8',
'20_Port_Connector_DIN_2353_GE10-LR_G3-8',(#59404));
#59381=APPLICATION_PROTOCOL_DEFINITION('international standard',
'automotive_design',2009,#59382);
#59382=APPLICATION_CONTEXT(
'Core Data for Automotive Mechanical Design Process');
#59383=PRODUCT_CONTEXT('part definition',#59382,'mechanical');
#59384=PRODUCT('2026-10-23-00-46-48-583','MAS-332',$,(#59383));
#59385=PRODUCT('2026-10-23-00-47-18-389','08_Slipper_Retainer_Plate',$,
(#59383));
#59386=PRODUCT('2026-10-23-00-47-19-123','09_Spherical_Ball_Guide_SR16',
$,(#59383));
#59387=PRODUCT('2026-10-23-00-47-19-372','10_Swashplate_15deg',$,(#59383));
#59388=PRODUCT('2026-10-23-00-47-20-071',
'11_Block_Hold-Down_Spring_3x33x24.5',$,(#59383));
#59389=PRODUCT('2026-10-23-00-47-21-965',
'16_DIN_6885_A_8x7x16_Parallel_Key',$,(#59383));
#59390=PRODUCT('2026-10-23-00-47-22-996',
'14_DIN_3760_A_25x40x7_NBR_Lip_Seal',$,(#59383));
#59391=PRODUCT('2026-10-23-00-47-37-044',
'18_Pressure_Relief_Valve_Plug_G3-8_AF22',$,(#59383));
#59392=PRODUCT('2026-10-23-00-47-48-451',
'19_Case_Drain_Fitting_DIN_2353_GE08-LR_G1-4',$,(#59383));
#59393=PRODUCT('2026-10-23-00-47-53-406',
'04_Drive_Shaft_D25_Keyed_42CrMo4',$,(#59383));
#59394=PRODUCT('2026-10-23-00-47-55-837',
'05_Rotary_Cylinder_Block_9xD12',$,(#59383));
#59395=PRODUCT('2026-10-23-00-48-09-036',
'01_Front_Housing_Pump_Casing_D100_Flange_D140',$,(#59383));
#59396=PRODUCT('2026-10-23-00-48-16-141',
'02_Valve_Port_Plate_D140x24_Kidney_Ports',$,(#59383));
#59397=PRODUCT('2026-10-23-00-48-24-882',
'03_Rear_End_Cover_D140_Bearing_Housing',$,(#59383));
#59398=PRODUCT('2026-10-23-00-47-08-320',
'06_Axial_Piston_D12_Ball_End_SR4.5',$,(#59383));
#59399=PRODUCT('2026-10-23-00-47-18-058','07_Slipper_Shoe_D16_Bronze',$,
(#59383));
#59400=PRODUCT('2026-10-23-00-47-28-876',
'12_Taper_Roller_Bearing_30205_Cone_Assembly',$,(#59383));
#59401=PRODUCT('2026-10-23-00-47-30-002',
'13_Taper_Roller_Bearing_30205_Cup',$,(#59383));
#59402=PRODUCT('2026-10-23-00-47-22-382',
'15_DIN_471_25x1.2_Retaining_Ring',$,(#59383));
#59403=PRODUCT('2026-10-23-00-47-30-365',
'17_ISO_4762_M8x45-12.9_Socket_Head_Screw',$,(#59383));
#59404=PRODUCT('2026-10-23-00-47-50-726',
'20_Port_Connector_DIN_2353_GE10-LR_G3-8',$,(#59383));
#59405=PRESENTATION_STYLE_ASSIGNMENT((#59427));
#59406=PRESENTATION_STYLE_ASSIGNMENT((#59428));
#59407=PRESENTATION_STYLE_ASSIGNMENT((#59429));
#59408=PRESENTATION_STYLE_ASSIGNMENT((#59430));
#59409=PRESENTATION_STYLE_ASSIGNMENT((#59431));
#59410=PRESENTATION_STYLE_ASSIGNMENT((#59432));
#59411=PRESENTATION_STYLE_ASSIGNMENT((#59433));
#59412=PRESENTATION_STYLE_ASSIGNMENT((#59434));
#59413=PRESENTATION_STYLE_ASSIGNMENT((#59435));
#59414=PRESENTATION_STYLE_ASSIGNMENT((#59436));
#59415=PRESENTATION_STYLE_ASSIGNMENT((#59437));
#59416=PRESENTATION_STYLE_ASSIGNMENT((#59438));
#59417=PRESENTATION_STYLE_ASSIGNMENT((#59439));
#59418=PRESENTATION_STYLE_ASSIGNMENT((#59440));
#59419=PRESENTATION_STYLE_ASSIGNMENT((#59441));
#59420=PRESENTATION_STYLE_ASSIGNMENT((#59442));
#59421=PRESENTATION_STYLE_ASSIGNMENT((#59443));
#59422=PRESENTATION_STYLE_ASSIGNMENT((#59444));
#59423=PRESENTATION_STYLE_ASSIGNMENT((#59445));
#59424=PRESENTATION_STYLE_ASSIGNMENT((#59446));
#59425=PRESENTATION_STYLE_ASSIGNMENT((#59447));
#59426=PRESENTATION_STYLE_ASSIGNMENT((#59448));
#59427=SURFACE_STYLE_USAGE(.BOTH.,#59449);
#59428=SURFACE_STYLE_USAGE(.BOTH.,#59450);
#59429=SURFACE_STYLE_USAGE(.BOTH.,#59451);
#59430=SURFACE_STYLE_USAGE(.BOTH.,#59452);
#59431=SURFACE_STYLE_USAGE(.BOTH.,#59453);
#59432=SURFACE_STYLE_USAGE(.BOTH.,#59454);
#59433=SURFACE_STYLE_USAGE(.BOTH.,#59455);
#59434=SURFACE_STYLE_USAGE(.BOTH.,#59456);
#59435=SURFACE_STYLE_USAGE(.BOTH.,#59457);
#59436=SURFACE_STYLE_USAGE(.BOTH.,#59458);
#59437=SURFACE_STYLE_USAGE(.BOTH.,#59459);
#59438=SURFACE_STYLE_USAGE(.BOTH.,#59460);
#59439=SURFACE_STYLE_USAGE(.BOTH.,#59461);
#59440=SURFACE_STYLE_USAGE(.BOTH.,#59462);
#59441=SURFACE_STYLE_USAGE(.BOTH.,#59463);
#59442=SURFACE_STYLE_USAGE(.BOTH.,#59464);
#59443=SURFACE_STYLE_USAGE(.BOTH.,#59465);
#59444=SURFACE_STYLE_USAGE(.BOTH.,#59466);
#59445=SURFACE_STYLE_USAGE(.BOTH.,#59467);
#59446=SURFACE_STYLE_USAGE(.BOTH.,#59468);
#59447=SURFACE_STYLE_USAGE(.BOTH.,#59469);
#59448=SURFACE_STYLE_USAGE(.BOTH.,#59470);
#59449=SURFACE_SIDE_STYLE('',(#59471));
#59450=SURFACE_SIDE_STYLE('',(#59472));
#59451=SURFACE_SIDE_STYLE('',(#59473));
#59452=SURFACE_SIDE_STYLE('',(#59474));
#59453=SURFACE_SIDE_STYLE('',(#59475));
#59454=SURFACE_SIDE_STYLE('',(#59476));
#59455=SURFACE_SIDE_STYLE('',(#59477));
#59456=SURFACE_SIDE_STYLE('',(#59478));
#59457=SURFACE_SIDE_STYLE('',(#59479));
#59458=SURFACE_SIDE_STYLE('',(#59480));
#59459=SURFACE_SIDE_STYLE('',(#59481));
#59460=SURFACE_SIDE_STYLE('',(#59482));
#59461=SURFACE_SIDE_STYLE('',(#59483));
#59462=SURFACE_SIDE_STYLE('',(#59484));
#59463=SURFACE_SIDE_STYLE('',(#59485));
#59464=SURFACE_SIDE_STYLE('',(#59486));
#59465=SURFACE_SIDE_STYLE('',(#59487));
#59466=SURFACE_SIDE_STYLE('',(#59488));
#59467=SURFACE_SIDE_STYLE('',(#59489));
#59468=SURFACE_SIDE_STYLE('',(#59490));
#59469=SURFACE_SIDE_STYLE('',(#59491));
#59470=SURFACE_SIDE_STYLE('',(#59492));
#59471=SURFACE_STYLE_FILL_AREA(#59493);
#59472=SURFACE_STYLE_FILL_AREA(#59494);
#59473=SURFACE_STYLE_FILL_AREA(#59495);
#59474=SURFACE_STYLE_FILL_AREA(#59496);
#59475=SURFACE_STYLE_FILL_AREA(#59497);
#59476=SURFACE_STYLE_FILL_AREA(#59498);
#59477=SURFACE_STYLE_FILL_AREA(#59499);
#59478=SURFACE_STYLE_FILL_AREA(#59500);
#59479=SURFACE_STYLE_FILL_AREA(#59501);
#59480=SURFACE_STYLE_FILL_AREA(#59502);
#59481=SURFACE_STYLE_FILL_AREA(#59503);
#59482=SURFACE_STYLE_FILL_AREA(#59504);
#59483=SURFACE_STYLE_FILL_AREA(#59505);
#59484=SURFACE_STYLE_FILL_AREA(#59506);
#59485=SURFACE_STYLE_FILL_AREA(#59507);
#59486=SURFACE_STYLE_FILL_AREA(#59508);
#59487=SURFACE_STYLE_FILL_AREA(#59509);
#59488=SURFACE_STYLE_FILL_AREA(#59510);
#59489=SURFACE_STYLE_FILL_AREA(#59511);
#59490=SURFACE_STYLE_FILL_AREA(#59512);
#59491=SURFACE_STYLE_FILL_AREA(#59513);
#59492=SURFACE_STYLE_FILL_AREA(#59514);
#59493=FILL_AREA_STYLE('Steel - Satin',(#59515));
#59494=FILL_AREA_STYLE('MAS332_ret',(#59516));
#59495=FILL_AREA_STYLE('MAS332_guide',(#59517));
#59496=FILL_AREA_STYLE('MAS332_swash',(#59518));
#59497=FILL_AREA_STYLE('MAS332_spr',(#59519));
#59498=FILL_AREA_STYLE('MAS332_key',(#59520));
#59499=FILL_AREA_STYLE('MAS332_seal',(#59521));
#59500=FILL_AREA_STYLE('MAS332_rv',(#59522));
#59501=FILL_AREA_STYLE('MAS332_drain',(#59523));
#59502=FILL_AREA_STYLE('MAS332_shaft',(#59524));
#59503=FILL_AREA_STYLE('MAS332_block',(#59525));
#59504=FILL_AREA_STYLE('MAS332_house',(#59526));
#59505=FILL_AREA_STYLE('MAS332_machined_face',(#59527));
#59506=FILL_AREA_STYLE('MAS332_plate',(#59528));
#59507=FILL_AREA_STYLE('MAS332_cover',(#59529));
#59508=FILL_AREA_STYLE('MAS332_piston',(#59530));
#59509=FILL_AREA_STYLE('MAS332_slip',(#59531));
#59510=FILL_AREA_STYLE('MAS332_cone',(#59532));
#59511=FILL_AREA_STYLE('MAS332_cup',(#59533));
#59512=FILL_AREA_STYLE('MAS332_circ',(#59534));
#59513=FILL_AREA_STYLE('MAS332_scr',(#59535));
#59514=FILL_AREA_STYLE('MAS332_port',(#59536));
#59515=FILL_AREA_STYLE_COLOUR('Steel - Satin',#59537);
#59516=FILL_AREA_STYLE_COLOUR('MAS332_ret',#59538);
#59517=FILL_AREA_STYLE_COLOUR('MAS332_guide',#59539);
#59518=FILL_AREA_STYLE_COLOUR('MAS332_swash',#59540);
#59519=FILL_AREA_STYLE_COLOUR('MAS332_spr',#59541);
#59520=FILL_AREA_STYLE_COLOUR('MAS332_key',#59542);
#59521=FILL_AREA_STYLE_COLOUR('MAS332_seal',#59543);
#59522=FILL_AREA_STYLE_COLOUR('MAS332_rv',#59544);
#59523=FILL_AREA_STYLE_COLOUR('MAS332_drain',#59545);
#59524=FILL_AREA_STYLE_COLOUR('MAS332_shaft',#59546);
#59525=FILL_AREA_STYLE_COLOUR('MAS332_block',#59547);
#59526=FILL_AREA_STYLE_COLOUR('MAS332_house',#59548);
#59527=FILL_AREA_STYLE_COLOUR('MAS332_machined_face',#59549);
#59528=FILL_AREA_STYLE_COLOUR('MAS332_plate',#59550);
#59529=FILL_AREA_STYLE_COLOUR('MAS332_cover',#59551);
#59530=FILL_AREA_STYLE_COLOUR('MAS332_piston',#59552);
#59531=FILL_AREA_STYLE_COLOUR('MAS332_slip',#59553);
#59532=FILL_AREA_STYLE_COLOUR('MAS332_cone',#59554);
#59533=FILL_AREA_STYLE_COLOUR('MAS332_cup',#59555);
#59534=FILL_AREA_STYLE_COLOUR('MAS332_circ',#59556);
#59535=FILL_AREA_STYLE_COLOUR('MAS332_scr',#59557);
#59536=FILL_AREA_STYLE_COLOUR('MAS332_port',#59558);
#59537=COLOUR_RGB('Steel - Satin',0.627450980392157,0.627450980392157,0.627450980392157);
#59538=COLOUR_RGB('MAS332_ret',0.807843137254902,0.627450980392157,0.149019607843137);
#59539=COLOUR_RGB('MAS332_guide',0.83921568627451,0.850980392156863,0.870588235294118);
#59540=COLOUR_RGB('MAS332_swash',0.588235294117647,0.6,0.615686274509804);
#59541=COLOUR_RGB('MAS332_spr',0.8,0.811764705882353,0.831372549019608);
#59542=COLOUR_RGB('MAS332_key',0.831372549019608,0.843137254901961,0.862745098039216);
#59543=COLOUR_RGB('MAS332_seal',0.156862745098039,0.156862745098039,0.164705882352941);
#59544=COLOUR_RGB('MAS332_rv',0.768627450980392,0.784313725490196,0.807843137254902);
#59545=COLOUR_RGB('MAS332_drain',0.776470588235294,0.792156862745098,0.815686274509804);
#59546=COLOUR_RGB('MAS332_shaft',0.815686274509804,0.827450980392157,0.847058823529412);
#59547=COLOUR_RGB('MAS332_block',0.886274509803922,0.501960784313725,0.501960784313725);
#59548=COLOUR_RGB('MAS332_house',0.109803921568627,0.454901960784314,0.745098039215686);
#59549=COLOUR_RGB('MAS332_machined_face',0.690196078431373,0.705882352941177,
0.729411764705882);
#59550=COLOUR_RGB('MAS332_plate',0.886274509803922,0.894117647058824,0.905882352941176);
#59551=COLOUR_RGB('MAS332_cover',0.125490196078431,0.470588235294118,0.76078431372549);
#59552=COLOUR_RGB('MAS332_piston',0.925490196078431,0.933333333333333,0.945098039215686);
#59553=COLOUR_RGB('MAS332_slip',0.83921568627451,0.658823529411765,0.180392156862745);
#59554=COLOUR_RGB('MAS332_cone',0.870588235294118,0.768627450980392,0.611764705882353);
#59555=COLOUR_RGB('MAS332_cup',0.776470588235294,0.788235294117647,0.807843137254902);
#59556=COLOUR_RGB('MAS332_circ',0.588235294117647,0.6,0.615686274509804);
#59557=COLOUR_RGB('MAS332_scr',0.784313725490196,0.8,0.819607843137255);
#59558=COLOUR_RGB('MAS332_port',0.792156862745098,0.807843137254902,0.823529411764706);
#59559=COLOUR_RGB('Dark Blue',0.08,0.2,0.34);
#59560=FILL_AREA_STYLE_COLOUR('',#59559);
#59561=FILL_AREA_STYLE('',(#59560));
#59562=SURFACE_STYLE_FILL_AREA(#59561);
#59563=SURFACE_SIDE_STYLE('',(#59562));
#59564=SURFACE_STYLE_USAGE(.BOTH.,#59563);
#59565=PRESENTATION_STYLE_ASSIGNMENT((#59564));
#59566=COLOUR_RGB('Light Blue',0.38,0.62,0.78);
#59567=FILL_AREA_STYLE_COLOUR('',#59566);
#59568=FILL_AREA_STYLE('',(#59567));
#59569=SURFACE_STYLE_FILL_AREA(#59568);
#59570=SURFACE_SIDE_STYLE('',(#59569));
#59571=SURFACE_STYLE_USAGE(.BOTH.,#59570);
#59572=PRESENTATION_STYLE_ASSIGNMENT((#59571));
#59573=COLOUR_RGB('Sky Blue',0.24,0.69,0.87);
#59574=FILL_AREA_STYLE_COLOUR('',#59573);
#59575=FILL_AREA_STYLE('',(#59574));
#59576=SURFACE_STYLE_FILL_AREA(#59575);
#59577=SURFACE_SIDE_STYLE('',(#59576));
#59578=SURFACE_STYLE_USAGE(.BOTH.,#59577);
#59579=PRESENTATION_STYLE_ASSIGNMENT((#59578));
#59580=COLOUR_RGB('Grey',0.48,0.52,0.57);
#59581=FILL_AREA_STYLE_COLOUR('',#59580);
#59582=FILL_AREA_STYLE('',(#59581));
#59583=SURFACE_STYLE_FILL_AREA(#59582);
#59584=SURFACE_SIDE_STYLE('',(#59583));
#59585=SURFACE_STYLE_USAGE(.BOTH.,#59584);
#59586=PRESENTATION_STYLE_ASSIGNMENT((#59585));
#59587=COLOUR_RGB('Black',0.12,0.14,0.17);
#59588=FILL_AREA_STYLE_COLOUR('',#59587);
#59589=FILL_AREA_STYLE('',(#59588));
#59590=SURFACE_STYLE_FILL_AREA(#59589);
#59591=SURFACE_SIDE_STYLE('',(#59590));
#59592=SURFACE_STYLE_USAGE(.BOTH.,#59591);
#59593=PRESENTATION_STYLE_ASSIGNMENT((#59592));
#59594=COLOUR_RGB('Off White',0.89,0.88,0.83);
#59595=FILL_AREA_STYLE_COLOUR('',#59594);
#59596=FILL_AREA_STYLE('',(#59595));
#59597=SURFACE_STYLE_FILL_AREA(#59596);
#59598=SURFACE_SIDE_STYLE('',(#59597));
#59599=SURFACE_STYLE_USAGE(.BOTH.,#59598);
#59600=PRESENTATION_STYLE_ASSIGNMENT((#59599));
ENDSEC;
END-ISO-10303-21;
